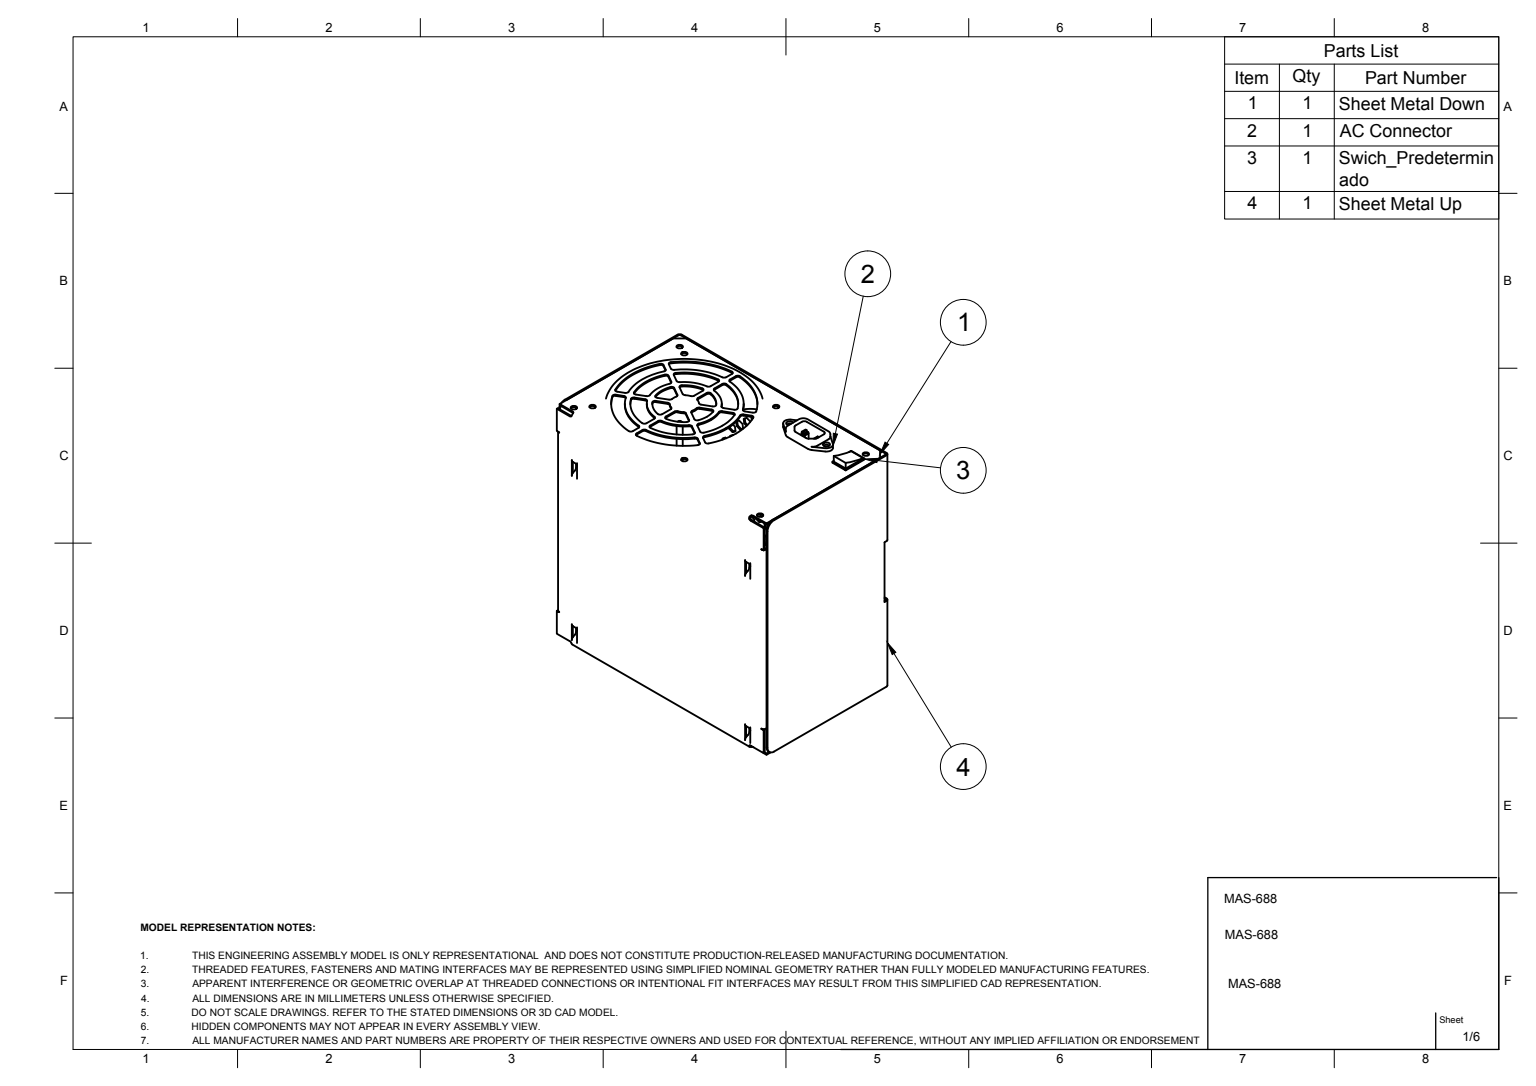
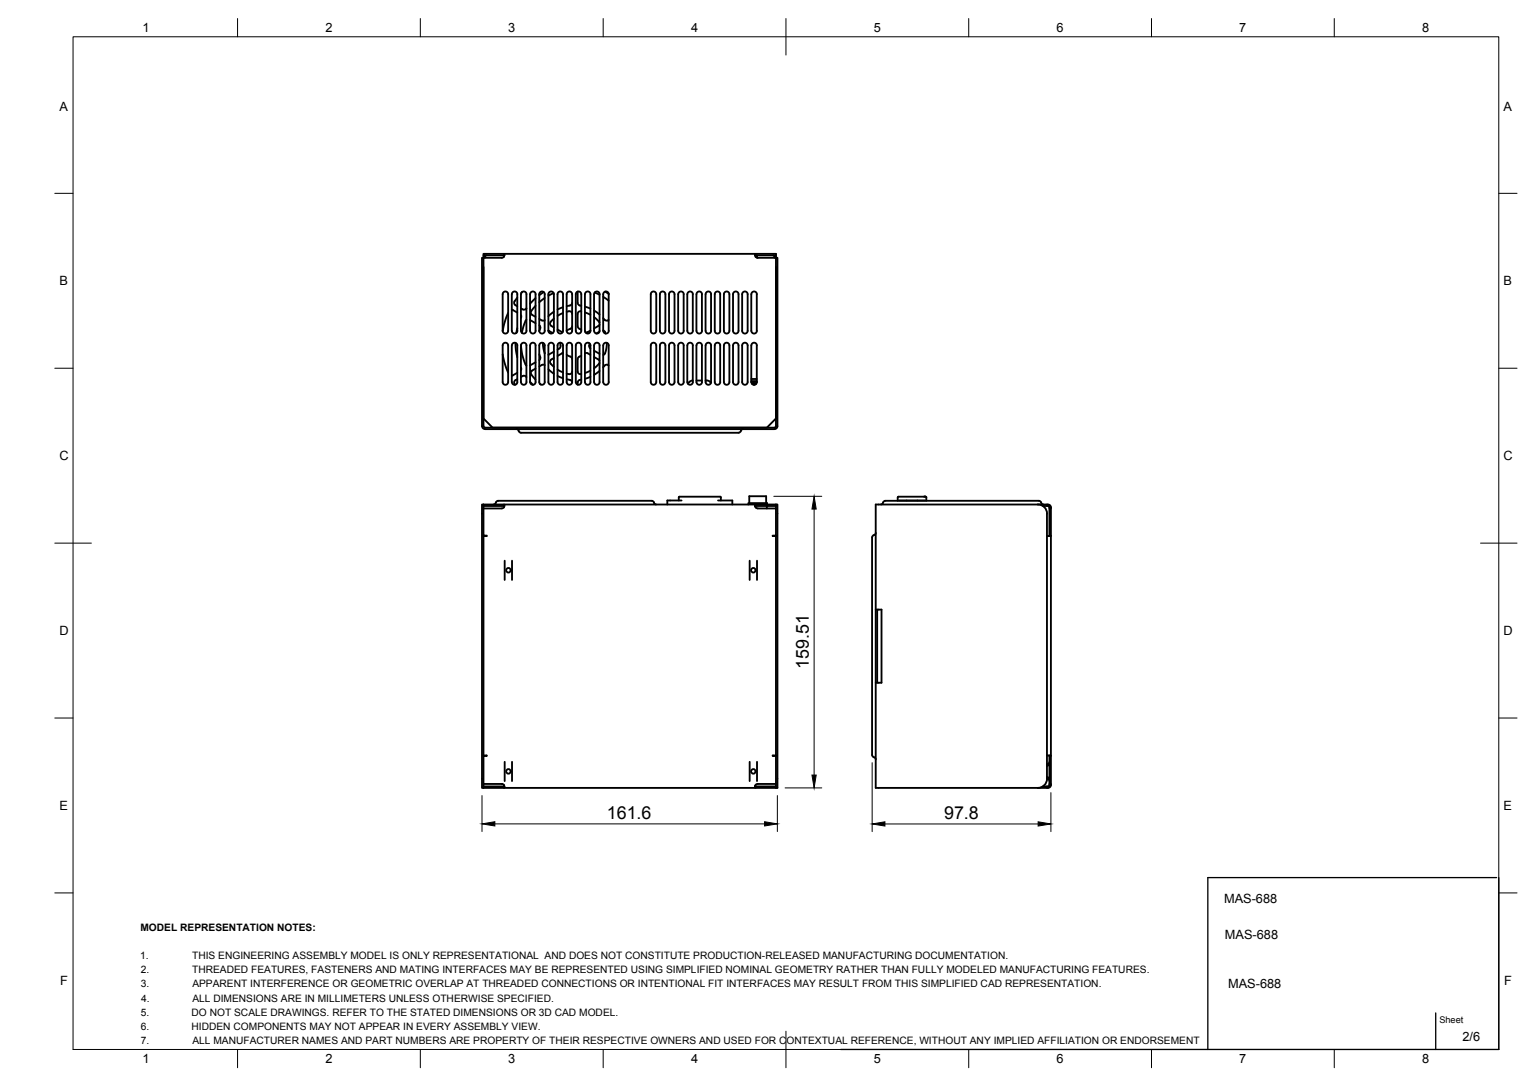
ISO-10303-21;
HEADER;
/* Generated by software containing ST-Developer
 * from STEP Tools, Inc. (www.steptools.com) 
 */

FILE_DESCRIPTION(
/* description */ ('STEP AP214'),
/* implementation_level */ '2;1');

FILE_NAME(
/* name */ 'MAS-688.step',
/* time_stamp */ '2026-11-14T03:58:36-08:00',
/* author */ (''),
/* organization */ (''),
/* preprocessor_version */ 'ST-DEVELOPER v20.2',
/* originating_system */ 'Autodesk Translation Framework v15.17.0.0',
/* authorisation */ '');

FILE_SCHEMA (('AUTOMOTIVE_DESIGN { 1 0 10303 214 3 1 1 }'));
ENDSEC;

DATA;
#10=MECHANICAL_DESIGN_GEOMETRIC_PRESENTATION_REPRESENTATION('',(#41,#42,
#43,#44),#65304);
#11=ITEM_DEFINED_TRANSFORMATION($,$,#39984,#42510);
#12=ITEM_DEFINED_TRANSFORMATION($,$,#41041,#42511);
#13=ITEM_DEFINED_TRANSFORMATION($,$,#41224,#42512);
#14=ITEM_DEFINED_TRANSFORMATION($,$,#41307,#42513);
#15=(
REPRESENTATION_RELATIONSHIP($,$,#65324,#65323)
REPRESENTATION_RELATIONSHIP_WITH_TRANSFORMATION(#11)
SHAPE_REPRESENTATION_RELATIONSHIP()
);
#16=(
REPRESENTATION_RELATIONSHIP($,$,#65325,#65323)
REPRESENTATION_RELATIONSHIP_WITH_TRANSFORMATION(#12)
SHAPE_REPRESENTATION_RELATIONSHIP()
);
#17=(
REPRESENTATION_RELATIONSHIP($,$,#65326,#65323)
REPRESENTATION_RELATIONSHIP_WITH_TRANSFORMATION(#13)
SHAPE_REPRESENTATION_RELATIONSHIP()
);
#18=(
REPRESENTATION_RELATIONSHIP($,$,#65327,#65323)
REPRESENTATION_RELATIONSHIP_WITH_TRANSFORMATION(#14)
SHAPE_REPRESENTATION_RELATIONSHIP()
);
#19=CONTEXT_DEPENDENT_SHAPE_REPRESENTATION(#15,#65319);
#20=CONTEXT_DEPENDENT_SHAPE_REPRESENTATION(#16,#65320);
#21=CONTEXT_DEPENDENT_SHAPE_REPRESENTATION(#17,#65321);
#22=CONTEXT_DEPENDENT_SHAPE_REPRESENTATION(#18,#65322);
#23=NEXT_ASSEMBLY_USAGE_OCCURRENCE('Sheet Metal Down:1',
'Sheet Metal Down:1','Sheet Metal Down:1',#65329,#65330,
'Sheet Metal Down:1');
#24=NEXT_ASSEMBLY_USAGE_OCCURRENCE('AC Connector:1','AC Connector:1',
'AC Connector:1',#65329,#65331,'AC Connector:1');
#25=NEXT_ASSEMBLY_USAGE_OCCURRENCE('Swich_Predeterminado:1',
'Swich_Predeterminado:1','Swich_Predeterminado:1',#65329,#65332,
'Swich_Predeterminado:1');
#26=NEXT_ASSEMBLY_USAGE_OCCURRENCE('Sheet Metal Up:1',
'Sheet Metal Up:1','Sheet Metal Up:1',#65329,#65333,'Sheet Metal Up:1');
#27=SPHERICAL_SURFACE('',#41303,0.5);
#28=SPHERICAL_SURFACE('',#41305,0.5);
#29=ORIENTED_CLOSED_SHELL('',*,#39935,.F.);
#30=BREP_WITH_VOIDS('Body1',#39936,(#29));
#31=CONICAL_SURFACE('',#41051,1.97294590991864,0.71558499331768);
#32=CONICAL_SURFACE('',#41055,1.97294590991864,0.71558499331768);
#33=SHAPE_REPRESENTATION_RELATIONSHIP('SRR','None',#65324,#37);
#34=SHAPE_REPRESENTATION_RELATIONSHIP('SRR','None',#65325,#38);
#35=SHAPE_REPRESENTATION_RELATIONSHIP('SRR','None',#65326,#39);
#36=SHAPE_REPRESENTATION_RELATIONSHIP('SRR','None',#65327,#40);
#37=ADVANCED_BREP_SHAPE_REPRESENTATION('',(#45),#65300);
#38=ADVANCED_BREP_SHAPE_REPRESENTATION('',(#46),#65301);
#39=ADVANCED_BREP_SHAPE_REPRESENTATION('',(#30),#65302);
#40=ADVANCED_BREP_SHAPE_REPRESENTATION('',(#47),#65303);
#41=STYLED_ITEM('',(#65353),#45);
#42=STYLED_ITEM('',(#65354),#46);
#43=STYLED_ITEM('',(#65355),#30);
#44=STYLED_ITEM('',(#65356),#47);
#45=MANIFOLD_SOLID_BREP('Body1',#39933);
#46=MANIFOLD_SOLID_BREP('Body1',#39934);
#47=MANIFOLD_SOLID_BREP('Body1',#39937);
#48=FACE_BOUND('',#4336,.T.);
#49=FACE_BOUND('',#4337,.T.);
#50=FACE_BOUND('',#4338,.T.);
#51=FACE_BOUND('',#4339,.T.);
#52=FACE_BOUND('',#4341,.T.);
#53=FACE_BOUND('',#4342,.T.);
#54=FACE_BOUND('',#4343,.T.);
#55=FACE_BOUND('',#4344,.T.);
#56=FACE_BOUND('',#4348,.T.);
#57=FACE_BOUND('',#4349,.T.);
#58=FACE_BOUND('',#4351,.T.);
#59=FACE_BOUND('',#4352,.T.);
#60=FACE_BOUND('',#4356,.T.);
#61=FACE_BOUND('',#4357,.T.);
#62=FACE_BOUND('',#4358,.T.);
#63=FACE_BOUND('',#4359,.T.);
#64=FACE_BOUND('',#4360,.T.);
#65=FACE_BOUND('',#4361,.T.);
#66=FACE_BOUND('',#4362,.T.);
#67=FACE_BOUND('',#4363,.T.);
#68=FACE_BOUND('',#4364,.T.);
#69=FACE_BOUND('',#4365,.T.);
#70=FACE_BOUND('',#4366,.T.);
#71=FACE_BOUND('',#4367,.T.);
#72=FACE_BOUND('',#4368,.T.);
#73=FACE_BOUND('',#4369,.T.);
#74=FACE_BOUND('',#4370,.T.);
#75=FACE_BOUND('',#4371,.T.);
#76=FACE_BOUND('',#4372,.T.);
#77=FACE_BOUND('',#4373,.T.);
#78=FACE_BOUND('',#4374,.T.);
#79=FACE_BOUND('',#4375,.T.);
#80=FACE_BOUND('',#4376,.T.);
#81=FACE_BOUND('',#4377,.T.);
#82=FACE_BOUND('',#4378,.T.);
#83=FACE_BOUND('',#4379,.T.);
#84=FACE_BOUND('',#4380,.T.);
#85=FACE_BOUND('',#4381,.T.);
#86=FACE_BOUND('',#4382,.T.);
#87=FACE_BOUND('',#4383,.T.);
#88=FACE_BOUND('',#4384,.T.);
#89=FACE_BOUND('',#4385,.T.);
#90=FACE_BOUND('',#4386,.T.);
#91=FACE_BOUND('',#4387,.T.);
#92=FACE_BOUND('',#4388,.T.);
#93=FACE_BOUND('',#4389,.T.);
#94=FACE_BOUND('',#4390,.T.);
#95=FACE_BOUND('',#4391,.T.);
#96=FACE_BOUND('',#4392,.T.);
#97=FACE_BOUND('',#4393,.T.);
#98=FACE_BOUND('',#4394,.T.);
#99=FACE_BOUND('',#4395,.T.);
#100=FACE_BOUND('',#4396,.T.);
#101=FACE_BOUND('',#4397,.T.);
#102=FACE_BOUND('',#4398,.T.);
#103=FACE_BOUND('',#4399,.T.);
#104=FACE_BOUND('',#4400,.T.);
#105=FACE_BOUND('',#4401,.T.);
#106=FACE_BOUND('',#4402,.T.);
#107=FACE_BOUND('',#4403,.T.);
#108=FACE_BOUND('',#4405,.T.);
#109=FACE_BOUND('',#4406,.T.);
#110=FACE_BOUND('',#4407,.T.);
#111=FACE_BOUND('',#4408,.T.);
#112=FACE_BOUND('',#4409,.T.);
#113=FACE_BOUND('',#4410,.T.);
#114=FACE_BOUND('',#4411,.T.);
#115=FACE_BOUND('',#4412,.T.);
#116=FACE_BOUND('',#4413,.T.);
#117=FACE_BOUND('',#4414,.T.);
#118=FACE_BOUND('',#4415,.T.);
#119=FACE_BOUND('',#4416,.T.);
#120=FACE_BOUND('',#4417,.T.);
#121=FACE_BOUND('',#4418,.T.);
#122=FACE_BOUND('',#4419,.T.);
#123=FACE_BOUND('',#4420,.T.);
#124=FACE_BOUND('',#4421,.T.);
#125=FACE_BOUND('',#4422,.T.);
#126=FACE_BOUND('',#4423,.T.);
#127=FACE_BOUND('',#4424,.T.);
#128=FACE_BOUND('',#4425,.T.);
#129=FACE_BOUND('',#4426,.T.);
#130=FACE_BOUND('',#4427,.T.);
#131=FACE_BOUND('',#4428,.T.);
#132=FACE_BOUND('',#4429,.T.);
#133=FACE_BOUND('',#4430,.T.);
#134=FACE_BOUND('',#4431,.T.);
#135=FACE_BOUND('',#4432,.T.);
#136=FACE_BOUND('',#4433,.T.);
#137=FACE_BOUND('',#4434,.T.);
#138=FACE_BOUND('',#4435,.T.);
#139=FACE_BOUND('',#4436,.T.);
#140=FACE_BOUND('',#4437,.T.);
#141=FACE_BOUND('',#4438,.T.);
#142=FACE_BOUND('',#4439,.T.);
#143=FACE_BOUND('',#4440,.T.);
#144=FACE_BOUND('',#4441,.T.);
#145=FACE_BOUND('',#4442,.T.);
#146=FACE_BOUND('',#4443,.T.);
#147=FACE_BOUND('',#4444,.T.);
#148=FACE_BOUND('',#4445,.T.);
#149=FACE_BOUND('',#4446,.T.);
#150=FACE_BOUND('',#4447,.T.);
#151=FACE_BOUND('',#4448,.T.);
#152=FACE_BOUND('',#4449,.T.);
#153=FACE_BOUND('',#4450,.T.);
#154=FACE_BOUND('',#4451,.T.);
#155=FACE_BOUND('',#4452,.T.);
#156=FACE_BOUND('',#4479,.T.);
#157=FACE_BOUND('',#4480,.T.);
#158=FACE_BOUND('',#4481,.T.);
#159=FACE_BOUND('',#4482,.T.);
#160=FACE_BOUND('',#4483,.T.);
#161=FACE_BOUND('',#4484,.T.);
#162=FACE_BOUND('',#4485,.T.);
#163=FACE_BOUND('',#4486,.T.);
#164=FACE_BOUND('',#4487,.T.);
#165=FACE_BOUND('',#4488,.T.);
#166=FACE_BOUND('',#4489,.T.);
#167=FACE_BOUND('',#4490,.T.);
#168=FACE_BOUND('',#4491,.T.);
#169=FACE_BOUND('',#4492,.T.);
#170=FACE_BOUND('',#4493,.T.);
#171=FACE_BOUND('',#4494,.T.);
#172=FACE_BOUND('',#4495,.T.);
#173=FACE_BOUND('',#4496,.T.);
#174=FACE_BOUND('',#4503,.T.);
#175=FACE_BOUND('',#4504,.T.);
#176=FACE_BOUND('',#4505,.T.);
#177=FACE_BOUND('',#4506,.T.);
#178=FACE_BOUND('',#4507,.T.);
#179=FACE_BOUND('',#4508,.T.);
#180=FACE_BOUND('',#4509,.T.);
#181=FACE_BOUND('',#4510,.T.);
#182=FACE_BOUND('',#4511,.T.);
#183=FACE_BOUND('',#4512,.T.);
#184=FACE_BOUND('',#4513,.T.);
#185=FACE_BOUND('',#4515,.T.);
#186=FACE_BOUND('',#4516,.T.);
#187=FACE_BOUND('',#4517,.T.);
#188=FACE_BOUND('',#4518,.T.);
#189=FACE_BOUND('',#4519,.T.);
#190=FACE_BOUND('',#4520,.T.);
#191=FACE_BOUND('',#4521,.T.);
#192=FACE_BOUND('',#4522,.T.);
#193=FACE_BOUND('',#4523,.T.);
#194=FACE_BOUND('',#4524,.T.);
#195=FACE_BOUND('',#4525,.T.);
#196=FACE_BOUND('',#4567,.T.);
#197=FACE_BOUND('',#4575,.T.);
#198=FACE_BOUND('',#4587,.T.);
#199=FACE_BOUND('',#4595,.T.);
#200=FACE_BOUND('',#4607,.T.);
#201=FACE_BOUND('',#4615,.T.);
#202=FACE_BOUND('',#4627,.T.);
#203=FACE_BOUND('',#4635,.T.);
#204=FACE_BOUND('',#4637,.T.);
#205=FACE_BOUND('',#4638,.T.);
#206=FACE_BOUND('',#4639,.T.);
#207=FACE_BOUND('',#4640,.T.);
#208=FACE_BOUND('',#4641,.T.);
#209=FACE_BOUND('',#4642,.T.);
#210=FACE_BOUND('',#4643,.T.);
#211=FACE_BOUND('',#4644,.T.);
#212=FACE_BOUND('',#4645,.T.);
#213=FACE_BOUND('',#4646,.T.);
#214=FACE_BOUND('',#4647,.T.);
#215=FACE_BOUND('',#4648,.T.);
#216=FACE_BOUND('',#4649,.T.);
#217=FACE_BOUND('',#4650,.T.);
#218=FACE_BOUND('',#4651,.T.);
#219=FACE_BOUND('',#4652,.T.);
#220=FACE_BOUND('',#4653,.T.);
#221=FACE_BOUND('',#4654,.T.);
#222=FACE_BOUND('',#4941,.T.);
#223=FACE_BOUND('',#4949,.T.);
#224=FACE_BOUND('',#4961,.T.);
#225=FACE_BOUND('',#4969,.T.);
#226=FACE_BOUND('',#4996,.T.);
#227=FACE_BOUND('',#4997,.T.);
#228=FACE_BOUND('',#4998,.T.);
#229=FACE_BOUND('',#5012,.T.);
#230=FACE_BOUND('',#5013,.T.);
#231=FACE_BOUND('',#5014,.T.);
#232=FACE_BOUND('',#5016,.T.);
#233=FACE_BOUND('',#5018,.T.);
#234=FACE_BOUND('',#5019,.T.);
#235=FACE_BOUND('',#5020,.T.);
#236=FACE_BOUND('',#5033,.T.);
#237=FACE_BOUND('',#5037,.T.);
#238=FACE_BOUND('',#5080,.T.);
#239=FACE_BOUND('',#5090,.T.);
#240=FACE_BOUND('',#5093,.T.);
#241=FACE_BOUND('',#5099,.T.);
#242=FACE_BOUND('',#5106,.T.);
#243=FACE_BOUND('',#5108,.T.);
#244=FACE_BOUND('',#5110,.T.);
#245=FACE_BOUND('',#5121,.T.);
#246=FACE_BOUND('',#5123,.T.);
#247=FACE_BOUND('',#5142,.T.);
#248=FACE_BOUND('',#5143,.T.);
#249=FACE_BOUND('',#5145,.T.);
#250=FACE_BOUND('',#5151,.T.);
#251=FACE_BOUND('',#5167,.T.);
#252=FACE_BOUND('',#5169,.T.);
#253=FACE_BOUND('',#5172,.T.);
#254=FACE_BOUND('',#5174,.T.);
#255=FACE_BOUND('',#5203,.T.);
#256=FACE_BOUND('',#5205,.T.);
#257=FACE_BOUND('',#5251,.T.);
#258=FACE_BOUND('',#5252,.T.);
#259=FACE_BOUND('',#5253,.T.);
#260=FACE_BOUND('',#5254,.T.);
#261=FACE_BOUND('',#5255,.T.);
#262=FACE_BOUND('',#5256,.T.);
#263=FACE_BOUND('',#5257,.T.);
#264=FACE_BOUND('',#5258,.T.);
#265=FACE_BOUND('',#5259,.T.);
#266=FACE_BOUND('',#5260,.T.);
#267=FACE_BOUND('',#5261,.T.);
#268=FACE_BOUND('',#5262,.T.);
#269=FACE_BOUND('',#5263,.T.);
#270=FACE_BOUND('',#5264,.T.);
#271=FACE_BOUND('',#5265,.T.);
#272=FACE_BOUND('',#5266,.T.);
#273=FACE_BOUND('',#5267,.T.);
#274=FACE_BOUND('',#5268,.T.);
#275=FACE_BOUND('',#5269,.T.);
#276=FACE_BOUND('',#5270,.T.);
#277=FACE_BOUND('',#5271,.T.);
#278=FACE_BOUND('',#5272,.T.);
#279=FACE_BOUND('',#5273,.T.);
#280=FACE_BOUND('',#5274,.T.);
#281=FACE_BOUND('',#5275,.T.);
#282=FACE_BOUND('',#5276,.T.);
#283=FACE_BOUND('',#5277,.T.);
#284=FACE_BOUND('',#5278,.T.);
#285=FACE_BOUND('',#5279,.T.);
#286=FACE_BOUND('',#5280,.T.);
#287=FACE_BOUND('',#5281,.T.);
#288=FACE_BOUND('',#5282,.T.);
#289=FACE_BOUND('',#5283,.T.);
#290=FACE_BOUND('',#5284,.T.);
#291=FACE_BOUND('',#5285,.T.);
#292=FACE_BOUND('',#5286,.T.);
#293=FACE_BOUND('',#5287,.T.);
#294=FACE_BOUND('',#5288,.T.);
#295=FACE_BOUND('',#5289,.T.);
#296=FACE_BOUND('',#5290,.T.);
#297=FACE_BOUND('',#5291,.T.);
#298=FACE_BOUND('',#5292,.T.);
#299=FACE_BOUND('',#5293,.T.);
#300=FACE_BOUND('',#5294,.T.);
#301=FACE_BOUND('',#5295,.T.);
#302=FACE_BOUND('',#5296,.T.);
#303=FACE_BOUND('',#5297,.T.);
#304=FACE_BOUND('',#5298,.T.);
#305=FACE_BOUND('',#5299,.T.);
#306=FACE_BOUND('',#5300,.T.);
#307=FACE_BOUND('',#5301,.T.);
#308=FACE_BOUND('',#5302,.T.);
#309=FACE_BOUND('',#5303,.T.);
#310=FACE_BOUND('',#5304,.T.);
#311=FACE_BOUND('',#5305,.T.);
#312=FACE_BOUND('',#5306,.T.);
#313=FACE_BOUND('',#5307,.T.);
#314=FACE_BOUND('',#5308,.T.);
#315=FACE_BOUND('',#5309,.T.);
#316=FACE_BOUND('',#5310,.T.);
#317=FACE_BOUND('',#5311,.T.);
#318=FACE_BOUND('',#5312,.T.);
#319=FACE_BOUND('',#5313,.T.);
#320=FACE_BOUND('',#5314,.T.);
#321=FACE_BOUND('',#5315,.T.);
#322=FACE_BOUND('',#5316,.T.);
#323=FACE_BOUND('',#5317,.T.);
#324=FACE_BOUND('',#5318,.T.);
#325=FACE_BOUND('',#5319,.T.);
#326=FACE_BOUND('',#5320,.T.);
#327=FACE_BOUND('',#5321,.T.);
#328=FACE_BOUND('',#5322,.T.);
#329=FACE_BOUND('',#5323,.T.);
#330=FACE_BOUND('',#5324,.T.);
#331=FACE_BOUND('',#5325,.T.);
#332=FACE_BOUND('',#5326,.T.);
#333=FACE_BOUND('',#5327,.T.);
#334=FACE_BOUND('',#5328,.T.);
#335=FACE_BOUND('',#5329,.T.);
#336=FACE_BOUND('',#5330,.T.);
#337=FACE_BOUND('',#5331,.T.);
#338=FACE_BOUND('',#5332,.T.);
#339=FACE_BOUND('',#5333,.T.);
#340=FACE_BOUND('',#5334,.T.);
#341=FACE_BOUND('',#5335,.T.);
#342=FACE_BOUND('',#5336,.T.);
#343=FACE_BOUND('',#5337,.T.);
#344=FACE_BOUND('',#5338,.T.);
#345=FACE_BOUND('',#5339,.T.);
#346=FACE_BOUND('',#5340,.T.);
#347=FACE_BOUND('',#5341,.T.);
#348=FACE_BOUND('',#5342,.T.);
#349=FACE_BOUND('',#5343,.T.);
#350=FACE_BOUND('',#5344,.T.);
#351=FACE_BOUND('',#5345,.T.);
#352=FACE_BOUND('',#5346,.T.);
#353=FACE_BOUND('',#5347,.T.);
#354=FACE_BOUND('',#5348,.T.);
#355=FACE_BOUND('',#5349,.T.);
#356=FACE_BOUND('',#5350,.T.);
#357=FACE_BOUND('',#5351,.T.);
#358=FACE_BOUND('',#5352,.T.);
#359=FACE_BOUND('',#5353,.T.);
#360=FACE_BOUND('',#5354,.T.);
#361=FACE_BOUND('',#5355,.T.);
#362=FACE_BOUND('',#5356,.T.);
#363=FACE_BOUND('',#5357,.T.);
#364=FACE_BOUND('',#5358,.T.);
#365=FACE_BOUND('',#5359,.T.);
#366=FACE_BOUND('',#5360,.T.);
#367=FACE_BOUND('',#5361,.T.);
#368=FACE_BOUND('',#5362,.T.);
#369=FACE_BOUND('',#5363,.T.);
#370=FACE_BOUND('',#5364,.T.);
#371=FACE_BOUND('',#5365,.T.);
#372=FACE_BOUND('',#5366,.T.);
#373=FACE_BOUND('',#5367,.T.);
#374=FACE_BOUND('',#5368,.T.);
#375=FACE_BOUND('',#5369,.T.);
#376=FACE_BOUND('',#5370,.T.);
#377=FACE_BOUND('',#5371,.T.);
#378=FACE_BOUND('',#5372,.T.);
#379=FACE_BOUND('',#5373,.T.);
#380=FACE_BOUND('',#5374,.T.);
#381=FACE_BOUND('',#5375,.T.);
#382=FACE_BOUND('',#5376,.T.);
#383=FACE_BOUND('',#5377,.T.);
#384=FACE_BOUND('',#5378,.T.);
#385=FACE_BOUND('',#5379,.T.);
#386=FACE_BOUND('',#5380,.T.);
#387=FACE_BOUND('',#5381,.T.);
#388=FACE_BOUND('',#5382,.T.);
#389=FACE_BOUND('',#5383,.T.);
#390=FACE_BOUND('',#5384,.T.);
#391=FACE_BOUND('',#5385,.T.);
#392=FACE_BOUND('',#5386,.T.);
#393=FACE_BOUND('',#5387,.T.);
#394=FACE_BOUND('',#5388,.T.);
#395=FACE_BOUND('',#5389,.T.);
#396=FACE_BOUND('',#5390,.T.);
#397=FACE_BOUND('',#5391,.T.);
#398=FACE_BOUND('',#5392,.T.);
#399=FACE_BOUND('',#5393,.T.);
#400=FACE_BOUND('',#5394,.T.);
#401=FACE_BOUND('',#5395,.T.);
#402=FACE_BOUND('',#5396,.T.);
#403=FACE_BOUND('',#5397,.T.);
#404=FACE_BOUND('',#5398,.T.);
#405=FACE_BOUND('',#5399,.T.);
#406=FACE_BOUND('',#5400,.T.);
#407=FACE_BOUND('',#5401,.T.);
#408=FACE_BOUND('',#5402,.T.);
#409=FACE_BOUND('',#5403,.T.);
#410=FACE_BOUND('',#5404,.T.);
#411=FACE_BOUND('',#5405,.T.);
#412=FACE_BOUND('',#5406,.T.);
#413=FACE_BOUND('',#5407,.T.);
#414=FACE_BOUND('',#5408,.T.);
#415=FACE_BOUND('',#5409,.T.);
#416=FACE_BOUND('',#5410,.T.);
#417=FACE_BOUND('',#5411,.T.);
#418=FACE_BOUND('',#5412,.T.);
#419=FACE_BOUND('',#5413,.T.);
#420=FACE_BOUND('',#5414,.T.);
#421=FACE_BOUND('',#5415,.T.);
#422=FACE_BOUND('',#5416,.T.);
#423=FACE_BOUND('',#5417,.T.);
#424=FACE_BOUND('',#5418,.T.);
#425=FACE_BOUND('',#5419,.T.);
#426=FACE_BOUND('',#5420,.T.);
#427=FACE_BOUND('',#5421,.T.);
#428=FACE_BOUND('',#5422,.T.);
#429=FACE_BOUND('',#5423,.T.);
#430=FACE_BOUND('',#5424,.T.);
#431=FACE_BOUND('',#5425,.T.);
#432=FACE_BOUND('',#5426,.T.);
#433=FACE_BOUND('',#5427,.T.);
#434=FACE_BOUND('',#5428,.T.);
#435=FACE_BOUND('',#5429,.T.);
#436=FACE_BOUND('',#5430,.T.);
#437=FACE_BOUND('',#5431,.T.);
#438=FACE_BOUND('',#5432,.T.);
#439=FACE_BOUND('',#5433,.T.);
#440=FACE_BOUND('',#5434,.T.);
#441=FACE_BOUND('',#5435,.T.);
#442=FACE_BOUND('',#5436,.T.);
#443=FACE_BOUND('',#5438,.T.);
#444=FACE_BOUND('',#5439,.T.);
#445=FACE_BOUND('',#5440,.T.);
#446=FACE_BOUND('',#5441,.T.);
#447=FACE_BOUND('',#5442,.T.);
#448=FACE_BOUND('',#5443,.T.);
#449=FACE_BOUND('',#5444,.T.);
#450=FACE_BOUND('',#5445,.T.);
#451=FACE_BOUND('',#5446,.T.);
#452=FACE_BOUND('',#5447,.T.);
#453=FACE_BOUND('',#5448,.T.);
#454=FACE_BOUND('',#5449,.T.);
#455=FACE_BOUND('',#5450,.T.);
#456=FACE_BOUND('',#5451,.T.);
#457=FACE_BOUND('',#5452,.T.);
#458=FACE_BOUND('',#5453,.T.);
#459=FACE_BOUND('',#5454,.T.);
#460=FACE_BOUND('',#5455,.T.);
#461=FACE_BOUND('',#5456,.T.);
#462=FACE_BOUND('',#5457,.T.);
#463=FACE_BOUND('',#5458,.T.);
#464=FACE_BOUND('',#5459,.T.);
#465=FACE_BOUND('',#5460,.T.);
#466=FACE_BOUND('',#5461,.T.);
#467=FACE_BOUND('',#5462,.T.);
#468=FACE_BOUND('',#5463,.T.);
#469=FACE_BOUND('',#5464,.T.);
#470=FACE_BOUND('',#5465,.T.);
#471=FACE_BOUND('',#5466,.T.);
#472=FACE_BOUND('',#5467,.T.);
#473=FACE_BOUND('',#5468,.T.);
#474=FACE_BOUND('',#5469,.T.);
#475=FACE_BOUND('',#5470,.T.);
#476=FACE_BOUND('',#5471,.T.);
#477=FACE_BOUND('',#5472,.T.);
#478=FACE_BOUND('',#5473,.T.);
#479=FACE_BOUND('',#5474,.T.);
#480=FACE_BOUND('',#5475,.T.);
#481=FACE_BOUND('',#5476,.T.);
#482=FACE_BOUND('',#5477,.T.);
#483=FACE_BOUND('',#5478,.T.);
#484=FACE_BOUND('',#5479,.T.);
#485=FACE_BOUND('',#5480,.T.);
#486=FACE_BOUND('',#5481,.T.);
#487=FACE_BOUND('',#5482,.T.);
#488=FACE_BOUND('',#5483,.T.);
#489=FACE_BOUND('',#5484,.T.);
#490=FACE_BOUND('',#5485,.T.);
#491=FACE_BOUND('',#5486,.T.);
#492=FACE_BOUND('',#5487,.T.);
#493=FACE_BOUND('',#5488,.T.);
#494=FACE_BOUND('',#5489,.T.);
#495=FACE_BOUND('',#5490,.T.);
#496=FACE_BOUND('',#5491,.T.);
#497=FACE_BOUND('',#5492,.T.);
#498=FACE_BOUND('',#5493,.T.);
#499=FACE_BOUND('',#5494,.T.);
#500=FACE_BOUND('',#5495,.T.);
#501=FACE_BOUND('',#5496,.T.);
#502=FACE_BOUND('',#5497,.T.);
#503=FACE_BOUND('',#5498,.T.);
#504=FACE_BOUND('',#5499,.T.);
#505=FACE_BOUND('',#5500,.T.);
#506=FACE_BOUND('',#5501,.T.);
#507=FACE_BOUND('',#5502,.T.);
#508=FACE_BOUND('',#5503,.T.);
#509=FACE_BOUND('',#5504,.T.);
#510=FACE_BOUND('',#5505,.T.);
#511=FACE_BOUND('',#5506,.T.);
#512=FACE_BOUND('',#5507,.T.);
#513=FACE_BOUND('',#5508,.T.);
#514=FACE_BOUND('',#5509,.T.);
#515=FACE_BOUND('',#5510,.T.);
#516=FACE_BOUND('',#5511,.T.);
#517=FACE_BOUND('',#5512,.T.);
#518=FACE_BOUND('',#5513,.T.);
#519=FACE_BOUND('',#5514,.T.);
#520=FACE_BOUND('',#5515,.T.);
#521=FACE_BOUND('',#5516,.T.);
#522=FACE_BOUND('',#5517,.T.);
#523=FACE_BOUND('',#5518,.T.);
#524=FACE_BOUND('',#5519,.T.);
#525=FACE_BOUND('',#5520,.T.);
#526=FACE_BOUND('',#5521,.T.);
#527=FACE_BOUND('',#5522,.T.);
#528=FACE_BOUND('',#5523,.T.);
#529=FACE_BOUND('',#5524,.T.);
#530=FACE_BOUND('',#5525,.T.);
#531=FACE_BOUND('',#5526,.T.);
#532=FACE_BOUND('',#5527,.T.);
#533=FACE_BOUND('',#5528,.T.);
#534=FACE_BOUND('',#5529,.T.);
#535=FACE_BOUND('',#5530,.T.);
#536=FACE_BOUND('',#5531,.T.);
#537=FACE_BOUND('',#5532,.T.);
#538=FACE_BOUND('',#5533,.T.);
#539=FACE_BOUND('',#5534,.T.);
#540=FACE_BOUND('',#5535,.T.);
#541=FACE_BOUND('',#5536,.T.);
#542=FACE_BOUND('',#5537,.T.);
#543=FACE_BOUND('',#5538,.T.);
#544=FACE_BOUND('',#5539,.T.);
#545=FACE_BOUND('',#5540,.T.);
#546=FACE_BOUND('',#5541,.T.);
#547=FACE_BOUND('',#5542,.T.);
#548=FACE_BOUND('',#5543,.T.);
#549=FACE_BOUND('',#5544,.T.);
#550=FACE_BOUND('',#5545,.T.);
#551=FACE_BOUND('',#5546,.T.);
#552=FACE_BOUND('',#5547,.T.);
#553=FACE_BOUND('',#5548,.T.);
#554=FACE_BOUND('',#5549,.T.);
#555=FACE_BOUND('',#5550,.T.);
#556=FACE_BOUND('',#5551,.T.);
#557=FACE_BOUND('',#5552,.T.);
#558=FACE_BOUND('',#5553,.T.);
#559=FACE_BOUND('',#5554,.T.);
#560=FACE_BOUND('',#5555,.T.);
#561=FACE_BOUND('',#5556,.T.);
#562=FACE_BOUND('',#5557,.T.);
#563=FACE_BOUND('',#5558,.T.);
#564=FACE_BOUND('',#5559,.T.);
#565=FACE_BOUND('',#5560,.T.);
#566=FACE_BOUND('',#5561,.T.);
#567=FACE_BOUND('',#5562,.T.);
#568=FACE_BOUND('',#5563,.T.);
#569=FACE_BOUND('',#5564,.T.);
#570=FACE_BOUND('',#5565,.T.);
#571=FACE_BOUND('',#5566,.T.);
#572=FACE_BOUND('',#5567,.T.);
#573=FACE_BOUND('',#5568,.T.);
#574=FACE_BOUND('',#5569,.T.);
#575=FACE_BOUND('',#5570,.T.);
#576=FACE_BOUND('',#5571,.T.);
#577=FACE_BOUND('',#5572,.T.);
#578=FACE_BOUND('',#5573,.T.);
#579=FACE_BOUND('',#5574,.T.);
#580=FACE_BOUND('',#5575,.T.);
#581=FACE_BOUND('',#5576,.T.);
#582=FACE_BOUND('',#5577,.T.);
#583=FACE_BOUND('',#5578,.T.);
#584=FACE_BOUND('',#5579,.T.);
#585=FACE_BOUND('',#5580,.T.);
#586=FACE_BOUND('',#5581,.T.);
#587=FACE_BOUND('',#5582,.T.);
#588=FACE_BOUND('',#5583,.T.);
#589=FACE_BOUND('',#5584,.T.);
#590=FACE_BOUND('',#5585,.T.);
#591=FACE_BOUND('',#5586,.T.);
#592=FACE_BOUND('',#5587,.T.);
#593=FACE_BOUND('',#5588,.T.);
#594=FACE_BOUND('',#5589,.T.);
#595=FACE_BOUND('',#5590,.T.);
#596=FACE_BOUND('',#5591,.T.);
#597=FACE_BOUND('',#5592,.T.);
#598=FACE_BOUND('',#5593,.T.);
#599=FACE_BOUND('',#5594,.T.);
#600=FACE_BOUND('',#5595,.T.);
#601=FACE_BOUND('',#5596,.T.);
#602=FACE_BOUND('',#5597,.T.);
#603=FACE_BOUND('',#5598,.T.);
#604=FACE_BOUND('',#5599,.T.);
#605=FACE_BOUND('',#5600,.T.);
#606=FACE_BOUND('',#5601,.T.);
#607=FACE_BOUND('',#5602,.T.);
#608=FACE_BOUND('',#5603,.T.);
#609=FACE_BOUND('',#5604,.T.);
#610=FACE_BOUND('',#5605,.T.);
#611=FACE_BOUND('',#5606,.T.);
#612=FACE_BOUND('',#5607,.T.);
#613=FACE_BOUND('',#5608,.T.);
#614=FACE_BOUND('',#5609,.T.);
#615=FACE_BOUND('',#5610,.T.);
#616=FACE_BOUND('',#5611,.T.);
#617=FACE_BOUND('',#5612,.T.);
#618=FACE_BOUND('',#5613,.T.);
#619=FACE_BOUND('',#5614,.T.);
#620=FACE_BOUND('',#5615,.T.);
#621=FACE_BOUND('',#5616,.T.);
#622=FACE_BOUND('',#5617,.T.);
#623=FACE_BOUND('',#5618,.T.);
#624=FACE_BOUND('',#5619,.T.);
#625=FACE_BOUND('',#5620,.T.);
#626=FACE_BOUND('',#5621,.T.);
#627=FACE_BOUND('',#5622,.T.);
#628=FACE_BOUND('',#5623,.T.);
#629=PLANE('',#40239);
#630=PLANE('',#40244);
#631=PLANE('',#40249);
#632=PLANE('',#40250);
#633=PLANE('',#40251);
#634=PLANE('',#40254);
#635=PLANE('',#40257);
#636=PLANE('',#40258);
#637=PLANE('',#40259);
#638=PLANE('',#40310);
#639=PLANE('',#40361);
#640=PLANE('',#40362);
#641=PLANE('',#40363);
#642=PLANE('',#40364);
#643=PLANE('',#40365);
#644=PLANE('',#40366);
#645=PLANE('',#40367);
#646=PLANE('',#40368);
#647=PLANE('',#40369);
#648=PLANE('',#40370);
#649=PLANE('',#40371);
#650=PLANE('',#40372);
#651=PLANE('',#40373);
#652=PLANE('',#40374);
#653=PLANE('',#40375);
#654=PLANE('',#40376);
#655=PLANE('',#40377);
#656=PLANE('',#40378);
#657=PLANE('',#40379);
#658=PLANE('',#40380);
#659=PLANE('',#40381);
#660=PLANE('',#40382);
#661=PLANE('',#40383);
#662=PLANE('',#40384);
#663=PLANE('',#40385);
#664=PLANE('',#40440);
#665=PLANE('',#40441);
#666=PLANE('',#40450);
#667=PLANE('',#40460);
#668=PLANE('',#40462);
#669=PLANE('',#40464);
#670=PLANE('',#40466);
#671=PLANE('',#40469);
#672=PLANE('',#40470);
#673=PLANE('',#40471);
#674=PLANE('',#40472);
#675=PLANE('',#40473);
#676=PLANE('',#40478);
#677=PLANE('',#40479);
#678=PLANE('',#40480);
#679=PLANE('',#40481);
#680=PLANE('',#40482);
#681=PLANE('',#40485);
#682=PLANE('',#40488);
#683=PLANE('',#40497);
#684=PLANE('',#40504);
#685=PLANE('',#40513);
#686=PLANE('',#40514);
#687=PLANE('',#40515);
#688=PLANE('',#40520);
#689=PLANE('',#40521);
#690=PLANE('',#40522);
#691=PLANE('',#40523);
#692=PLANE('',#40526);
#693=PLANE('',#40535);
#694=PLANE('',#40542);
#695=PLANE('',#40551);
#696=PLANE('',#40552);
#697=PLANE('',#40553);
#698=PLANE('',#40558);
#699=PLANE('',#40559);
#700=PLANE('',#40560);
#701=PLANE('',#40561);
#702=PLANE('',#40564);
#703=PLANE('',#40573);
#704=PLANE('',#40580);
#705=PLANE('',#40589);
#706=PLANE('',#40590);
#707=PLANE('',#40591);
#708=PLANE('',#40596);
#709=PLANE('',#40597);
#710=PLANE('',#40598);
#711=PLANE('',#40599);
#712=PLANE('',#40602);
#713=PLANE('',#40611);
#714=PLANE('',#40618);
#715=PLANE('',#40627);
#716=PLANE('',#40628);
#717=PLANE('',#40629);
#718=PLANE('',#40634);
#719=PLANE('',#40635);
#720=PLANE('',#40636);
#721=PLANE('',#40637);
#722=PLANE('',#40692);
#723=PLANE('',#40693);
#724=PLANE('',#40694);
#725=PLANE('',#40695);
#726=PLANE('',#40696);
#727=PLANE('',#40697);
#728=PLANE('',#40698);
#729=PLANE('',#40699);
#730=PLANE('',#40700);
#731=PLANE('',#40701);
#732=PLANE('',#40702);
#733=PLANE('',#40758);
#734=PLANE('',#40760);
#735=PLANE('',#40762);
#736=PLANE('',#40764);
#737=PLANE('',#40766);
#738=PLANE('',#40768);
#739=PLANE('',#40769);
#740=PLANE('',#40770);
#741=PLANE('',#40771);
#742=PLANE('',#40772);
#743=PLANE('',#40773);
#744=PLANE('',#40774);
#745=PLANE('',#40775);
#746=PLANE('',#40776);
#747=PLANE('',#40777);
#748=PLANE('',#40779);
#749=PLANE('',#40780);
#750=PLANE('',#40781);
#751=PLANE('',#40783);
#752=PLANE('',#40784);
#753=PLANE('',#40786);
#754=PLANE('',#40788);
#755=PLANE('',#40789);
#756=PLANE('',#40790);
#757=PLANE('',#40792);
#758=PLANE('',#40794);
#759=PLANE('',#40795);
#760=PLANE('',#40797);
#761=PLANE('',#40798);
#762=PLANE('',#40799);
#763=PLANE('',#40801);
#764=PLANE('',#40802);
#765=PLANE('',#40804);
#766=PLANE('',#40805);
#767=PLANE('',#40807);
#768=PLANE('',#40808);
#769=PLANE('',#40810);
#770=PLANE('',#40812);
#771=PLANE('',#40813);
#772=PLANE('',#40815);
#773=PLANE('',#40816);
#774=PLANE('',#40818);
#775=PLANE('',#40819);
#776=PLANE('',#40821);
#777=PLANE('',#40822);
#778=PLANE('',#40824);
#779=PLANE('',#40825);
#780=PLANE('',#40827);
#781=PLANE('',#40828);
#782=PLANE('',#40830);
#783=PLANE('',#40831);
#784=PLANE('',#40832);
#785=PLANE('',#40834);
#786=PLANE('',#40835);
#787=PLANE('',#40837);
#788=PLANE('',#40838);
#789=PLANE('',#40840);
#790=PLANE('',#40841);
#791=PLANE('',#40843);
#792=PLANE('',#40844);
#793=PLANE('',#40846);
#794=PLANE('',#40848);
#795=PLANE('',#40849);
#796=PLANE('',#40851);
#797=PLANE('',#40852);
#798=PLANE('',#40854);
#799=PLANE('',#40855);
#800=PLANE('',#40857);
#801=PLANE('',#40858);
#802=PLANE('',#40860);
#803=PLANE('',#40861);
#804=PLANE('',#40863);
#805=PLANE('',#40864);
#806=PLANE('',#40866);
#807=PLANE('',#40867);
#808=PLANE('',#40869);
#809=PLANE('',#40870);
#810=PLANE('',#40872);
#811=PLANE('',#40873);
#812=PLANE('',#40875);
#813=PLANE('',#40876);
#814=PLANE('',#40878);
#815=PLANE('',#40879);
#816=PLANE('',#40881);
#817=PLANE('',#40882);
#818=PLANE('',#40884);
#819=PLANE('',#40885);
#820=PLANE('',#40887);
#821=PLANE('',#40888);
#822=PLANE('',#40890);
#823=PLANE('',#40891);
#824=PLANE('',#40893);
#825=PLANE('',#40894);
#826=PLANE('',#40896);
#827=PLANE('',#40897);
#828=PLANE('',#40899);
#829=PLANE('',#40900);
#830=PLANE('',#40902);
#831=PLANE('',#40903);
#832=PLANE('',#40905);
#833=PLANE('',#40906);
#834=PLANE('',#40908);
#835=PLANE('',#40909);
#836=PLANE('',#40911);
#837=PLANE('',#40912);
#838=PLANE('',#40914);
#839=PLANE('',#40915);
#840=PLANE('',#40917);
#841=PLANE('',#40918);
#842=PLANE('',#40920);
#843=PLANE('',#40921);
#844=PLANE('',#40922);
#845=PLANE('',#40923);
#846=PLANE('',#40924);
#847=PLANE('',#40925);
#848=PLANE('',#40926);
#849=PLANE('',#40927);
#850=PLANE('',#40930);
#851=PLANE('',#40935);
#852=PLANE('',#40936);
#853=PLANE('',#40938);
#854=PLANE('',#40940);
#855=PLANE('',#40943);
#856=PLANE('',#40952);
#857=PLANE('',#40959);
#858=PLANE('',#40968);
#859=PLANE('',#40969);
#860=PLANE('',#40970);
#861=PLANE('',#40975);
#862=PLANE('',#40976);
#863=PLANE('',#40977);
#864=PLANE('',#40978);
#865=PLANE('',#40981);
#866=PLANE('',#40990);
#867=PLANE('',#40997);
#868=PLANE('',#41006);
#869=PLANE('',#41007);
#870=PLANE('',#41008);
#871=PLANE('',#41013);
#872=PLANE('',#41014);
#873=PLANE('',#41015);
#874=PLANE('',#41016);
#875=PLANE('',#41017);
#876=PLANE('',#41018);
#877=PLANE('',#41019);
#878=PLANE('',#41020);
#879=PLANE('',#41021);
#880=PLANE('',#41022);
#881=PLANE('',#41025);
#882=PLANE('',#41030);
#883=PLANE('',#41031);
#884=PLANE('',#41032);
#885=PLANE('',#41035);
#886=PLANE('',#41039);
#887=PLANE('',#41066);
#888=PLANE('',#41073);
#889=PLANE('',#41074);
#890=PLANE('',#41075);
#891=PLANE('',#41076);
#892=PLANE('',#41077);
#893=PLANE('',#41078);
#894=PLANE('',#41079);
#895=PLANE('',#41080);
#896=PLANE('',#41081);
#897=PLANE('',#41082);
#898=PLANE('',#41083);
#899=PLANE('',#41084);
#900=PLANE('',#41085);
#901=PLANE('',#41092);
#902=PLANE('',#41103);
#903=PLANE('',#41118);
#904=PLANE('',#41122);
#905=PLANE('',#41126);
#906=PLANE('',#41130);
#907=PLANE('',#41131);
#908=PLANE('',#41134);
#909=PLANE('',#41135);
#910=PLANE('',#41136);
#911=PLANE('',#41137);
#912=PLANE('',#41138);
#913=PLANE('',#41156);
#914=PLANE('',#41158);
#915=PLANE('',#41160);
#916=PLANE('',#41162);
#917=PLANE('',#41164);
#918=PLANE('',#41166);
#919=PLANE('',#41168);
#920=PLANE('',#41170);
#921=PLANE('',#41172);
#922=PLANE('',#41174);
#923=PLANE('',#41176);
#924=PLANE('',#41178);
#925=PLANE('',#41179);
#926=PLANE('',#41180);
#927=PLANE('',#41181);
#928=PLANE('',#41182);
#929=PLANE('',#41183);
#930=PLANE('',#41184);
#931=PLANE('',#41185);
#932=PLANE('',#41186);
#933=PLANE('',#41187);
#934=PLANE('',#41188);
#935=PLANE('',#41189);
#936=PLANE('',#41190);
#937=PLANE('',#41191);
#938=PLANE('',#41192);
#939=PLANE('',#41193);
#940=PLANE('',#41194);
#941=PLANE('',#41195);
#942=PLANE('',#41196);
#943=PLANE('',#41197);
#944=PLANE('',#41198);
#945=PLANE('',#41199);
#946=PLANE('',#41200);
#947=PLANE('',#41201);
#948=PLANE('',#41202);
#949=PLANE('',#41203);
#950=PLANE('',#41204);
#951=PLANE('',#41205);
#952=PLANE('',#41206);
#953=PLANE('',#41207);
#954=PLANE('',#41208);
#955=PLANE('',#41209);
#956=PLANE('',#41210);
#957=PLANE('',#41211);
#958=PLANE('',#41212);
#959=PLANE('',#41213);
#960=PLANE('',#41214);
#961=PLANE('',#41215);
#962=PLANE('',#41216);
#963=PLANE('',#41217);
#964=PLANE('',#41218);
#965=PLANE('',#41219);
#966=PLANE('',#41220);
#967=PLANE('',#41221);
#968=PLANE('',#41222);
#969=PLANE('',#41223);
#970=PLANE('',#41225);
#971=PLANE('',#41226);
#972=PLANE('',#41227);
#973=PLANE('',#41228);
#974=PLANE('',#41229);
#975=PLANE('',#41230);
#976=PLANE('',#41240);
#977=PLANE('',#41241);
#978=PLANE('',#41242);
#979=PLANE('',#41243);
#980=PLANE('',#41244);
#981=PLANE('',#41245);
#982=PLANE('',#41246);
#983=PLANE('',#41247);
#984=PLANE('',#41248);
#985=PLANE('',#41249);
#986=PLANE('',#41250);
#987=PLANE('',#41251);
#988=PLANE('',#41252);
#989=PLANE('',#41253);
#990=PLANE('',#41254);
#991=PLANE('',#41255);
#992=PLANE('',#41258);
#993=PLANE('',#41259);
#994=PLANE('',#41262);
#995=PLANE('',#41263);
#996=PLANE('',#41264);
#997=PLANE('',#41265);
#998=PLANE('',#41266);
#999=PLANE('',#41267);
#1000=PLANE('',#41268);
#1001=PLANE('',#41269);
#1002=PLANE('',#41270);
#1003=PLANE('',#41271);
#1004=PLANE('',#41272);
#1005=PLANE('',#41273);
#1006=PLANE('',#41275);
#1007=PLANE('',#41277);
#1008=PLANE('',#41278);
#1009=PLANE('',#41280);
#1010=PLANE('',#41282);
#1011=PLANE('',#41283);
#1012=PLANE('',#41284);
#1013=PLANE('',#41285);
#1014=PLANE('',#41286);
#1015=PLANE('',#41289);
#1016=PLANE('',#41290);
#1017=PLANE('',#41291);
#1018=PLANE('',#41292);
#1019=PLANE('',#41293);
#1020=PLANE('',#41294);
#1021=PLANE('',#41295);
#1022=PLANE('',#41296);
#1023=PLANE('',#41297);
#1024=PLANE('',#41298);
#1025=PLANE('',#41299);
#1026=PLANE('',#41300);
#1027=PLANE('',#41301);
#1028=PLANE('',#41302);
#1029=PLANE('',#41322);
#1030=PLANE('',#41323);
#1031=PLANE('',#41324);
#1032=PLANE('',#41325);
#1033=PLANE('',#41326);
#1034=PLANE('',#41327);
#1035=PLANE('',#41328);
#1036=PLANE('',#41329);
#1037=PLANE('',#41330);
#1038=PLANE('',#41331);
#1039=PLANE('',#41332);
#1040=PLANE('',#41335);
#1041=PLANE('',#41340);
#1042=PLANE('',#41343);
#1043=PLANE('',#41351);
#1044=PLANE('',#41355);
#1045=PLANE('',#41356);
#1046=PLANE('',#41357);
#1047=PLANE('',#41358);
#1048=PLANE('',#41359);
#1049=PLANE('',#41360);
#1050=PLANE('',#41361);
#1051=PLANE('',#41362);
#1052=PLANE('',#41365);
#1053=PLANE('',#41370);
#1054=PLANE('',#41373);
#1055=PLANE('',#41381);
#1056=PLANE('',#41385);
#1057=PLANE('',#41386);
#1058=PLANE('',#41387);
#1059=PLANE('',#41388);
#1060=PLANE('',#41389);
#1061=PLANE('',#41390);
#1062=PLANE('',#41391);
#1063=PLANE('',#41392);
#1064=PLANE('',#41393);
#1065=PLANE('',#41394);
#1066=PLANE('',#41395);
#1067=PLANE('',#41396);
#1068=PLANE('',#41397);
#1069=PLANE('',#41398);
#1070=PLANE('',#41399);
#1071=PLANE('',#41400);
#1072=PLANE('',#41401);
#1073=PLANE('',#41402);
#1074=PLANE('',#41403);
#1075=PLANE('',#41404);
#1076=PLANE('',#41405);
#1077=PLANE('',#41406);
#1078=PLANE('',#41407);
#1079=PLANE('',#41408);
#1080=PLANE('',#41409);
#1081=PLANE('',#41410);
#1082=PLANE('',#41411);
#1083=PLANE('',#41412);
#1084=PLANE('',#41413);
#1085=PLANE('',#41414);
#1086=PLANE('',#41415);
#1087=PLANE('',#41416);
#1088=PLANE('',#41417);
#1089=PLANE('',#41418);
#1090=PLANE('',#41419);
#1091=PLANE('',#41420);
#1092=PLANE('',#41421);
#1093=PLANE('',#41422);
#1094=PLANE('',#41423);
#1095=PLANE('',#41424);
#1096=PLANE('',#41425);
#1097=PLANE('',#41426);
#1098=PLANE('',#41427);
#1099=PLANE('',#41428);
#1100=PLANE('',#41429);
#1101=PLANE('',#41430);
#1102=PLANE('',#41431);
#1103=PLANE('',#41432);
#1104=PLANE('',#41433);
#1105=PLANE('',#41434);
#1106=PLANE('',#41435);
#1107=PLANE('',#41436);
#1108=PLANE('',#41437);
#1109=PLANE('',#41438);
#1110=PLANE('',#41439);
#1111=PLANE('',#41440);
#1112=PLANE('',#41441);
#1113=PLANE('',#41442);
#1114=PLANE('',#41443);
#1115=PLANE('',#41444);
#1116=PLANE('',#41445);
#1117=PLANE('',#41446);
#1118=PLANE('',#41447);
#1119=PLANE('',#41448);
#1120=PLANE('',#41449);
#1121=PLANE('',#41450);
#1122=PLANE('',#41451);
#1123=PLANE('',#41452);
#1124=PLANE('',#41453);
#1125=PLANE('',#41454);
#1126=PLANE('',#41455);
#1127=PLANE('',#41456);
#1128=PLANE('',#41457);
#1129=PLANE('',#41458);
#1130=PLANE('',#41459);
#1131=PLANE('',#41460);
#1132=PLANE('',#41461);
#1133=PLANE('',#41462);
#1134=PLANE('',#41463);
#1135=PLANE('',#41464);
#1136=PLANE('',#41465);
#1137=PLANE('',#41466);
#1138=PLANE('',#41467);
#1139=PLANE('',#41468);
#1140=PLANE('',#41469);
#1141=PLANE('',#41470);
#1142=PLANE('',#41471);
#1143=PLANE('',#41472);
#1144=PLANE('',#41473);
#1145=PLANE('',#41474);
#1146=PLANE('',#41475);
#1147=PLANE('',#41476);
#1148=PLANE('',#41477);
#1149=PLANE('',#41478);
#1150=PLANE('',#41479);
#1151=PLANE('',#41480);
#1152=PLANE('',#41481);
#1153=PLANE('',#41482);
#1154=PLANE('',#41483);
#1155=PLANE('',#41484);
#1156=PLANE('',#41485);
#1157=PLANE('',#41486);
#1158=PLANE('',#41487);
#1159=PLANE('',#41488);
#1160=PLANE('',#41489);
#1161=PLANE('',#41490);
#1162=PLANE('',#41491);
#1163=PLANE('',#41492);
#1164=PLANE('',#41493);
#1165=PLANE('',#41494);
#1166=PLANE('',#41495);
#1167=PLANE('',#41496);
#1168=PLANE('',#41497);
#1169=PLANE('',#41498);
#1170=PLANE('',#41499);
#1171=PLANE('',#41500);
#1172=PLANE('',#41501);
#1173=PLANE('',#41502);
#1174=PLANE('',#41503);
#1175=PLANE('',#41504);
#1176=PLANE('',#41505);
#1177=PLANE('',#41506);
#1178=PLANE('',#41507);
#1179=PLANE('',#41508);
#1180=PLANE('',#41509);
#1181=PLANE('',#41510);
#1182=PLANE('',#41511);
#1183=PLANE('',#41512);
#1184=PLANE('',#41513);
#1185=PLANE('',#41514);
#1186=PLANE('',#41515);
#1187=PLANE('',#41516);
#1188=PLANE('',#41517);
#1189=PLANE('',#41518);
#1190=PLANE('',#41519);
#1191=PLANE('',#41520);
#1192=PLANE('',#41521);
#1193=PLANE('',#41522);
#1194=PLANE('',#41523);
#1195=PLANE('',#41524);
#1196=PLANE('',#41525);
#1197=PLANE('',#41526);
#1198=PLANE('',#41527);
#1199=PLANE('',#41528);
#1200=PLANE('',#41529);
#1201=PLANE('',#41530);
#1202=PLANE('',#41531);
#1203=PLANE('',#41532);
#1204=PLANE('',#41533);
#1205=PLANE('',#41534);
#1206=PLANE('',#41535);
#1207=PLANE('',#41536);
#1208=PLANE('',#41537);
#1209=PLANE('',#41538);
#1210=PLANE('',#41539);
#1211=PLANE('',#41540);
#1212=PLANE('',#41541);
#1213=PLANE('',#41542);
#1214=PLANE('',#41543);
#1215=PLANE('',#41544);
#1216=PLANE('',#41545);
#1217=PLANE('',#41546);
#1218=PLANE('',#41547);
#1219=PLANE('',#41548);
#1220=PLANE('',#41549);
#1221=PLANE('',#41550);
#1222=PLANE('',#41551);
#1223=PLANE('',#41552);
#1224=PLANE('',#41553);
#1225=PLANE('',#41554);
#1226=PLANE('',#41555);
#1227=PLANE('',#41556);
#1228=PLANE('',#41557);
#1229=PLANE('',#41558);
#1230=PLANE('',#41559);
#1231=PLANE('',#41560);
#1232=PLANE('',#41561);
#1233=PLANE('',#41562);
#1234=PLANE('',#41563);
#1235=PLANE('',#41564);
#1236=PLANE('',#41565);
#1237=PLANE('',#41566);
#1238=PLANE('',#41567);
#1239=PLANE('',#41568);
#1240=PLANE('',#41569);
#1241=PLANE('',#41570);
#1242=PLANE('',#41571);
#1243=PLANE('',#41572);
#1244=PLANE('',#41573);
#1245=PLANE('',#41574);
#1246=PLANE('',#41575);
#1247=PLANE('',#41576);
#1248=PLANE('',#41577);
#1249=PLANE('',#41578);
#1250=PLANE('',#41579);
#1251=PLANE('',#41580);
#1252=PLANE('',#41581);
#1253=PLANE('',#41582);
#1254=PLANE('',#41583);
#1255=PLANE('',#41584);
#1256=PLANE('',#41585);
#1257=PLANE('',#41586);
#1258=PLANE('',#41587);
#1259=PLANE('',#41588);
#1260=PLANE('',#41589);
#1261=PLANE('',#41590);
#1262=PLANE('',#41591);
#1263=PLANE('',#41592);
#1264=PLANE('',#41593);
#1265=PLANE('',#41594);
#1266=PLANE('',#41595);
#1267=PLANE('',#41596);
#1268=PLANE('',#41597);
#1269=PLANE('',#41598);
#1270=PLANE('',#41599);
#1271=PLANE('',#41600);
#1272=PLANE('',#41601);
#1273=PLANE('',#41602);
#1274=PLANE('',#41603);
#1275=PLANE('',#41604);
#1276=PLANE('',#41605);
#1277=PLANE('',#41606);
#1278=PLANE('',#41607);
#1279=PLANE('',#41608);
#1280=PLANE('',#41609);
#1281=PLANE('',#41610);
#1282=PLANE('',#41611);
#1283=PLANE('',#41612);
#1284=PLANE('',#41613);
#1285=PLANE('',#41614);
#1286=PLANE('',#41615);
#1287=PLANE('',#41616);
#1288=PLANE('',#41617);
#1289=PLANE('',#41618);
#1290=PLANE('',#41619);
#1291=PLANE('',#41620);
#1292=PLANE('',#41621);
#1293=PLANE('',#41622);
#1294=PLANE('',#41623);
#1295=PLANE('',#41624);
#1296=PLANE('',#41625);
#1297=PLANE('',#41626);
#1298=PLANE('',#41627);
#1299=PLANE('',#41628);
#1300=PLANE('',#41629);
#1301=PLANE('',#41630);
#1302=PLANE('',#41631);
#1303=PLANE('',#41632);
#1304=PLANE('',#41633);
#1305=PLANE('',#41634);
#1306=PLANE('',#41635);
#1307=PLANE('',#41636);
#1308=PLANE('',#41637);
#1309=PLANE('',#41638);
#1310=PLANE('',#41639);
#1311=PLANE('',#41640);
#1312=PLANE('',#41641);
#1313=PLANE('',#41642);
#1314=PLANE('',#41643);
#1315=PLANE('',#41644);
#1316=PLANE('',#41645);
#1317=PLANE('',#41646);
#1318=PLANE('',#41647);
#1319=PLANE('',#41648);
#1320=PLANE('',#41649);
#1321=PLANE('',#41650);
#1322=PLANE('',#41651);
#1323=PLANE('',#41652);
#1324=PLANE('',#41653);
#1325=PLANE('',#41654);
#1326=PLANE('',#41655);
#1327=PLANE('',#41656);
#1328=PLANE('',#41657);
#1329=PLANE('',#41658);
#1330=PLANE('',#41659);
#1331=PLANE('',#41660);
#1332=PLANE('',#41661);
#1333=PLANE('',#41662);
#1334=PLANE('',#41663);
#1335=PLANE('',#41664);
#1336=PLANE('',#41665);
#1337=PLANE('',#41666);
#1338=PLANE('',#41667);
#1339=PLANE('',#41668);
#1340=PLANE('',#41669);
#1341=PLANE('',#41670);
#1342=PLANE('',#41671);
#1343=PLANE('',#41672);
#1344=PLANE('',#41673);
#1345=PLANE('',#41674);
#1346=PLANE('',#41675);
#1347=PLANE('',#41676);
#1348=PLANE('',#41677);
#1349=PLANE('',#41678);
#1350=PLANE('',#41679);
#1351=PLANE('',#41680);
#1352=PLANE('',#41681);
#1353=PLANE('',#41682);
#1354=PLANE('',#41683);
#1355=PLANE('',#41684);
#1356=PLANE('',#41685);
#1357=PLANE('',#41686);
#1358=PLANE('',#41687);
#1359=PLANE('',#41688);
#1360=PLANE('',#41689);
#1361=PLANE('',#41690);
#1362=PLANE('',#41691);
#1363=PLANE('',#41692);
#1364=PLANE('',#41693);
#1365=PLANE('',#41694);
#1366=PLANE('',#41695);
#1367=PLANE('',#41696);
#1368=PLANE('',#41697);
#1369=PLANE('',#41698);
#1370=PLANE('',#41699);
#1371=PLANE('',#41700);
#1372=PLANE('',#41701);
#1373=PLANE('',#41702);
#1374=PLANE('',#41703);
#1375=PLANE('',#41704);
#1376=PLANE('',#41705);
#1377=PLANE('',#41706);
#1378=PLANE('',#41707);
#1379=PLANE('',#41708);
#1380=PLANE('',#41709);
#1381=PLANE('',#41710);
#1382=PLANE('',#41711);
#1383=PLANE('',#41712);
#1384=PLANE('',#41713);
#1385=PLANE('',#41714);
#1386=PLANE('',#41715);
#1387=PLANE('',#41716);
#1388=PLANE('',#41717);
#1389=PLANE('',#41718);
#1390=PLANE('',#41719);
#1391=PLANE('',#41720);
#1392=PLANE('',#41721);
#1393=PLANE('',#41722);
#1394=PLANE('',#41723);
#1395=PLANE('',#41724);
#1396=PLANE('',#41725);
#1397=PLANE('',#41726);
#1398=PLANE('',#41727);
#1399=PLANE('',#41728);
#1400=PLANE('',#41729);
#1401=PLANE('',#41730);
#1402=PLANE('',#41731);
#1403=PLANE('',#41732);
#1404=PLANE('',#41733);
#1405=PLANE('',#41734);
#1406=PLANE('',#41735);
#1407=PLANE('',#41736);
#1408=PLANE('',#41737);
#1409=PLANE('',#41738);
#1410=PLANE('',#41739);
#1411=PLANE('',#41740);
#1412=PLANE('',#41741);
#1413=PLANE('',#41742);
#1414=PLANE('',#41743);
#1415=PLANE('',#41744);
#1416=PLANE('',#41745);
#1417=PLANE('',#41746);
#1418=PLANE('',#41747);
#1419=PLANE('',#41748);
#1420=PLANE('',#41749);
#1421=PLANE('',#41750);
#1422=PLANE('',#41751);
#1423=PLANE('',#41752);
#1424=PLANE('',#41753);
#1425=PLANE('',#41754);
#1426=PLANE('',#41755);
#1427=PLANE('',#41756);
#1428=PLANE('',#41757);
#1429=PLANE('',#41758);
#1430=PLANE('',#41759);
#1431=PLANE('',#41760);
#1432=PLANE('',#41761);
#1433=PLANE('',#41762);
#1434=PLANE('',#41763);
#1435=PLANE('',#41764);
#1436=PLANE('',#41765);
#1437=PLANE('',#41766);
#1438=PLANE('',#41767);
#1439=PLANE('',#41768);
#1440=PLANE('',#41769);
#1441=PLANE('',#41770);
#1442=PLANE('',#41771);
#1443=PLANE('',#41772);
#1444=PLANE('',#41773);
#1445=PLANE('',#41774);
#1446=PLANE('',#41775);
#1447=PLANE('',#41776);
#1448=PLANE('',#41777);
#1449=PLANE('',#41778);
#1450=PLANE('',#41779);
#1451=PLANE('',#41780);
#1452=PLANE('',#41781);
#1453=PLANE('',#41782);
#1454=PLANE('',#41783);
#1455=PLANE('',#41784);
#1456=PLANE('',#41785);
#1457=PLANE('',#41786);
#1458=PLANE('',#41787);
#1459=PLANE('',#41788);
#1460=PLANE('',#41789);
#1461=PLANE('',#41790);
#1462=PLANE('',#41791);
#1463=PLANE('',#41792);
#1464=PLANE('',#41793);
#1465=PLANE('',#41794);
#1466=PLANE('',#41795);
#1467=PLANE('',#41796);
#1468=PLANE('',#41797);
#1469=PLANE('',#41798);
#1470=PLANE('',#41799);
#1471=PLANE('',#41800);
#1472=PLANE('',#41801);
#1473=PLANE('',#41802);
#1474=PLANE('',#41803);
#1475=PLANE('',#41804);
#1476=PLANE('',#41805);
#1477=PLANE('',#41806);
#1478=PLANE('',#41807);
#1479=PLANE('',#41808);
#1480=PLANE('',#41809);
#1481=PLANE('',#41810);
#1482=PLANE('',#41811);
#1483=PLANE('',#41812);
#1484=PLANE('',#41813);
#1485=PLANE('',#41814);
#1486=PLANE('',#41815);
#1487=PLANE('',#41816);
#1488=PLANE('',#41817);
#1489=PLANE('',#41818);
#1490=PLANE('',#41819);
#1491=PLANE('',#41820);
#1492=PLANE('',#41821);
#1493=PLANE('',#41822);
#1494=PLANE('',#41823);
#1495=PLANE('',#41824);
#1496=PLANE('',#41825);
#1497=PLANE('',#41826);
#1498=PLANE('',#41827);
#1499=PLANE('',#41828);
#1500=PLANE('',#41829);
#1501=PLANE('',#41830);
#1502=PLANE('',#41831);
#1503=PLANE('',#41832);
#1504=PLANE('',#41833);
#1505=PLANE('',#41834);
#1506=PLANE('',#41835);
#1507=PLANE('',#41836);
#1508=PLANE('',#41837);
#1509=PLANE('',#41838);
#1510=PLANE('',#41839);
#1511=PLANE('',#41840);
#1512=PLANE('',#41841);
#1513=PLANE('',#41842);
#1514=PLANE('',#41843);
#1515=PLANE('',#41844);
#1516=PLANE('',#41845);
#1517=PLANE('',#41846);
#1518=PLANE('',#41847);
#1519=PLANE('',#41848);
#1520=PLANE('',#41849);
#1521=PLANE('',#41850);
#1522=PLANE('',#41851);
#1523=PLANE('',#41852);
#1524=PLANE('',#41853);
#1525=PLANE('',#41854);
#1526=PLANE('',#41855);
#1527=PLANE('',#41856);
#1528=PLANE('',#41857);
#1529=PLANE('',#41858);
#1530=PLANE('',#41859);
#1531=PLANE('',#41860);
#1532=PLANE('',#41861);
#1533=PLANE('',#41862);
#1534=PLANE('',#41863);
#1535=PLANE('',#41864);
#1536=PLANE('',#41865);
#1537=PLANE('',#41866);
#1538=PLANE('',#41867);
#1539=PLANE('',#41868);
#1540=PLANE('',#41869);
#1541=PLANE('',#41870);
#1542=PLANE('',#41871);
#1543=PLANE('',#41872);
#1544=PLANE('',#41873);
#1545=PLANE('',#41874);
#1546=PLANE('',#41875);
#1547=PLANE('',#41876);
#1548=PLANE('',#41877);
#1549=PLANE('',#41878);
#1550=PLANE('',#41879);
#1551=PLANE('',#41880);
#1552=PLANE('',#41881);
#1553=PLANE('',#41882);
#1554=PLANE('',#41883);
#1555=PLANE('',#41884);
#1556=PLANE('',#41885);
#1557=PLANE('',#41886);
#1558=PLANE('',#41887);
#1559=PLANE('',#41888);
#1560=PLANE('',#41889);
#1561=PLANE('',#41890);
#1562=PLANE('',#41891);
#1563=PLANE('',#41892);
#1564=PLANE('',#41893);
#1565=PLANE('',#41894);
#1566=PLANE('',#41895);
#1567=PLANE('',#41896);
#1568=PLANE('',#41897);
#1569=PLANE('',#41898);
#1570=PLANE('',#41899);
#1571=PLANE('',#41900);
#1572=PLANE('',#41901);
#1573=PLANE('',#41902);
#1574=PLANE('',#41903);
#1575=PLANE('',#41904);
#1576=PLANE('',#41905);
#1577=PLANE('',#41906);
#1578=PLANE('',#41907);
#1579=PLANE('',#41908);
#1580=PLANE('',#41909);
#1581=PLANE('',#41910);
#1582=PLANE('',#41911);
#1583=PLANE('',#41912);
#1584=PLANE('',#41913);
#1585=PLANE('',#41914);
#1586=PLANE('',#41915);
#1587=PLANE('',#41916);
#1588=PLANE('',#41917);
#1589=PLANE('',#41918);
#1590=PLANE('',#41919);
#1591=PLANE('',#41920);
#1592=PLANE('',#41921);
#1593=PLANE('',#41922);
#1594=PLANE('',#41923);
#1595=PLANE('',#41924);
#1596=PLANE('',#41925);
#1597=PLANE('',#41926);
#1598=PLANE('',#41927);
#1599=PLANE('',#41928);
#1600=PLANE('',#41929);
#1601=PLANE('',#41930);
#1602=PLANE('',#41931);
#1603=PLANE('',#41932);
#1604=PLANE('',#41933);
#1605=PLANE('',#41934);
#1606=PLANE('',#41935);
#1607=PLANE('',#41936);
#1608=PLANE('',#41937);
#1609=PLANE('',#41938);
#1610=PLANE('',#41939);
#1611=PLANE('',#41940);
#1612=PLANE('',#41941);
#1613=PLANE('',#41942);
#1614=PLANE('',#41943);
#1615=PLANE('',#41944);
#1616=PLANE('',#41945);
#1617=PLANE('',#41946);
#1618=PLANE('',#41947);
#1619=PLANE('',#41948);
#1620=PLANE('',#41949);
#1621=PLANE('',#41950);
#1622=PLANE('',#41951);
#1623=PLANE('',#41952);
#1624=PLANE('',#41953);
#1625=PLANE('',#41954);
#1626=PLANE('',#41955);
#1627=PLANE('',#41956);
#1628=PLANE('',#41957);
#1629=PLANE('',#41958);
#1630=PLANE('',#41959);
#1631=PLANE('',#41960);
#1632=PLANE('',#41961);
#1633=PLANE('',#41962);
#1634=PLANE('',#41963);
#1635=PLANE('',#41964);
#1636=PLANE('',#41965);
#1637=PLANE('',#41966);
#1638=PLANE('',#41967);
#1639=PLANE('',#41968);
#1640=PLANE('',#41969);
#1641=PLANE('',#41970);
#1642=PLANE('',#41971);
#1643=PLANE('',#41972);
#1644=PLANE('',#41973);
#1645=PLANE('',#41974);
#1646=PLANE('',#41975);
#1647=PLANE('',#41976);
#1648=PLANE('',#41977);
#1649=PLANE('',#41978);
#1650=PLANE('',#41979);
#1651=PLANE('',#41980);
#1652=PLANE('',#41981);
#1653=PLANE('',#41982);
#1654=PLANE('',#41983);
#1655=PLANE('',#41984);
#1656=PLANE('',#41985);
#1657=PLANE('',#41986);
#1658=PLANE('',#41987);
#1659=PLANE('',#41988);
#1660=PLANE('',#41989);
#1661=PLANE('',#41990);
#1662=PLANE('',#41991);
#1663=PLANE('',#41992);
#1664=PLANE('',#41993);
#1665=PLANE('',#41994);
#1666=PLANE('',#41995);
#1667=PLANE('',#41996);
#1668=PLANE('',#41997);
#1669=PLANE('',#41998);
#1670=PLANE('',#41999);
#1671=PLANE('',#42000);
#1672=PLANE('',#42001);
#1673=PLANE('',#42002);
#1674=PLANE('',#42003);
#1675=PLANE('',#42004);
#1676=PLANE('',#42005);
#1677=PLANE('',#42006);
#1678=PLANE('',#42007);
#1679=PLANE('',#42008);
#1680=PLANE('',#42009);
#1681=PLANE('',#42010);
#1682=PLANE('',#42011);
#1683=PLANE('',#42012);
#1684=PLANE('',#42013);
#1685=PLANE('',#42014);
#1686=PLANE('',#42015);
#1687=PLANE('',#42016);
#1688=PLANE('',#42017);
#1689=PLANE('',#42018);
#1690=PLANE('',#42019);
#1691=PLANE('',#42020);
#1692=PLANE('',#42021);
#1693=PLANE('',#42022);
#1694=PLANE('',#42023);
#1695=PLANE('',#42024);
#1696=PLANE('',#42025);
#1697=PLANE('',#42026);
#1698=PLANE('',#42027);
#1699=PLANE('',#42028);
#1700=PLANE('',#42029);
#1701=PLANE('',#42030);
#1702=PLANE('',#42031);
#1703=PLANE('',#42032);
#1704=PLANE('',#42033);
#1705=PLANE('',#42034);
#1706=PLANE('',#42035);
#1707=PLANE('',#42036);
#1708=PLANE('',#42037);
#1709=PLANE('',#42038);
#1710=PLANE('',#42039);
#1711=PLANE('',#42040);
#1712=PLANE('',#42041);
#1713=PLANE('',#42042);
#1714=PLANE('',#42043);
#1715=PLANE('',#42044);
#1716=PLANE('',#42045);
#1717=PLANE('',#42046);
#1718=PLANE('',#42047);
#1719=PLANE('',#42048);
#1720=PLANE('',#42049);
#1721=PLANE('',#42050);
#1722=PLANE('',#42051);
#1723=PLANE('',#42052);
#1724=PLANE('',#42053);
#1725=PLANE('',#42054);
#1726=PLANE('',#42055);
#1727=PLANE('',#42056);
#1728=PLANE('',#42057);
#1729=PLANE('',#42058);
#1730=PLANE('',#42059);
#1731=PLANE('',#42060);
#1732=PLANE('',#42061);
#1733=PLANE('',#42062);
#1734=PLANE('',#42063);
#1735=PLANE('',#42064);
#1736=PLANE('',#42065);
#1737=PLANE('',#42066);
#1738=PLANE('',#42067);
#1739=PLANE('',#42068);
#1740=PLANE('',#42069);
#1741=PLANE('',#42070);
#1742=PLANE('',#42071);
#1743=PLANE('',#42072);
#1744=PLANE('',#42073);
#1745=PLANE('',#42074);
#1746=PLANE('',#42075);
#1747=PLANE('',#42076);
#1748=PLANE('',#42077);
#1749=PLANE('',#42078);
#1750=PLANE('',#42079);
#1751=PLANE('',#42080);
#1752=PLANE('',#42081);
#1753=PLANE('',#42082);
#1754=PLANE('',#42083);
#1755=PLANE('',#42084);
#1756=PLANE('',#42085);
#1757=PLANE('',#42086);
#1758=PLANE('',#42087);
#1759=PLANE('',#42088);
#1760=PLANE('',#42089);
#1761=PLANE('',#42090);
#1762=PLANE('',#42091);
#1763=PLANE('',#42092);
#1764=PLANE('',#42093);
#1765=PLANE('',#42094);
#1766=PLANE('',#42095);
#1767=PLANE('',#42096);
#1768=PLANE('',#42097);
#1769=PLANE('',#42098);
#1770=PLANE('',#42099);
#1771=PLANE('',#42100);
#1772=PLANE('',#42101);
#1773=PLANE('',#42102);
#1774=PLANE('',#42103);
#1775=PLANE('',#42104);
#1776=PLANE('',#42105);
#1777=PLANE('',#42106);
#1778=PLANE('',#42107);
#1779=PLANE('',#42108);
#1780=PLANE('',#42109);
#1781=PLANE('',#42110);
#1782=PLANE('',#42111);
#1783=PLANE('',#42112);
#1784=PLANE('',#42113);
#1785=PLANE('',#42114);
#1786=PLANE('',#42115);
#1787=PLANE('',#42116);
#1788=PLANE('',#42117);
#1789=PLANE('',#42118);
#1790=PLANE('',#42119);
#1791=PLANE('',#42120);
#1792=PLANE('',#42121);
#1793=PLANE('',#42122);
#1794=PLANE('',#42123);
#1795=PLANE('',#42124);
#1796=PLANE('',#42125);
#1797=PLANE('',#42126);
#1798=PLANE('',#42127);
#1799=PLANE('',#42128);
#1800=PLANE('',#42129);
#1801=PLANE('',#42130);
#1802=PLANE('',#42131);
#1803=PLANE('',#42132);
#1804=PLANE('',#42133);
#1805=PLANE('',#42134);
#1806=PLANE('',#42135);
#1807=PLANE('',#42136);
#1808=PLANE('',#42137);
#1809=PLANE('',#42138);
#1810=PLANE('',#42139);
#1811=PLANE('',#42140);
#1812=PLANE('',#42141);
#1813=PLANE('',#42142);
#1814=PLANE('',#42143);
#1815=PLANE('',#42144);
#1816=PLANE('',#42145);
#1817=PLANE('',#42146);
#1818=PLANE('',#42147);
#1819=PLANE('',#42148);
#1820=PLANE('',#42149);
#1821=PLANE('',#42150);
#1822=PLANE('',#42151);
#1823=PLANE('',#42152);
#1824=PLANE('',#42153);
#1825=PLANE('',#42154);
#1826=PLANE('',#42155);
#1827=PLANE('',#42156);
#1828=PLANE('',#42157);
#1829=PLANE('',#42158);
#1830=PLANE('',#42159);
#1831=PLANE('',#42160);
#1832=PLANE('',#42161);
#1833=PLANE('',#42162);
#1834=PLANE('',#42163);
#1835=PLANE('',#42164);
#1836=PLANE('',#42165);
#1837=PLANE('',#42166);
#1838=PLANE('',#42167);
#1839=PLANE('',#42168);
#1840=PLANE('',#42169);
#1841=PLANE('',#42170);
#1842=PLANE('',#42171);
#1843=PLANE('',#42172);
#1844=PLANE('',#42173);
#1845=PLANE('',#42174);
#1846=PLANE('',#42175);
#1847=PLANE('',#42176);
#1848=PLANE('',#42177);
#1849=PLANE('',#42178);
#1850=PLANE('',#42179);
#1851=PLANE('',#42180);
#1852=PLANE('',#42181);
#1853=PLANE('',#42182);
#1854=PLANE('',#42183);
#1855=PLANE('',#42184);
#1856=PLANE('',#42185);
#1857=PLANE('',#42186);
#1858=PLANE('',#42187);
#1859=PLANE('',#42188);
#1860=PLANE('',#42189);
#1861=PLANE('',#42190);
#1862=PLANE('',#42191);
#1863=PLANE('',#42192);
#1864=PLANE('',#42193);
#1865=PLANE('',#42194);
#1866=PLANE('',#42195);
#1867=PLANE('',#42196);
#1868=PLANE('',#42197);
#1869=PLANE('',#42198);
#1870=PLANE('',#42199);
#1871=PLANE('',#42200);
#1872=PLANE('',#42201);
#1873=PLANE('',#42202);
#1874=PLANE('',#42203);
#1875=PLANE('',#42204);
#1876=PLANE('',#42205);
#1877=PLANE('',#42206);
#1878=PLANE('',#42207);
#1879=PLANE('',#42208);
#1880=PLANE('',#42209);
#1881=PLANE('',#42210);
#1882=PLANE('',#42211);
#1883=PLANE('',#42212);
#1884=PLANE('',#42213);
#1885=PLANE('',#42214);
#1886=PLANE('',#42215);
#1887=PLANE('',#42216);
#1888=PLANE('',#42217);
#1889=PLANE('',#42218);
#1890=PLANE('',#42219);
#1891=PLANE('',#42220);
#1892=PLANE('',#42221);
#1893=PLANE('',#42222);
#1894=PLANE('',#42223);
#1895=PLANE('',#42224);
#1896=PLANE('',#42225);
#1897=PLANE('',#42226);
#1898=PLANE('',#42227);
#1899=PLANE('',#42228);
#1900=PLANE('',#42229);
#1901=PLANE('',#42230);
#1902=PLANE('',#42231);
#1903=PLANE('',#42232);
#1904=PLANE('',#42233);
#1905=PLANE('',#42234);
#1906=PLANE('',#42235);
#1907=PLANE('',#42236);
#1908=PLANE('',#42237);
#1909=PLANE('',#42238);
#1910=PLANE('',#42239);
#1911=PLANE('',#42240);
#1912=PLANE('',#42241);
#1913=PLANE('',#42242);
#1914=PLANE('',#42243);
#1915=PLANE('',#42244);
#1916=PLANE('',#42245);
#1917=PLANE('',#42246);
#1918=PLANE('',#42247);
#1919=PLANE('',#42248);
#1920=PLANE('',#42249);
#1921=PLANE('',#42250);
#1922=PLANE('',#42251);
#1923=PLANE('',#42252);
#1924=PLANE('',#42253);
#1925=PLANE('',#42254);
#1926=PLANE('',#42255);
#1927=PLANE('',#42256);
#1928=PLANE('',#42257);
#1929=PLANE('',#42258);
#1930=PLANE('',#42259);
#1931=PLANE('',#42260);
#1932=PLANE('',#42261);
#1933=PLANE('',#42262);
#1934=PLANE('',#42263);
#1935=PLANE('',#42264);
#1936=PLANE('',#42265);
#1937=PLANE('',#42266);
#1938=PLANE('',#42267);
#1939=PLANE('',#42268);
#1940=PLANE('',#42269);
#1941=PLANE('',#42270);
#1942=PLANE('',#42271);
#1943=PLANE('',#42272);
#1944=PLANE('',#42273);
#1945=PLANE('',#42274);
#1946=PLANE('',#42275);
#1947=PLANE('',#42276);
#1948=PLANE('',#42277);
#1949=PLANE('',#42278);
#1950=PLANE('',#42279);
#1951=PLANE('',#42280);
#1952=PLANE('',#42281);
#1953=PLANE('',#42282);
#1954=PLANE('',#42283);
#1955=PLANE('',#42284);
#1956=PLANE('',#42285);
#1957=PLANE('',#42286);
#1958=PLANE('',#42287);
#1959=PLANE('',#42288);
#1960=PLANE('',#42289);
#1961=PLANE('',#42290);
#1962=PLANE('',#42291);
#1963=PLANE('',#42292);
#1964=PLANE('',#42293);
#1965=PLANE('',#42294);
#1966=PLANE('',#42295);
#1967=PLANE('',#42296);
#1968=PLANE('',#42297);
#1969=PLANE('',#42298);
#1970=PLANE('',#42299);
#1971=PLANE('',#42300);
#1972=PLANE('',#42301);
#1973=PLANE('',#42302);
#1974=PLANE('',#42303);
#1975=PLANE('',#42304);
#1976=PLANE('',#42305);
#1977=PLANE('',#42306);
#1978=PLANE('',#42307);
#1979=PLANE('',#42308);
#1980=PLANE('',#42309);
#1981=PLANE('',#42310);
#1982=PLANE('',#42311);
#1983=PLANE('',#42312);
#1984=PLANE('',#42313);
#1985=PLANE('',#42314);
#1986=PLANE('',#42315);
#1987=PLANE('',#42316);
#1988=PLANE('',#42317);
#1989=PLANE('',#42318);
#1990=PLANE('',#42319);
#1991=PLANE('',#42320);
#1992=PLANE('',#42321);
#1993=PLANE('',#42322);
#1994=PLANE('',#42323);
#1995=PLANE('',#42324);
#1996=PLANE('',#42325);
#1997=PLANE('',#42326);
#1998=PLANE('',#42327);
#1999=PLANE('',#42328);
#2000=PLANE('',#42329);
#2001=PLANE('',#42330);
#2002=PLANE('',#42331);
#2003=PLANE('',#42332);
#2004=PLANE('',#42333);
#2005=PLANE('',#42334);
#2006=PLANE('',#42335);
#2007=PLANE('',#42336);
#2008=PLANE('',#42337);
#2009=PLANE('',#42338);
#2010=PLANE('',#42339);
#2011=PLANE('',#42340);
#2012=PLANE('',#42341);
#2013=PLANE('',#42342);
#2014=PLANE('',#42343);
#2015=PLANE('',#42344);
#2016=PLANE('',#42345);
#2017=PLANE('',#42346);
#2018=PLANE('',#42347);
#2019=PLANE('',#42348);
#2020=PLANE('',#42349);
#2021=PLANE('',#42350);
#2022=PLANE('',#42351);
#2023=PLANE('',#42352);
#2024=PLANE('',#42353);
#2025=PLANE('',#42354);
#2026=PLANE('',#42355);
#2027=PLANE('',#42356);
#2028=PLANE('',#42357);
#2029=PLANE('',#42358);
#2030=PLANE('',#42359);
#2031=PLANE('',#42360);
#2032=PLANE('',#42361);
#2033=PLANE('',#42362);
#2034=PLANE('',#42363);
#2035=PLANE('',#42364);
#2036=PLANE('',#42365);
#2037=PLANE('',#42366);
#2038=PLANE('',#42367);
#2039=PLANE('',#42368);
#2040=PLANE('',#42369);
#2041=PLANE('',#42370);
#2042=PLANE('',#42371);
#2043=PLANE('',#42372);
#2044=PLANE('',#42373);
#2045=PLANE('',#42374);
#2046=PLANE('',#42375);
#2047=PLANE('',#42376);
#2048=PLANE('',#42377);
#2049=PLANE('',#42378);
#2050=PLANE('',#42379);
#2051=PLANE('',#42380);
#2052=PLANE('',#42381);
#2053=PLANE('',#42382);
#2054=PLANE('',#42383);
#2055=PLANE('',#42384);
#2056=PLANE('',#42385);
#2057=PLANE('',#42386);
#2058=PLANE('',#42387);
#2059=PLANE('',#42388);
#2060=PLANE('',#42389);
#2061=PLANE('',#42390);
#2062=PLANE('',#42391);
#2063=PLANE('',#42392);
#2064=PLANE('',#42393);
#2065=PLANE('',#42394);
#2066=PLANE('',#42395);
#2067=PLANE('',#42396);
#2068=PLANE('',#42397);
#2069=PLANE('',#42398);
#2070=PLANE('',#42399);
#2071=PLANE('',#42400);
#2072=PLANE('',#42401);
#2073=PLANE('',#42402);
#2074=PLANE('',#42403);
#2075=PLANE('',#42404);
#2076=PLANE('',#42405);
#2077=PLANE('',#42406);
#2078=PLANE('',#42407);
#2079=PLANE('',#42408);
#2080=PLANE('',#42409);
#2081=PLANE('',#42410);
#2082=PLANE('',#42411);
#2083=PLANE('',#42412);
#2084=PLANE('',#42413);
#2085=PLANE('',#42414);
#2086=PLANE('',#42415);
#2087=PLANE('',#42416);
#2088=PLANE('',#42417);
#2089=PLANE('',#42418);
#2090=PLANE('',#42419);
#2091=PLANE('',#42420);
#2092=PLANE('',#42421);
#2093=PLANE('',#42422);
#2094=PLANE('',#42423);
#2095=PLANE('',#42424);
#2096=PLANE('',#42425);
#2097=PLANE('',#42426);
#2098=PLANE('',#42427);
#2099=PLANE('',#42428);
#2100=PLANE('',#42429);
#2101=PLANE('',#42430);
#2102=PLANE('',#42431);
#2103=PLANE('',#42432);
#2104=PLANE('',#42433);
#2105=PLANE('',#42434);
#2106=PLANE('',#42435);
#2107=PLANE('',#42436);
#2108=PLANE('',#42437);
#2109=PLANE('',#42438);
#2110=PLANE('',#42439);
#2111=PLANE('',#42440);
#2112=PLANE('',#42441);
#2113=PLANE('',#42442);
#2114=PLANE('',#42443);
#2115=PLANE('',#42444);
#2116=PLANE('',#42445);
#2117=PLANE('',#42446);
#2118=PLANE('',#42447);
#2119=PLANE('',#42448);
#2120=PLANE('',#42449);
#2121=PLANE('',#42450);
#2122=PLANE('',#42451);
#2123=PLANE('',#42452);
#2124=PLANE('',#42453);
#2125=PLANE('',#42454);
#2126=PLANE('',#42455);
#2127=PLANE('',#42456);
#2128=PLANE('',#42457);
#2129=PLANE('',#42458);
#2130=PLANE('',#42459);
#2131=PLANE('',#42460);
#2132=PLANE('',#42461);
#2133=PLANE('',#42462);
#2134=PLANE('',#42463);
#2135=PLANE('',#42464);
#2136=PLANE('',#42465);
#2137=PLANE('',#42466);
#2138=PLANE('',#42467);
#2139=PLANE('',#42468);
#2140=PLANE('',#42469);
#2141=PLANE('',#42470);
#2142=PLANE('',#42471);
#2143=PLANE('',#42472);
#2144=PLANE('',#42473);
#2145=PLANE('',#42474);
#2146=PLANE('',#42475);
#2147=PLANE('',#42476);
#2148=PLANE('',#42477);
#2149=PLANE('',#42478);
#2150=PLANE('',#42479);
#2151=PLANE('',#42480);
#2152=PLANE('',#42481);
#2153=PLANE('',#42482);
#2154=PLANE('',#42483);
#2155=PLANE('',#42484);
#2156=PLANE('',#42485);
#2157=PLANE('',#42486);
#2158=PLANE('',#42487);
#2159=PLANE('',#42488);
#2160=PLANE('',#42489);
#2161=PLANE('',#42490);
#2162=PLANE('',#42491);
#2163=PLANE('',#42492);
#2164=PLANE('',#42493);
#2165=PLANE('',#42494);
#2166=PLANE('',#42495);
#2167=PLANE('',#42496);
#2168=PLANE('',#42497);
#2169=PLANE('',#42498);
#2170=PLANE('',#42499);
#2171=PLANE('',#42500);
#2172=PLANE('',#42501);
#2173=PLANE('',#42502);
#2174=PLANE('',#42503);
#2175=PLANE('',#42504);
#2176=PLANE('',#42505);
#2177=PLANE('',#42506);
#2178=PLANE('',#42507);
#2179=PLANE('',#42508);
#2180=PLANE('',#42509);
#2181=TOROIDAL_SURFACE('',#40213,42.,0.5);
#2182=TOROIDAL_SURFACE('',#40217,44.4494897427832,1.2);
#2183=TOROIDAL_SURFACE('',#40221,42.,1.3);
#2184=TOROIDAL_SURFACE('',#40224,44.4494897427832,2.);
#2185=TOROIDAL_SURFACE('',#41139,3.2004,0.3556);
#2186=TOROIDAL_SURFACE('',#41146,3.2004,0.3556);
#2187=TOROIDAL_SURFACE('',#41148,3.2004,0.3556);
#2188=TOROIDAL_SURFACE('',#41154,3.2004,0.3556);
#2189=TOROIDAL_SURFACE('',#41308,59.5,0.5);
#2190=TOROIDAL_SURFACE('',#41312,61.9494897427832,1.2);
#2191=TOROIDAL_SURFACE('',#41316,59.5,1.3);
#2192=TOROIDAL_SURFACE('',#41319,61.9494897427832,2.);
#2193=B_SPLINE_CURVE_WITH_KNOTS('',3,(#53095,#53096,#53097,#53098,#53099,
#53100,#53101),.UNSPECIFIED.,.F.,.F.,(4,3,4),(0.,0.157051988846949,0.161817475839807),
 .UNSPECIFIED.);
#2194=B_SPLINE_CURVE_WITH_KNOTS('',3,(#53105,#53106,#53107,#53108,#53109,
#53110,#53111),.UNSPECIFIED.,.F.,.F.,(4,3,4),(-0.161817475844561,-0.157051988849942,
0.),.UNSPECIFIED.);
#2195=B_SPLINE_CURVE_WITH_KNOTS('',3,(#53125,#53126,#53127,#53128,#53129),
 .UNSPECIFIED.,.F.,.F.,(4,1,4),(0.,0.0312500000000001,0.0615627359467318),
 .UNSPECIFIED.);
#2196=B_SPLINE_CURVE_WITH_KNOTS('',3,(#53133,#53134,#53135,#53136,#53137),
 .UNSPECIFIED.,.F.,.F.,(4,1,4),(0.938437264048131,0.96875,1.),
 .UNSPECIFIED.);
#2197=B_SPLINE_CURVE_WITH_KNOTS('',3,(#53151,#53152,#53153,#53154,#53155),
 .UNSPECIFIED.,.F.,.F.,(4,1,4),(0.946686835703626,0.96875,1.),
 .UNSPECIFIED.);
#2198=B_SPLINE_CURVE_WITH_KNOTS('',3,(#53159,#53160,#53161,#53162,#53163),
 .UNSPECIFIED.,.F.,.F.,(4,1,4),(3.5013190022134E-10,0.0220631646607223,
0.0533131646607223),.UNSPECIFIED.);
#2199=B_SPLINE_CURVE_WITH_KNOTS('',3,(#53179,#53180,#53181,#53182,#53183,
#53184),.UNSPECIFIED.,.F.,.F.,(4,1,1,4),(0.,0.0312500000000001,0.0625000000000001,
0.0692715472300784),.UNSPECIFIED.);
#2200=B_SPLINE_CURVE_WITH_KNOTS('',3,(#53188,#53189,#53190,#53191,#53192,
#53193),.UNSPECIFIED.,.F.,.F.,(4,1,1,4),(0.930728452769685,0.9375,0.96875,
1.),.UNSPECIFIED.);
#2201=B_SPLINE_CURVE_WITH_KNOTS('',3,(#53209,#53210,#53211,#53212,#53213,
#53214),.UNSPECIFIED.,.F.,.F.,(4,1,1,4),(0.933751327236427,0.9375,0.96875,
1.),.UNSPECIFIED.);
#2202=B_SPLINE_CURVE_WITH_KNOTS('',3,(#53218,#53219,#53220,#53221,#53222,
#53223),.UNSPECIFIED.,.F.,.F.,(4,1,1,4),(0.,0.00374867276368319,0.0349986727636832,
0.0662486727636832),.UNSPECIFIED.);
#2203=B_SPLINE_CURVE_WITH_KNOTS('',3,(#53311,#53312,#53313,#53314,#53315,
#53316,#53317,#53318),.UNSPECIFIED.,.F.,.F.,(4,1,1,1,1,4),(-0.0709179217772133,
-0.0624999946725598,-0.0468738960837615,-0.0312499946726309,-0.0156244480037392,
3.22111226580546E-11),.UNSPECIFIED.);
#2204=B_SPLINE_CURVE_WITH_KNOTS('',3,(#53322,#53323,#53324,#53325,#53326,
#53327,#53328,#53329),.UNSPECIFIED.,.F.,.F.,(4,1,1,1,1,4),(-0.0709179217772133,
-0.0624999946725598,-0.0468738960837615,-0.0312499946726309,-0.0156244480037392,
3.22111226580546E-11),.UNSPECIFIED.);
#2205=B_SPLINE_CURVE_WITH_KNOTS('',3,(#54357,#54358,#54359,#54360,#54361,
#54362,#54363,#54364,#54365,#54366,#54367,#54368,#54369),.UNSPECIFIED.,
 .F.,.F.,(4,1,1,1,1,1,1,1,1,1,4),(0.762413302244216,0.765626103915763,0.781250005327804,
0.796876103916497,0.812500005327733,0.828126103916075,0.843750005327655,
0.859376103915845,0.875000005327586,0.890626103916147,0.904252904949607),
 .UNSPECIFIED.);
#2206=B_SPLINE_CURVE_WITH_KNOTS('',3,(#54373,#54374,#54375,#54376,#54377,
#54378,#54379,#54380,#54381,#54382,#54383,#54384,#54385),.UNSPECIFIED.,
 .F.,.F.,(4,1,1,1,1,1,1,1,1,1,4),(0.762413302244216,0.765626103915763,0.781250005327804,
0.796876103916497,0.812500005327733,0.828126103916075,0.843750005327655,
0.859376103915845,0.875000005327586,0.890626103916147,0.904252904949607),
 .UNSPECIFIED.);
#2207=B_SPLINE_CURVE_WITH_KNOTS('',3,(#54391,#54392,#54393,#54394,#54395),
 .UNSPECIFIED.,.F.,.F.,(4,1,4),(0.938437264053268,0.96875,1.),
 .UNSPECIFIED.);
#2208=B_SPLINE_CURVE_WITH_KNOTS('',3,(#54397,#54398,#54399,#54400,#54401,
#54402),.UNSPECIFIED.,.F.,.F.,(4,1,1,4),(0.,0.03125,0.0625,0.0662486727635731),
 .UNSPECIFIED.);
#2209=B_SPLINE_CURVE_WITH_KNOTS('',3,(#54409,#54410,#54411,#54412,#54413,
#54414,#54415),.UNSPECIFIED.,.F.,.F.,(4,3,4),(0.,0.00476894941081738,0.161935046139474),
 .UNSPECIFIED.);
#2210=B_SPLINE_CURVE_WITH_KNOTS('',3,(#54419,#54420,#54421,#54422,#54423),
 .UNSPECIFIED.,.F.,.F.,(4,1,4),(0.,0.0312500000000001,0.053313164296374),
 .UNSPECIFIED.);
#2211=B_SPLINE_CURVE_WITH_KNOTS('',3,(#54429,#54430,#54431,#54432,#54433,
#54434),.UNSPECIFIED.,.F.,.F.,(4,1,1,4),(0.801135800019621,0.8125,0.84375,
0.865533173173361),.UNSPECIFIED.);
#2212=B_SPLINE_CURVE_WITH_KNOTS('',3,(#54440,#54441,#54442,#54443,#54444,
#54445,#54446,#54447),.UNSPECIFIED.,.F.,.F.,(4,1,1,1,1,4),(0.780018892621858,
0.78125,0.8125,0.84375,0.875,0.886647915447513),.UNSPECIFIED.);
#2213=B_SPLINE_CURVE_WITH_KNOTS('',3,(#54452,#54453,#54454,#54455,#54456,
#54457),.UNSPECIFIED.,.F.,.F.,(4,1,1,4),(0.634466826826639,0.65625,0.6875,
0.698864199980379),.UNSPECIFIED.);
#2214=B_SPLINE_CURVE_WITH_KNOTS('',3,(#54465,#54466,#54467,#54468,#54469,
#54470,#54471,#54472),.UNSPECIFIED.,.F.,.F.,(4,1,1,1,1,4),(0.613352084552486,
0.625,0.65625,0.6875,0.71875,0.719981107378142),.UNSPECIFIED.);
#2215=B_SPLINE_CURVE_WITH_KNOTS('',3,(#54479,#54480,#54481,#54482,#54483,
#54484,#54485),.UNSPECIFIED.,.F.,.F.,(4,1,1,1,4),(0.467801769610686,0.46875,
0.5,0.53125,0.532198230389313),.UNSPECIFIED.);
#2216=B_SPLINE_CURVE_WITH_KNOTS('',3,(#54492,#54493,#54494,#54495,#54496,
#54497,#54498),.UNSPECIFIED.,.F.,.F.,(4,1,1,1,4),(0.446686835703626,0.46875,
0.5,0.53125,0.553313164296374),.UNSPECIFIED.);
#2217=B_SPLINE_CURVE_WITH_KNOTS('',3,(#54504,#54505,#54506,#54507,#54508,
#54509),.UNSPECIFIED.,.F.,.F.,(4,1,1,4),(0.301135800019622,0.3125,0.34375,
0.36553317317336),.UNSPECIFIED.);
#2218=B_SPLINE_CURVE_WITH_KNOTS('',3,(#54516,#54517,#54518,#54519,#54520,
#54521,#54522,#54523),.UNSPECIFIED.,.F.,.F.,(4,1,1,1,1,4),(0.280018892621858,
0.28125,0.3125,0.34375,0.375,0.386647915447513),.UNSPECIFIED.);
#2219=B_SPLINE_CURVE_WITH_KNOTS('',3,(#54530,#54531,#54532,#54533,#54534,
#54535),.UNSPECIFIED.,.F.,.F.,(4,1,1,4),(0.13446682682664,0.15625,0.1875,
0.198864199980378),.UNSPECIFIED.);
#2220=B_SPLINE_CURVE_WITH_KNOTS('',3,(#54540,#54541,#54542,#54543,#54544,
#54545,#54546,#54547),.UNSPECIFIED.,.F.,.F.,(4,1,1,1,1,4),(0.113352084552487,
0.125,0.15625,0.1875,0.21875,0.219981107378142),.UNSPECIFIED.);
#2221=B_SPLINE_CURVE_WITH_KNOTS('',3,(#54551,#54552,#54553,#54554,#54555,
#54556,#54557,#54558),.UNSPECIFIED.,.F.,.F.,(4,1,1,1,1,4),(0.771771373885868,
0.78125,0.8125,0.84375,0.875,0.894896231061431),.UNSPECIFIED.);
#2222=B_SPLINE_CURVE_WITH_KNOTS('',3,(#54562,#54563,#54564,#54565,#54566,
#54567,#54568,#54569),.UNSPECIFIED.,.F.,.F.,(4,1,1,1,1,4),(0.767085043602908,
0.78125,0.8125,0.84375,0.875,0.899580964190556),.UNSPECIFIED.);
#2223=B_SPLINE_CURVE_WITH_KNOTS('',3,(#54572,#54573,#54574,#54575,#54576,
#54577,#54578,#54579),.UNSPECIFIED.,.F.,.F.,(4,1,1,1,1,4),(0.605103768938569,
0.625,0.65625,0.6875,0.71875,0.728228626114132),.UNSPECIFIED.);
#2224=B_SPLINE_CURVE_WITH_KNOTS('',3,(#54584,#54585,#54586,#54587,#54588,
#54589,#54590,#54591),.UNSPECIFIED.,.F.,.F.,(4,1,1,1,1,4),(0.600419035809444,
0.625,0.65625,0.6875,0.71875,0.732914956397092),.UNSPECIFIED.);
#2225=B_SPLINE_CURVE_WITH_KNOTS('',3,(#54596,#54597,#54598,#54599,#54600,
#54601,#54602),.UNSPECIFIED.,.F.,.F.,(4,1,1,1,4),(0.438437264053268,0.46875,
0.5,0.53125,0.561562735946732),.UNSPECIFIED.);
#2226=B_SPLINE_CURVE_WITH_KNOTS('',3,(#54606,#54607,#54608,#54609,#54610,
#54611,#54612,#54613,#54614),.UNSPECIFIED.,.F.,.F.,(4,1,1,1,1,1,4),(0.433751327236426,
0.4375,0.46875,0.5,0.53125,0.5625,0.566248672763573),.UNSPECIFIED.);
#2227=B_SPLINE_CURVE_WITH_KNOTS('',3,(#54618,#54619,#54620,#54621,#54622,
#54623,#54624,#54625),.UNSPECIFIED.,.F.,.F.,(4,1,1,1,1,4),(0.271771373885868,
0.28125,0.3125,0.34375,0.375,0.394896231061431),.UNSPECIFIED.);
#2228=B_SPLINE_CURVE_WITH_KNOTS('',3,(#54629,#54630,#54631,#54632,#54633,
#54634,#54635,#54636),.UNSPECIFIED.,.F.,.F.,(4,1,1,1,1,4),(0.267085043602908,
0.28125,0.3125,0.34375,0.375,0.399580964190556),.UNSPECIFIED.);
#2229=B_SPLINE_CURVE_WITH_KNOTS('',3,(#54640,#54641,#54642,#54643,#54644,
#54645,#54646,#54647),.UNSPECIFIED.,.F.,.F.,(4,1,1,1,1,4),(0.105103768938569,
0.125,0.15625,0.1875,0.21875,0.228228626114132),.UNSPECIFIED.);
#2230=B_SPLINE_CURVE_WITH_KNOTS('',3,(#54650,#54651,#54652,#54653,#54654,
#54655,#54656,#54657),.UNSPECIFIED.,.F.,.F.,(4,1,1,1,1,4),(0.100419035809444,
0.125,0.15625,0.1875,0.21875,0.232914956397092),.UNSPECIFIED.);
#2231=B_SPLINE_CURVE_WITH_KNOTS('',3,(#54661,#54662,#54663,#54664,#54665,
#54666,#54667,#54668),.UNSPECIFIED.,.F.,.F.,(4,1,1,1,1,4),(0.764061321213706,
0.78125,0.8125,0.84375,0.875,0.902605614421776),.UNSPECIFIED.);
#2232=B_SPLINE_CURVE_WITH_KNOTS('',3,(#54672,#54673,#54674,#54675,#54676,
#54677,#54678,#54679),.UNSPECIFIED.,.F.,.F.,(4,1,1,1,1,4),(0.597394385578223,
0.625,0.65625,0.6875,0.71875,0.735938678786293),.UNSPECIFIED.);
#2233=B_SPLINE_CURVE_WITH_KNOTS('',3,(#54684,#54685,#54686,#54687,#54688,
#54689,#54690,#54691,#54692,#54693,#54694,#54695,#54696),.UNSPECIFIED.,
 .F.,.F.,(4,1,1,1,1,1,1,1,1,1,4),(0.595747106058032,0.609376103916341,0.625000005328168,
0.640626103916569,0.656250005328095,0.671876103916693,0.687500005328024,
0.703126103916646,0.718750005327949,0.734376103915816,0.737586706461852),
 .UNSPECIFIED.);
#2234=B_SPLINE_CURVE_WITH_KNOTS('',3,(#54701,#54702,#54703,#54704,#54705,
#54706,#54707,#54708,#54709),.UNSPECIFIED.,.F.,.F.,(4,1,1,1,1,1,4),(0.430728452769921,
0.4375,0.46875,0.5,0.53125,0.5625,0.569271547230078),.UNSPECIFIED.);
#2235=B_SPLINE_CURVE_WITH_KNOTS('',3,(#54713,#54714,#54715,#54716,#54717,
#54718,#54719,#54720,#54721,#54722,#54723,#54724,#54725),.UNSPECIFIED.,
 .F.,.F.,(4,1,1,1,1,1,1,1,1,1,4),(0.429082078647101,0.437500005328602,0.453126103916167,
0.468750005328528,0.484376103916409,0.500000005328459,0.515626103916853,
0.531250005328387,0.546876103916685,0.562500005328313,0.57091793098853),
 .UNSPECIFIED.);
#2236=B_SPLINE_CURVE_WITH_KNOTS('',3,(#54729,#54730,#54731,#54732,#54733,
#54734,#54735,#54736),.UNSPECIFIED.,.F.,.F.,(4,1,1,1,1,4),(0.264061321213707,
0.28125,0.3125,0.34375,0.375,0.402605614421775),.UNSPECIFIED.);
#2237=B_SPLINE_CURVE_WITH_KNOTS('',3,(#54740,#54741,#54742,#54743,#54744,
#54745,#54746,#54747,#54748,#54749,#54750,#54751,#54752),.UNSPECIFIED.,
 .F.,.F.,(4,1,1,1,1,1,1,1,1,1,4),(0.262413302245398,0.265626103917436,0.28125000532897,
0.296876103917406,0.312500005328897,0.328126103917406,0.343750005328825,
0.359376103917345,0.375000005328751,0.390626103917082,0.404252904915522),
 .UNSPECIFIED.);
#2238=B_SPLINE_CURVE_WITH_KNOTS('',3,(#54756,#54757,#54758,#54759,#54760,
#54761,#54762,#54763),.UNSPECIFIED.,.F.,.F.,(4,1,1,1,1,4),(0.097394385578224,
0.125,0.15625,0.1875,0.21875,0.235938678786293),.UNSPECIFIED.);
#2239=B_SPLINE_CURVE_WITH_KNOTS('',3,(#54766,#54767,#54768,#54769,#54770,
#54771,#54772,#54773,#54774,#54775,#54776,#54777,#54778),.UNSPECIFIED.,
 .F.,.F.,(4,1,1,1,1,1,1,1,1,1,4),(0.0957471060944922,0.109376103917698,
0.125000005329334,0.140626103917786,0.156250005329262,0.171876103917926,
0.18750000532919,0.203126103917764,0.218750005329116,0.234376103917514,
0.237586706463033),.UNSPECIFIED.);
#2240=B_SPLINE_CURVE_WITH_KNOTS('',3,(#54783,#54784,#54785,#54786,#54787,
#54788),.UNSPECIFIED.,.F.,.F.,(4,1,1,4),(0.930728452769921,0.9375,0.96875,
1.),.UNSPECIFIED.);
#2241=B_SPLINE_CURVE_WITH_KNOTS('',3,(#54790,#54791,#54792,#54793,#54794,
#54795,#54796,#54797),.UNSPECIFIED.,.F.,.F.,(4,1,1,1,1,4),(0.,0.0156255519209496,
0.0312500053295531,0.0468761039179887,0.0625000053294804,0.0709179305664047),
 .UNSPECIFIED.);
#2242=B_SPLINE_CURVE_WITH_KNOTS('',3,(#54814,#54815,#54816,#54817,#54818,
#54819,#54820,#54821),.UNSPECIFIED.,.F.,.F.,(4,1,1,1,1,4),(0.,0.0156255519209496,
0.0312500053295531,0.0468761039179887,0.0625000053294804,0.0709179305664047),
 .UNSPECIFIED.);
#2243=B_SPLINE_CURVE_WITH_KNOTS('',3,(#54853,#54854,#54855,#54856,#54857,
#54858,#54859,#54860,#54861,#54862,#54863,#54864,#54865),.UNSPECIFIED.,
 .F.,.F.,(4,1,1,1,1,1,1,1,1,1,4),(0.0957471060944922,0.109376103917698,
0.125000005329334,0.140626103917786,0.156250005329262,0.171876103917926,
0.18750000532919,0.203126103917764,0.218750005329116,0.234376103917514,
0.237586706463033),.UNSPECIFIED.);
#2244=B_SPLINE_CURVE_WITH_KNOTS('',3,(#54895,#54896,#54897,#54898,#54899,
#54900,#54901,#54902,#54903,#54904,#54905,#54906,#54907),.UNSPECIFIED.,
 .F.,.F.,(4,1,1,1,1,1,1,1,1,1,4),(0.262413302245398,0.265626103917436,0.28125000532897,
0.296876103917406,0.312500005328897,0.328126103917406,0.343750005328825,
0.359376103917345,0.375000005328751,0.390626103917082,0.404252904915522),
 .UNSPECIFIED.);
#2245=B_SPLINE_CURVE_WITH_KNOTS('',3,(#54936,#54937,#54938,#54939,#54940,
#54941,#54942,#54943,#54944,#54945,#54946,#54947,#54948),.UNSPECIFIED.,
 .F.,.F.,(4,1,1,1,1,1,1,1,1,1,4),(0.429082078647101,0.437500005328602,0.453126103916167,
0.468750005328528,0.484376103916409,0.500000005328459,0.515626103916853,
0.531250005328387,0.546876103916685,0.562500005328313,0.57091793098853),
 .UNSPECIFIED.);
#2246=B_SPLINE_CURVE_WITH_KNOTS('',3,(#55119,#55120,#55121,#55122,#55123,
#55124,#55125,#55126,#55127,#55128,#55129,#55130,#55131,#55132,#55133,#55134,
#55135,#55136,#55137,#55138),.UNSPECIFIED.,.F.,.F.,(4,2,2,2,2,2,2,2,2,4),
(0.,0.25,0.375,0.4375,0.46875,0.484375,0.4921875,0.5,0.75,1.),
 .UNSPECIFIED.);
#2247=B_SPLINE_CURVE_WITH_KNOTS('',3,(#55142,#55143,#55144,#55145,#55146,
#55147,#55148,#55149,#55150,#55151,#55152,#55153,#55154,#55155,#55156,#55157,
#55158,#55159,#55160,#55161,#55162,#55163,#55164,#55165,#55166,#55167,#55168,
#55169,#55170,#55171,#55172,#55173,#55174,#55175,#55176,#55177,#55178,#55179,
#55180,#55181,#55182,#55183,#55184),.UNSPECIFIED.,.F.,.F.,(4,3,3,3,3,3,
3,3,3,3,3,3,3,3,4),(0.,0.0927561114044612,0.190932288541826,0.249999999999901,
0.374999999999842,0.437499999999813,0.468749992147447,0.484374999999801,
0.492187499999797,0.499999999999798,0.749999999999899,0.83185850735952,
0.909993813469674,0.982561474349579,1.),.UNSPECIFIED.);
#2248=B_SPLINE_CURVE_WITH_KNOTS('',3,(#55228,#55229,#55230,#55231,#55232,
#55233,#55234,#55235,#55236,#55237,#55238,#55239,#55240,#55241,#55242,#55243,
#55244,#55245,#55246,#55247),.UNSPECIFIED.,.F.,.F.,(4,2,2,2,2,2,2,2,2,4),
(0.,0.25,0.375,0.4375,0.46875,0.484375,0.4921875,0.5,0.75,1.),
 .UNSPECIFIED.);
#2249=B_SPLINE_CURVE_WITH_KNOTS('',3,(#55248,#55249,#55250,#55251,#55252,
#55253,#55254,#55255,#55256,#55257,#55258,#55259,#55260,#55261,#55262,#55263,
#55264,#55265,#55266,#55267,#55268,#55269,#55270,#55271,#55272,#55273,#55274,
#55275,#55276,#55277,#55278,#55279,#55280,#55281,#55282,#55283,#55284,#55285,
#55286,#55287,#55288,#55289,#55290),.UNSPECIFIED.,.F.,.F.,(4,3,3,3,3,3,
3,3,3,3,3,3,3,3,4),(0.,0.0927561113839666,0.190932288501874,0.2499999999999,
0.374999999999847,0.437499999999822,0.468749992147457,0.48437499999981,
0.492187499999816,0.49999999999981,0.749999999999905,0.83185850736903,0.909993813488733,
0.982561474378202,1.),.UNSPECIFIED.);
#2250=B_SPLINE_CURVE_WITH_KNOTS('',3,(#55351,#55352,#55353,#55354,#55355,
#55356,#55357,#55358,#55359,#55360,#55361,#55362,#55363,#55364,#55365,#55366,
#55367,#55368,#55369,#55370),.UNSPECIFIED.,.F.,.F.,(4,2,2,2,2,2,2,2,2,4),
(0.,0.25,0.375,0.4375,0.46875,0.484375,0.4921875,0.5,0.75,1.),
 .UNSPECIFIED.);
#2251=B_SPLINE_CURVE_WITH_KNOTS('',3,(#55371,#55372,#55373,#55374,#55375,
#55376,#55377,#55378,#55379,#55380,#55381,#55382,#55383,#55384,#55385,#55386,
#55387,#55388,#55389,#55390,#55391,#55392,#55393,#55394,#55395,#55396,#55397,
#55398,#55399,#55400,#55401,#55402,#55403,#55404,#55405,#55406,#55407,#55408,
#55409,#55410,#55411,#55412,#55413),.UNSPECIFIED.,.F.,.F.,(4,3,3,3,3,3,
3,3,3,3,3,3,3,3,4),(0.,0.0927561113855575,0.190932288505144,0.250000000000093,
0.37500000000014,0.437500000000168,0.468749992147812,0.48437500000018,0.492187500000186,
0.500000000000184,0.750000000000092,0.831858507368402,0.909993813487336,
0.982561474376173,1.),.UNSPECIFIED.);
#2252=B_SPLINE_CURVE_WITH_KNOTS('',3,(#55454,#55455,#55456,#55457,#55458,
#55459,#55460,#55461,#55462,#55463,#55464,#55465,#55466,#55467,#55468,#55469,
#55470,#55471,#55472,#55473),.UNSPECIFIED.,.F.,.F.,(4,2,2,2,2,2,2,2,2,4),
(0.,0.25,0.375,0.4375,0.46875,0.484375,0.4921875,0.5,0.75,1.),
 .UNSPECIFIED.);
#2253=B_SPLINE_CURVE_WITH_KNOTS('',3,(#55477,#55478,#55479,#55480,#55481,
#55482,#55483,#55484,#55485,#55486,#55487,#55488,#55489,#55490,#55491,#55492,
#55493,#55494,#55495,#55496,#55497,#55498,#55499,#55500,#55501,#55502,#55503,
#55504,#55505,#55506,#55507,#55508,#55509,#55510,#55511,#55512,#55513,#55514,
#55515,#55516,#55517,#55518,#55519),.UNSPECIFIED.,.F.,.F.,(4,3,3,3,3,3,
3,3,3,3,3,3,3,3,4),(0.,0.092756111383829,0.190932288501491,0.249999999999982,
0.374999999999972,0.437499999999958,0.468749992147606,0.484374999999957,
0.492187499999956,0.499999999999956,0.749999999999978,0.831858507368429,
0.909993813487417,0.982561474376421,1.),.UNSPECIFIED.);
#2254=B_SPLINE_CURVE_WITH_KNOTS('',3,(#55882,#55883,#55884,#55885,#55886),
 .UNSPECIFIED.,.F.,.F.,(4,1,4),(0.,0.0312500000000001,0.0533131643109959),
 .UNSPECIFIED.);
#2255=B_SPLINE_CURVE_WITH_KNOTS('',3,(#55889,#55890,#55891,#55892,#55893,
#55894,#55895),.UNSPECIFIED.,.F.,.F.,(4,3,4),(-0.161935046144155,-0.00476894941103452,
0.),.UNSPECIFIED.);
#2256=B_SPLINE_CURVE_WITH_KNOTS('',3,(#55903,#55904,#55905,#55906,#55907,
#55908,#55909,#55910),.UNSPECIFIED.,.F.,.F.,(4,1,1,1,1,4),(0.,0.00123110737814575,
0.0324811073781457,0.0637311073781457,0.0949811073781457,0.106629022825536),
 .UNSPECIFIED.);
#2257=B_SPLINE_CURVE_WITH_KNOTS('',3,(#55915,#55916,#55917,#55918,#55919,
#55920),.UNSPECIFIED.,.F.,.F.,(4,1,1,4),(0.134466826826819,0.15625,0.1875,
0.198864199679252),.UNSPECIFIED.);
#2258=B_SPLINE_CURVE_WITH_KNOTS('',3,(#55928,#55929,#55930,#55931,#55932,
#55933,#55934,#55935),.UNSPECIFIED.,.F.,.F.,(4,1,1,1,1,4),(0.,0.0116479154473907,
0.0428979154473907,0.0741479154473907,0.105397915447391,0.106629022825536),
 .UNSPECIFIED.);
#2259=B_SPLINE_CURVE_WITH_KNOTS('',3,(#55942,#55943,#55944,#55945,#55946,
#55947),.UNSPECIFIED.,.F.,.F.,(4,1,1,4),(0.301135800390954,0.3125,0.34375,
0.365533173173181),.UNSPECIFIED.);
#2260=B_SPLINE_CURVE_WITH_KNOTS('',3,(#55952,#55953,#55954,#55955,#55956,
#55957,#55958),.UNSPECIFIED.,.F.,.F.,(4,1,1,1,4),(0.,0.0220631642961554,
0.0533131642961553,0.0845631642961553,0.10662632859231),.UNSPECIFIED.);
#2261=B_SPLINE_CURVE_WITH_KNOTS('',3,(#55966,#55967,#55968,#55969,#55970,
#55971,#55972),.UNSPECIFIED.,.F.,.F.,(4,1,1,1,4),(0.467801769610687,0.46875,
0.5,0.53125,0.532198230389314),.UNSPECIFIED.);
#2262=B_SPLINE_CURVE_WITH_KNOTS('',3,(#55977,#55978,#55979,#55980,#55981,
#55982,#55983,#55984),.UNSPECIFIED.,.F.,.F.,(4,1,1,1,1,4),(0.,0.00123110737814613,
0.0324811073781462,0.063731107378146,0.0949811073781461,0.106629022825536),
 .UNSPECIFIED.);
#2263=B_SPLINE_CURVE_WITH_KNOTS('',3,(#55992,#55993,#55994,#55995,#55996,
#55997),.UNSPECIFIED.,.F.,.F.,(4,1,1,4),(0.63446682682682,0.65625,0.6875,
0.698864199679252),.UNSPECIFIED.);
#2264=B_SPLINE_CURVE_WITH_KNOTS('',3,(#56002,#56003,#56004,#56005,#56006,
#56007,#56008,#56009),.UNSPECIFIED.,.F.,.F.,(4,1,1,1,1,4),(0.,0.0116479154473909,
0.0428979154473909,0.0741479154473906,0.105397915447391,0.106629022825536),
 .UNSPECIFIED.);
#2265=B_SPLINE_CURVE_WITH_KNOTS('',3,(#56015,#56016,#56017,#56018,#56019,
#56020),.UNSPECIFIED.,.F.,.F.,(4,1,1,4),(0.801135800390954,0.8125,0.84375,
0.86553317317318),.UNSPECIFIED.);
#2266=B_SPLINE_CURVE_WITH_KNOTS('',3,(#56026,#56027,#56028,#56029,#56030,
#56031),.UNSPECIFIED.,.F.,.F.,(4,1,1,4),(0.,0.03125,0.0625,0.0662486727636835),
 .UNSPECIFIED.);
#2267=B_SPLINE_CURVE_WITH_KNOTS('',3,(#56034,#56035,#56036,#56037,#56038),
 .UNSPECIFIED.,.F.,.F.,(4,1,4),(0.,0.03125,0.0615627359472197),
 .UNSPECIFIED.);
#2268=B_SPLINE_CURVE_WITH_KNOTS('',3,(#56043,#56044,#56045,#56046,#56047,
#56048,#56049,#56050),.UNSPECIFIED.,.F.,.F.,(4,1,1,1,1,4),(0.,0.0141649563968439,
0.0454149563968439,0.0766649563968438,0.107914956396844,0.132495920587091),
 .UNSPECIFIED.);
#2269=B_SPLINE_CURVE_WITH_KNOTS('',3,(#56053,#56054,#56055,#56056,#56057,
#56058,#56059,#56060),.UNSPECIFIED.,.F.,.F.,(4,1,1,1,1,4),(0.105103768938473,
0.125,0.15625,0.1875,0.21875,0.228228626114295),.UNSPECIFIED.);
#2270=B_SPLINE_CURVE_WITH_KNOTS('',3,(#56065,#56066,#56067,#56068,#56069,
#56070,#56071,#56072),.UNSPECIFIED.,.F.,.F.,(4,1,1,1,1,4),(0.,0.0245809641902474,
0.0558309641902474,0.0870809641902473,0.118330964190247,0.132495920587091),
 .UNSPECIFIED.);
#2271=B_SPLINE_CURVE_WITH_KNOTS('',3,(#56076,#56077,#56078,#56079,#56080,
#56081,#56082,#56083),.UNSPECIFIED.,.F.,.F.,(4,1,1,1,1,4),(0.271771373885705,
0.28125,0.3125,0.34375,0.375,0.394896231061528),.UNSPECIFIED.);
#2272=B_SPLINE_CURVE_WITH_KNOTS('',3,(#56086,#56087,#56088,#56089,#56090,
#56091,#56092,#56093,#56094),.UNSPECIFIED.,.F.,.F.,(4,1,1,1,1,1,4),(0.,
0.00374867276368307,0.034998672763683,0.0662486727636831,0.0974986727636831,
0.128748672763683,0.132497345527366),.UNSPECIFIED.);
#2273=B_SPLINE_CURVE_WITH_KNOTS('',3,(#56099,#56100,#56101,#56102,#56103,
#56104,#56105),.UNSPECIFIED.,.F.,.F.,(4,1,1,1,4),(0.43843726405327,0.46875,
0.5,0.53125,0.561562735946731),.UNSPECIFIED.);
#2274=B_SPLINE_CURVE_WITH_KNOTS('',3,(#56108,#56109,#56110,#56111,#56112,
#56113,#56114,#56115),.UNSPECIFIED.,.F.,.F.,(4,1,1,1,1,4),(0.,0.0141649563968442,
0.0454149563968442,0.0766649563968441,0.107914956396844,0.132495920587091),
 .UNSPECIFIED.);
#2275=B_SPLINE_CURVE_WITH_KNOTS('',3,(#56120,#56121,#56122,#56123,#56124,
#56125,#56126,#56127),.UNSPECIFIED.,.F.,.F.,(4,1,1,1,1,4),(0.605103768938473,
0.625,0.65625,0.6875,0.71875,0.728228626114296),.UNSPECIFIED.);
#2276=B_SPLINE_CURVE_WITH_KNOTS('',3,(#56130,#56131,#56132,#56133,#56134,
#56135,#56136,#56137),.UNSPECIFIED.,.F.,.F.,(4,1,1,1,1,4),(0.,0.0245809641902476,
0.0558309641902476,0.0870809641902475,0.118330964190247,0.132495920587092),
 .UNSPECIFIED.);
#2277=B_SPLINE_CURVE_WITH_KNOTS('',3,(#56141,#56142,#56143,#56144,#56145,
#56146,#56147,#56148),.UNSPECIFIED.,.F.,.F.,(4,1,1,1,1,4),(0.771771373885705,
0.78125,0.8125,0.84375,0.875,0.894896231061527),.UNSPECIFIED.);
#2278=B_SPLINE_CURVE_WITH_KNOTS('',3,(#56153,#56154,#56155,#56156,#56157,
#56158),.UNSPECIFIED.,.F.,.F.,(4,1,1,4),(0.,0.03125,0.0625,0.0692715472303151),
 .UNSPECIFIED.);
#2279=B_SPLINE_CURVE_WITH_KNOTS('',3,(#56163,#56164,#56165,#56166,#56167,
#56168,#56169,#56170),.UNSPECIFIED.,.F.,.F.,(4,1,1,1,1,4),(0.0973943855783285,
0.125,0.15625,0.1875,0.21875,0.235938678786541),.UNSPECIFIED.);
#2280=B_SPLINE_CURVE_WITH_KNOTS('',3,(#56175,#56176,#56177,#56178,#56179,
#56180,#56181,#56182,#56183,#56184,#56185,#56186,#56187),.UNSPECIFIED.,
 .F.,.F.,(4,1,1,1,1,1,1,1,1,1,4),(0.595747106058032,0.609376103916341,0.625000005328168,
0.640626103916569,0.656250005328095,0.671876103916693,0.687500005328024,
0.703126103916646,0.718750005327949,0.734376103915816,0.737586706461852),
 .UNSPECIFIED.);
#2281=B_SPLINE_CURVE_WITH_KNOTS('',3,(#56191,#56192,#56193,#56194,#56195,
#56196,#56197,#56198),.UNSPECIFIED.,.F.,.F.,(4,1,1,1,1,4),(0.26406132121346,
0.28125,0.3125,0.34375,0.375,0.402605614421673),.UNSPECIFIED.);
#2282=B_SPLINE_CURVE_WITH_KNOTS('',3,(#56204,#56205,#56206,#56207,#56208,
#56209,#56210,#56211,#56212),.UNSPECIFIED.,.F.,.F.,(4,1,1,1,1,1,4),(0.430728452769685,
0.4375,0.46875,0.5,0.53125,0.5625,0.569271547230316),.UNSPECIFIED.);
#2283=B_SPLINE_CURVE_WITH_KNOTS('',3,(#56218,#56219,#56220,#56221,#56222,
#56223,#56224,#56225),.UNSPECIFIED.,.F.,.F.,(4,1,1,1,1,4),(0.597394385578329,
0.625,0.65625,0.6875,0.71875,0.735938678786541),.UNSPECIFIED.);
#2284=B_SPLINE_CURVE_WITH_KNOTS('',3,(#56230,#56231,#56232,#56233,#56234,
#56235,#56236,#56237),.UNSPECIFIED.,.F.,.F.,(4,1,1,1,1,4),(0.76406132121346,
0.78125,0.8125,0.84375,0.875,0.902605614421672),.UNSPECIFIED.);
#2285=B_SPLINE_SURFACE_WITH_KNOTS('',3,1,((#53083,#53084),(#53085,#53086),
(#53087,#53088),(#53089,#53090),(#53091,#53092)),.UNSPECIFIED.,.F.,.F.,
 .F.,(4,1,4),(2,2),(0.967801769610354,0.96875,1.),(0.,0.0959999999999937),
 .UNSPECIFIED.);
#2286=B_SPLINE_SURFACE_WITH_KNOTS('',3,1,((#53113,#53114),(#53115,#53116),
(#53117,#53118),(#53119,#53120),(#53121,#53122)),.UNSPECIFIED.,.F.,.F.,
 .F.,(4,1,4),(2,2),(0.938437264048131,0.96875,1.),(0.,0.0959999999999979),
 .UNSPECIFIED.);
#2287=B_SPLINE_SURFACE_WITH_KNOTS('',3,1,((#53139,#53140),(#53141,#53142),
(#53143,#53144),(#53145,#53146),(#53147,#53148)),.UNSPECIFIED.,.F.,.F.,
 .F.,(4,1,4),(2,2),(0.,0.0220631646607223,0.0533131646607223),(0.,0.0960000000000576),
 .UNSPECIFIED.);
#2288=B_SPLINE_SURFACE_WITH_KNOTS('',3,1,((#53165,#53166),(#53167,#53168),
(#53169,#53170),(#53171,#53172),(#53173,#53174),(#53175,#53176)),
 .UNSPECIFIED.,.F.,.F.,.F.,(4,1,1,4),(2,2),(0.930728452769685,0.9375,0.96875,
1.),(0.,0.0960000000000171),.UNSPECIFIED.);
#2289=B_SPLINE_SURFACE_WITH_KNOTS('',3,1,((#53195,#53196),(#53197,#53198),
(#53199,#53200),(#53201,#53202),(#53203,#53204),(#53205,#53206)),
 .UNSPECIFIED.,.F.,.F.,.F.,(4,1,1,4),(2,2),(0.,0.00374867276368319,0.0349986727636832,
0.0662486727636832),(0.,0.0960000000000512),.UNSPECIFIED.);
#2290=B_SPLINE_SURFACE_WITH_KNOTS('',3,1,((#53293,#53294),(#53295,#53296),
(#53297,#53298),(#53299,#53300),(#53301,#53302),(#53303,#53304),(#53305,
#53306),(#53307,#53308)),.UNSPECIFIED.,.F.,.F.,.F.,(4,1,1,1,1,4),(2,2),
(-3.22111226580546E-11,0.0156244480037392,0.0312499946726309,0.0468738960837615,
0.0624999946725598,0.0709179217772133),(0.,0.0960000000000491),
 .UNSPECIFIED.);
#2291=B_SPLINE_SURFACE_WITH_KNOTS('',3,1,((#54329,#54330),(#54331,#54332),
(#54333,#54334),(#54335,#54336),(#54337,#54338),(#54339,#54340),(#54341,
#54342),(#54343,#54344),(#54345,#54346),(#54347,#54348),(#54349,#54350),
(#54351,#54352),(#54353,#54354)),.UNSPECIFIED.,.F.,.F.,.F.,(4,1,1,1,1,1,
1,1,1,1,4),(2,2),(0.0957470950504153,0.109373896083853,0.124999994672414,
0.140623896084155,0.156249994672345,0.171873896083925,0.187499994672267,
0.203123896083503,0.218749994672196,0.234373896084237,0.237586697755757),
(0.,0.0960000000000299),.UNSPECIFIED.);
#2292=B_SPLINE_SURFACE_WITH_KNOTS('',3,1,((#54798,#54799),(#54800,#54801),
(#54802,#54803),(#54804,#54805),(#54806,#54807),(#54808,#54809),(#54810,
#54811),(#54812,#54813)),.UNSPECIFIED.,.F.,.F.,.F.,(4,1,1,1,1,4),(2,2),
(0.929082069433556,0.93749999467052,0.953123896082011,0.968749994670447,
0.98437444807905,1.),(0.,0.0960000000000576),.UNSPECIFIED.);
#2293=B_SPLINE_SURFACE_WITH_KNOTS('',3,1,((#54826,#54827),(#54828,#54829),
(#54830,#54831),(#54832,#54833),(#54834,#54835),(#54836,#54837),(#54838,
#54839),(#54840,#54841),(#54842,#54843),(#54844,#54845),(#54846,#54847),
(#54848,#54849),(#54850,#54851)),.UNSPECIFIED.,.F.,.F.,.F.,(4,1,1,1,1,1,
1,1,1,1,4),(2,2),(0.762413293536994,0.765623896082486,0.781249994670884,
0.796873896082236,0.81249999467081,0.828123896082074,0.843749994670738,
0.859373896082214,0.874999994670666,0.890623896082302,0.904252893905486),
(0.,0.0960000000000257),.UNSPECIFIED.);
#2294=B_SPLINE_SURFACE_WITH_KNOTS('',3,1,((#54867,#54868),(#54869,#54870),
(#54871,#54872),(#54873,#54874),(#54875,#54876),(#54877,#54878),(#54879,
#54880),(#54881,#54882),(#54883,#54884),(#54885,#54886),(#54887,#54888),
(#54889,#54890),(#54891,#54892)),.UNSPECIFIED.,.F.,.F.,.F.,(4,1,1,1,1,1,
1,1,1,1,4),(2,2),(0.595747095084501,0.609373896082918,0.624999994671249,
0.640623896082655,0.656249994671175,0.671873896082594,0.687499994671103,
0.703123896082594,0.71874999467103,0.734373896082564,0.737586697754574),
(0.,0.0960000000000214),.UNSPECIFIED.);
#2295=B_SPLINE_SURFACE_WITH_KNOTS('',3,1,((#54908,#54909),(#54910,#54911),
(#54912,#54913),(#54914,#54915),(#54916,#54917),(#54918,#54919),(#54920,
#54921),(#54922,#54923),(#54924,#54925),(#54926,#54927),(#54928,#54929),
(#54930,#54931),(#54932,#54933)),.UNSPECIFIED.,.F.,.F.,.F.,(4,1,1,1,1,1,
1,1,1,1,4),(2,2),(0.429082069011431,0.437499994671687,0.453123896083315,
0.468749994671613,0.484373896083147,0.499999994671541,0.515623896083591,
0.531249994671472,0.546873896083833,0.562499994671398,0.570917921352938),
(0.,0.0960000000000299),.UNSPECIFIED.);
#2296=B_SPLINE_SURFACE_WITH_KNOTS('',1,3,((#55079,#55080,#55081,#55082,
#55083,#55084,#55085,#55086,#55087,#55088,#55089,#55090,#55091,#55092,#55093,
#55094,#55095,#55096,#55097,#55098),(#55099,#55100,#55101,#55102,#55103,
#55104,#55105,#55106,#55107,#55108,#55109,#55110,#55111,#55112,#55113,#55114,
#55115,#55116,#55117,#55118)),.UNSPECIFIED.,.F.,.F.,.F.,(2,2),(4,2,2,2,
2,2,2,2,2,4),(0.,1.),(0.,0.25,0.375,0.4375,0.46875,0.484375,0.4921875,0.5,
0.75,1.),.UNSPECIFIED.);
#2297=B_SPLINE_SURFACE_WITH_KNOTS('',1,3,((#55185,#55186,#55187,#55188,
#55189,#55190,#55191,#55192,#55193,#55194,#55195,#55196,#55197,#55198,#55199,
#55200,#55201,#55202,#55203,#55204),(#55205,#55206,#55207,#55208,#55209,
#55210,#55211,#55212,#55213,#55214,#55215,#55216,#55217,#55218,#55219,#55220,
#55221,#55222,#55223,#55224)),.UNSPECIFIED.,.F.,.F.,.F.,(2,2),(4,2,2,2,
2,2,2,2,2,4),(0.,1.),(0.,0.25,0.375,0.4375,0.46875,0.484375,0.4921875,0.5,
0.75,1.),.UNSPECIFIED.);
#2298=B_SPLINE_SURFACE_WITH_KNOTS('',1,3,((#55308,#55309,#55310,#55311,
#55312,#55313,#55314,#55315,#55316,#55317,#55318,#55319,#55320,#55321,#55322,
#55323,#55324,#55325,#55326,#55327),(#55328,#55329,#55330,#55331,#55332,
#55333,#55334,#55335,#55336,#55337,#55338,#55339,#55340,#55341,#55342,#55343,
#55344,#55345,#55346,#55347)),.UNSPECIFIED.,.F.,.F.,.F.,(2,2),(4,2,2,2,
2,2,2,2,2,4),(0.,1.),(0.,0.25,0.375,0.4375,0.46875,0.484375,0.4921875,0.5,
0.75,1.),.UNSPECIFIED.);
#2299=B_SPLINE_SURFACE_WITH_KNOTS('',1,3,((#55414,#55415,#55416,#55417,
#55418,#55419,#55420,#55421,#55422,#55423,#55424,#55425,#55426,#55427,#55428,
#55429,#55430,#55431,#55432,#55433),(#55434,#55435,#55436,#55437,#55438,
#55439,#55440,#55441,#55442,#55443,#55444,#55445,#55446,#55447,#55448,#55449,
#55450,#55451,#55452,#55453)),.UNSPECIFIED.,.F.,.F.,.F.,(2,2),(4,2,2,2,
2,2,2,2,2,4),(0.,1.),(0.,0.25,0.375,0.4375,0.46875,0.484375,0.4921875,0.5,
0.75,1.),.UNSPECIFIED.);
#2300=B_SPLINE_SURFACE_WITH_KNOTS('',3,1,((#56240,#56241),(#56242,#56243),
(#56244,#56245),(#56246,#56247),(#56248,#56249),(#56250,#56251),(#56252,
#56253),(#56254,#56255),(#56256,#56257),(#56258,#56259),(#56260,#56261),
(#56262,#56263),(#56264,#56265)),.UNSPECIFIED.,.F.,.F.,.F.,(4,1,1,1,1,1,
1,1,1,1,4),(2,2),(0.262413293538176,0.265623896084184,0.281249994672051,
0.296873896083354,0.312499994671976,0.328123896083308,0.343749994671905,
0.359373896083431,0.374999994671832,0.390623896083659,0.404252893941946),
(0.,0.0960000000000214),.UNSPECIFIED.);
#2301=B_SPLINE_SURFACE_WITH_KNOTS('',3,1,((#56296,#56297),(#56298,#56299),
(#56300,#56301),(#56302,#56303),(#56304,#56305),(#56306,#56307),(#56308,
#56309),(#56310,#56311)),.UNSPECIFIED.,.F.,.F.,.F.,(4,1,1,1,1,4),(2,2),
(0.,0.0245809641902474,0.0558309641902474,0.0870809641902473,0.118330964190247,
0.132495920587091),(0.,0.096000000000015),.UNSPECIFIED.);
#2302=B_SPLINE_SURFACE_WITH_KNOTS('',3,1,((#56314,#56315),(#56316,#56317),
(#56318,#56319),(#56320,#56321),(#56322,#56323),(#56324,#56325),(#56326,
#56327),(#56328,#56329)),.UNSPECIFIED.,.F.,.F.,.F.,(4,1,1,1,1,4),(2,2),
(0.26406132121346,0.28125,0.3125,0.34375,0.375,0.402605614421673),(0.,0.0960000000000342),
 .UNSPECIFIED.);
#2303=B_SPLINE_SURFACE_WITH_KNOTS('',3,1,((#56331,#56332),(#56333,#56334),
(#56335,#56336),(#56337,#56338),(#56339,#56340),(#56341,#56342),(#56343,
#56344),(#56345,#56346)),.UNSPECIFIED.,.F.,.F.,.F.,(4,1,1,1,1,4),(2,2),
(0.,0.0141649563968439,0.0454149563968439,0.0766649563968438,0.107914956396844,
0.132495920587091),(0.,0.0959999999999916),.UNSPECIFIED.);
#2304=B_SPLINE_SURFACE_WITH_KNOTS('',3,1,((#56349,#56350),(#56351,#56352),
(#56353,#56354),(#56355,#56356),(#56357,#56358),(#56359,#56360),(#56361,
#56362),(#56363,#56364)),.UNSPECIFIED.,.F.,.F.,.F.,(4,1,1,1,1,4),(2,2),
(0.0973943855783285,0.125,0.15625,0.1875,0.21875,0.235938678786541),(0.,
0.0960000000000321),.UNSPECIFIED.);
#2305=B_SPLINE_SURFACE_WITH_KNOTS('',3,1,((#56366,#56367),(#56368,#56369),
(#56370,#56371),(#56372,#56373),(#56374,#56375),(#56376,#56377)),
 .UNSPECIFIED.,.F.,.F.,.F.,(4,1,1,4),(2,2),(0.,0.03125,0.0625,0.0662486727636835),
(0.,0.0960000000000193),.UNSPECIFIED.);
#2306=B_SPLINE_SURFACE_WITH_KNOTS('',3,1,((#56378,#56379),(#56380,#56381),
(#56382,#56383),(#56384,#56385),(#56386,#56387),(#56388,#56389)),
 .UNSPECIFIED.,.F.,.F.,.F.,(4,1,1,4),(2,2),(0.,0.03125,0.0625,0.0692715472303151),
(0.,0.0960000000000278),.UNSPECIFIED.);
#2307=B_SPLINE_SURFACE_WITH_KNOTS('',3,1,((#56391,#56392),(#56393,#56394),
(#56395,#56396),(#56397,#56398),(#56399,#56400),(#56401,#56402),(#56403,
#56404),(#56405,#56406)),.UNSPECIFIED.,.F.,.F.,.F.,(4,1,1,1,1,4),(2,2),
(0.,0.0245809641902476,0.0558309641902476,0.0870809641902475,0.118330964190247,
0.132495920587092),(0.,0.0959999999999617),.UNSPECIFIED.);
#2308=B_SPLINE_SURFACE_WITH_KNOTS('',3,1,((#56408,#56409),(#56410,#56411),
(#56412,#56413),(#56414,#56415),(#56416,#56417),(#56418,#56419),(#56420,
#56421),(#56422,#56423)),.UNSPECIFIED.,.F.,.F.,.F.,(4,1,1,1,1,4),(2,2),
(0.76406132121346,0.78125,0.8125,0.84375,0.875,0.902605614421672),(0.,0.0960000000000022),
 .UNSPECIFIED.);
#2309=B_SPLINE_SURFACE_WITH_KNOTS('',3,1,((#56426,#56427),(#56428,#56429),
(#56430,#56431),(#56432,#56433),(#56434,#56435),(#56436,#56437),(#56438,
#56439),(#56440,#56441)),.UNSPECIFIED.,.F.,.F.,.F.,(4,1,1,1,1,4),(2,2),
(0.,0.0141649563968442,0.0454149563968442,0.0766649563968441,0.107914956396844,
0.132495920587091),(0.,0.0959999999999745),.UNSPECIFIED.);
#2310=B_SPLINE_SURFACE_WITH_KNOTS('',3,1,((#56443,#56444),(#56445,#56446),
(#56447,#56448),(#56449,#56450),(#56451,#56452),(#56453,#56454),(#56455,
#56456),(#56457,#56458)),.UNSPECIFIED.,.F.,.F.,.F.,(4,1,1,1,1,4),(2,2),
(0.597394385578329,0.625,0.65625,0.6875,0.71875,0.735938678786541),(0.,
0.0960000000000129),.UNSPECIFIED.);
#2311=B_SPLINE_SURFACE_WITH_KNOTS('',3,1,((#56461,#56462),(#56463,#56464),
(#56465,#56466),(#56467,#56468),(#56469,#56470),(#56471,#56472),(#56473,
#56474),(#56475,#56476),(#56477,#56478)),.UNSPECIFIED.,.F.,.F.,.F.,(4,1,
1,1,1,1,4),(2,2),(0.430728452769685,0.4375,0.46875,0.5,0.53125,0.5625,0.569271547230316),
(0.,0.0959999999999958),.UNSPECIFIED.);
#2312=B_SPLINE_SURFACE_WITH_KNOTS('',3,1,((#56481,#56482),(#56483,#56484),
(#56485,#56486),(#56487,#56488),(#56489,#56490),(#56491,#56492),(#56493,
#56494),(#56495,#56496),(#56497,#56498)),.UNSPECIFIED.,.F.,.F.,.F.,(4,1,
1,1,1,1,4),(2,2),(0.,0.00374867276368307,0.034998672763683,0.0662486727636831,
0.0974986727636831,0.128748672763683,0.132497345527366),(0.,0.0959999999999873),
 .UNSPECIFIED.);
#2313=B_SPLINE_SURFACE_WITH_KNOTS('',3,1,((#56500,#56501),(#56502,#56503),
(#56504,#56505),(#56506,#56507),(#56508,#56509),(#56510,#56511),(#56512,
#56513),(#56514,#56515)),.UNSPECIFIED.,.F.,.F.,.F.,(4,1,1,1,1,4),(2,2),
(0.,0.0116479154473907,0.0428979154473907,0.0741479154473907,0.105397915447391,
0.106629022825536),(0.,0.0960000000000235),.UNSPECIFIED.);
#2314=B_SPLINE_SURFACE_WITH_KNOTS('',3,1,((#56518,#56519),(#56520,#56521),
(#56522,#56523),(#56524,#56525),(#56526,#56527),(#56528,#56529),(#56530,
#56531),(#56532,#56533)),.UNSPECIFIED.,.F.,.F.,.F.,(4,1,1,1,1,4),(2,2),
(0.271771373885705,0.28125,0.3125,0.34375,0.375,0.394896231061528),(0.,
0.0959999999999894),.UNSPECIFIED.);
#2315=B_SPLINE_SURFACE_WITH_KNOTS('',3,1,((#56535,#56536),(#56537,#56538),
(#56539,#56540),(#56541,#56542),(#56543,#56544),(#56545,#56546),(#56547,
#56548),(#56549,#56550)),.UNSPECIFIED.,.F.,.F.,.F.,(4,1,1,1,1,4),(2,2),
(0.,0.00123110737814575,0.0324811073781457,0.0637311073781457,0.0949811073781457,
0.106629022825536),(0.,0.0960000000000043),.UNSPECIFIED.);
#2316=B_SPLINE_SURFACE_WITH_KNOTS('',3,1,((#56553,#56554),(#56555,#56556),
(#56557,#56558),(#56559,#56560),(#56561,#56562),(#56563,#56564),(#56565,
#56566),(#56567,#56568)),.UNSPECIFIED.,.F.,.F.,.F.,(4,1,1,1,1,4),(2,2),
(0.105103768938473,0.125,0.15625,0.1875,0.21875,0.228228626114295),(0.,
0.0959999999999894),.UNSPECIFIED.);
#2317=B_SPLINE_SURFACE_WITH_KNOTS('',3,1,((#56570,#56571),(#56572,#56573),
(#56574,#56575),(#56576,#56577),(#56578,#56579)),.UNSPECIFIED.,.F.,.F.,
 .F.,(4,1,4),(2,2),(0.,0.0312500000000001,0.0533131646711191),(0.,0.0960000000000768),
 .UNSPECIFIED.);
#2318=B_SPLINE_SURFACE_WITH_KNOTS('',3,1,((#56580,#56581),(#56582,#56583),
(#56584,#56585),(#56586,#56587),(#56588,#56589)),.UNSPECIFIED.,.F.,.F.,
 .F.,(4,1,4),(2,2),(0.,0.03125,0.0615627359472197),(0.,0.0960000000000001),
 .UNSPECIFIED.);
#2319=B_SPLINE_SURFACE_WITH_KNOTS('',3,1,((#56591,#56592),(#56593,#56594),
(#56595,#56596),(#56597,#56598),(#56599,#56600),(#56601,#56602),(#56603,
#56604),(#56605,#56606)),.UNSPECIFIED.,.F.,.F.,.F.,(4,1,1,1,1,4),(2,2),
(0.,0.0116479154473909,0.0428979154473909,0.0741479154473906,0.105397915447391,
0.106629022825536),(0.,0.0960000000000491),.UNSPECIFIED.);
#2320=B_SPLINE_SURFACE_WITH_KNOTS('',3,1,((#56608,#56609),(#56610,#56611),
(#56612,#56613),(#56614,#56615),(#56616,#56617),(#56618,#56619),(#56620,
#56621),(#56622,#56623)),.UNSPECIFIED.,.F.,.F.,.F.,(4,1,1,1,1,4),(2,2),
(0.771771373885705,0.78125,0.8125,0.84375,0.875,0.894896231061527),(0.,
0.0960000000000001),.UNSPECIFIED.);
#2321=B_SPLINE_SURFACE_WITH_KNOTS('',3,1,((#56626,#56627),(#56628,#56629),
(#56630,#56631),(#56632,#56633),(#56634,#56635),(#56636,#56637),(#56638,
#56639),(#56640,#56641)),.UNSPECIFIED.,.F.,.F.,.F.,(4,1,1,1,1,4),(2,2),
(0.,0.00123110737814613,0.0324811073781462,0.063731107378146,0.0949811073781461,
0.106629022825536),(0.,0.0960000000000043),.UNSPECIFIED.);
#2322=B_SPLINE_SURFACE_WITH_KNOTS('',3,1,((#56643,#56644),(#56645,#56646),
(#56647,#56648),(#56649,#56650),(#56651,#56652),(#56653,#56654),(#56655,
#56656),(#56657,#56658)),.UNSPECIFIED.,.F.,.F.,.F.,(4,1,1,1,1,4),(2,2),
(0.605103768938473,0.625,0.65625,0.6875,0.71875,0.728228626114296),(0.,
0.0959999999999873),.UNSPECIFIED.);
#2323=B_SPLINE_SURFACE_WITH_KNOTS('',3,1,((#56661,#56662),(#56663,#56664),
(#56665,#56666),(#56667,#56668),(#56669,#56670),(#56671,#56672),(#56673,
#56674)),.UNSPECIFIED.,.F.,.F.,.F.,(4,1,1,1,4),(2,2),(0.43843726405327,
0.46875,0.5,0.53125,0.561562735946731),(0.,0.0960000000000065),
 .UNSPECIFIED.);
#2324=B_SPLINE_SURFACE_WITH_KNOTS('',3,1,((#56677,#56678),(#56679,#56680),
(#56681,#56682),(#56683,#56684),(#56685,#56686),(#56687,#56688),(#56689,
#56690)),.UNSPECIFIED.,.F.,.F.,.F.,(4,1,1,1,4),(2,2),(0.,0.0220631642961554,
0.0533131642961553,0.0845631642961553,0.10662632859231),(0.,0.0960000000000299),
 .UNSPECIFIED.);
#2325=B_SPLINE_SURFACE_WITH_KNOTS('',3,1,((#56692,#56693),(#56694,#56695),
(#56696,#56697),(#56698,#56699),(#56700,#56701),(#56702,#56703)),
 .UNSPECIFIED.,.F.,.F.,.F.,(4,1,1,4),(2,2),(0.301135800019707,0.3125,0.34375,
0.365533173173181),(0.,0.0959999999999553),.UNSPECIFIED.);
#2326=B_SPLINE_SURFACE_WITH_KNOTS('',3,1,((#56705,#56706),(#56707,#56708),
(#56709,#56710),(#56711,#56712),(#56713,#56714),(#56715,#56716)),
 .UNSPECIFIED.,.F.,.F.,.F.,(4,1,1,4),(2,2),(0.134466826826819,0.15625,0.1875,
0.198864199980294),(0.,0.0959999999999489),.UNSPECIFIED.);
#2327=B_SPLINE_SURFACE_WITH_KNOTS('',3,1,((#56718,#56719),(#56720,#56721),
(#56722,#56723),(#56724,#56725),(#56726,#56727)),.UNSPECIFIED.,.F.,.F.,
 .F.,(4,1,4),(2,2),(0.,0.03125,0.0321982303893307),(0.,0.0959999999999532),
 .UNSPECIFIED.);
#2328=B_SPLINE_SURFACE_WITH_KNOTS('',3,1,((#56729,#56730),(#56731,#56732),
(#56733,#56734),(#56735,#56736),(#56737,#56738),(#56739,#56740)),
 .UNSPECIFIED.,.F.,.F.,.F.,(4,1,1,4),(2,2),(0.801135800019707,0.8125,0.84375,
0.86553317317318),(0.,0.0959999999999511),.UNSPECIFIED.);
#2329=B_SPLINE_SURFACE_WITH_KNOTS('',3,1,((#56743,#56744),(#56745,#56746),
(#56747,#56748),(#56749,#56750),(#56751,#56752),(#56753,#56754)),
 .UNSPECIFIED.,.F.,.F.,.F.,(4,1,1,4),(2,2),(0.63446682682682,0.65625,0.6875,
0.698864199980293),(0.,0.0959999999999106),.UNSPECIFIED.);
#2330=B_SPLINE_SURFACE_WITH_KNOTS('',3,1,((#56757,#56758),(#56759,#56760),
(#56761,#56762),(#56763,#56764),(#56765,#56766),(#56767,#56768),(#56769,
#56770)),.UNSPECIFIED.,.F.,.F.,.F.,(4,1,1,1,4),(2,2),(0.467801769610687,
0.46875,0.5,0.53125,0.532198230389314),(0.,0.0959999999999468),
 .UNSPECIFIED.);
#2331=FACE_OUTER_BOUND('',#4245,.T.);
#2332=FACE_OUTER_BOUND('',#4246,.T.);
#2333=FACE_OUTER_BOUND('',#4247,.T.);
#2334=FACE_OUTER_BOUND('',#4248,.T.);
#2335=FACE_OUTER_BOUND('',#4249,.T.);
#2336=FACE_OUTER_BOUND('',#4250,.T.);
#2337=FACE_OUTER_BOUND('',#4251,.T.);
#2338=FACE_OUTER_BOUND('',#4252,.T.);
#2339=FACE_OUTER_BOUND('',#4253,.T.);
#2340=FACE_OUTER_BOUND('',#4254,.T.);
#2341=FACE_OUTER_BOUND('',#4255,.T.);
#2342=FACE_OUTER_BOUND('',#4256,.T.);
#2343=FACE_OUTER_BOUND('',#4257,.T.);
#2344=FACE_OUTER_BOUND('',#4258,.T.);
#2345=FACE_OUTER_BOUND('',#4259,.T.);
#2346=FACE_OUTER_BOUND('',#4260,.T.);
#2347=FACE_OUTER_BOUND('',#4261,.T.);
#2348=FACE_OUTER_BOUND('',#4262,.T.);
#2349=FACE_OUTER_BOUND('',#4263,.T.);
#2350=FACE_OUTER_BOUND('',#4264,.T.);
#2351=FACE_OUTER_BOUND('',#4265,.T.);
#2352=FACE_OUTER_BOUND('',#4266,.T.);
#2353=FACE_OUTER_BOUND('',#4267,.T.);
#2354=FACE_OUTER_BOUND('',#4268,.T.);
#2355=FACE_OUTER_BOUND('',#4269,.T.);
#2356=FACE_OUTER_BOUND('',#4270,.T.);
#2357=FACE_OUTER_BOUND('',#4271,.T.);
#2358=FACE_OUTER_BOUND('',#4272,.T.);
#2359=FACE_OUTER_BOUND('',#4273,.T.);
#2360=FACE_OUTER_BOUND('',#4274,.T.);
#2361=FACE_OUTER_BOUND('',#4275,.T.);
#2362=FACE_OUTER_BOUND('',#4276,.T.);
#2363=FACE_OUTER_BOUND('',#4277,.T.);
#2364=FACE_OUTER_BOUND('',#4278,.T.);
#2365=FACE_OUTER_BOUND('',#4279,.T.);
#2366=FACE_OUTER_BOUND('',#4280,.T.);
#2367=FACE_OUTER_BOUND('',#4281,.T.);
#2368=FACE_OUTER_BOUND('',#4282,.T.);
#2369=FACE_OUTER_BOUND('',#4283,.T.);
#2370=FACE_OUTER_BOUND('',#4284,.T.);
#2371=FACE_OUTER_BOUND('',#4285,.T.);
#2372=FACE_OUTER_BOUND('',#4286,.T.);
#2373=FACE_OUTER_BOUND('',#4287,.T.);
#2374=FACE_OUTER_BOUND('',#4288,.T.);
#2375=FACE_OUTER_BOUND('',#4289,.T.);
#2376=FACE_OUTER_BOUND('',#4290,.T.);
#2377=FACE_OUTER_BOUND('',#4291,.T.);
#2378=FACE_OUTER_BOUND('',#4292,.T.);
#2379=FACE_OUTER_BOUND('',#4293,.T.);
#2380=FACE_OUTER_BOUND('',#4294,.T.);
#2381=FACE_OUTER_BOUND('',#4295,.T.);
#2382=FACE_OUTER_BOUND('',#4296,.T.);
#2383=FACE_OUTER_BOUND('',#4297,.T.);
#2384=FACE_OUTER_BOUND('',#4298,.T.);
#2385=FACE_OUTER_BOUND('',#4299,.T.);
#2386=FACE_OUTER_BOUND('',#4300,.T.);
#2387=FACE_OUTER_BOUND('',#4301,.T.);
#2388=FACE_OUTER_BOUND('',#4302,.T.);
#2389=FACE_OUTER_BOUND('',#4303,.T.);
#2390=FACE_OUTER_BOUND('',#4304,.T.);
#2391=FACE_OUTER_BOUND('',#4305,.T.);
#2392=FACE_OUTER_BOUND('',#4306,.T.);
#2393=FACE_OUTER_BOUND('',#4307,.T.);
#2394=FACE_OUTER_BOUND('',#4308,.T.);
#2395=FACE_OUTER_BOUND('',#4309,.T.);
#2396=FACE_OUTER_BOUND('',#4310,.T.);
#2397=FACE_OUTER_BOUND('',#4311,.T.);
#2398=FACE_OUTER_BOUND('',#4312,.T.);
#2399=FACE_OUTER_BOUND('',#4313,.T.);
#2400=FACE_OUTER_BOUND('',#4314,.T.);
#2401=FACE_OUTER_BOUND('',#4315,.T.);
#2402=FACE_OUTER_BOUND('',#4316,.T.);
#2403=FACE_OUTER_BOUND('',#4317,.T.);
#2404=FACE_OUTER_BOUND('',#4318,.T.);
#2405=FACE_OUTER_BOUND('',#4319,.T.);
#2406=FACE_OUTER_BOUND('',#4320,.T.);
#2407=FACE_OUTER_BOUND('',#4321,.T.);
#2408=FACE_OUTER_BOUND('',#4322,.T.);
#2409=FACE_OUTER_BOUND('',#4323,.T.);
#2410=FACE_OUTER_BOUND('',#4324,.T.);
#2411=FACE_OUTER_BOUND('',#4325,.T.);
#2412=FACE_OUTER_BOUND('',#4326,.T.);
#2413=FACE_OUTER_BOUND('',#4327,.T.);
#2414=FACE_OUTER_BOUND('',#4328,.T.);
#2415=FACE_OUTER_BOUND('',#4329,.T.);
#2416=FACE_OUTER_BOUND('',#4330,.T.);
#2417=FACE_OUTER_BOUND('',#4331,.T.);
#2418=FACE_OUTER_BOUND('',#4332,.T.);
#2419=FACE_OUTER_BOUND('',#4333,.T.);
#2420=FACE_OUTER_BOUND('',#4334,.T.);
#2421=FACE_OUTER_BOUND('',#4335,.T.);
#2422=FACE_OUTER_BOUND('',#4340,.T.);
#2423=FACE_OUTER_BOUND('',#4345,.T.);
#2424=FACE_OUTER_BOUND('',#4346,.T.);
#2425=FACE_OUTER_BOUND('',#4347,.T.);
#2426=FACE_OUTER_BOUND('',#4350,.T.);
#2427=FACE_OUTER_BOUND('',#4353,.T.);
#2428=FACE_OUTER_BOUND('',#4354,.T.);
#2429=FACE_OUTER_BOUND('',#4355,.T.);
#2430=FACE_OUTER_BOUND('',#4404,.T.);
#2431=FACE_OUTER_BOUND('',#4453,.T.);
#2432=FACE_OUTER_BOUND('',#4454,.T.);
#2433=FACE_OUTER_BOUND('',#4455,.T.);
#2434=FACE_OUTER_BOUND('',#4456,.T.);
#2435=FACE_OUTER_BOUND('',#4457,.T.);
#2436=FACE_OUTER_BOUND('',#4458,.T.);
#2437=FACE_OUTER_BOUND('',#4459,.T.);
#2438=FACE_OUTER_BOUND('',#4460,.T.);
#2439=FACE_OUTER_BOUND('',#4461,.T.);
#2440=FACE_OUTER_BOUND('',#4462,.T.);
#2441=FACE_OUTER_BOUND('',#4463,.T.);
#2442=FACE_OUTER_BOUND('',#4464,.T.);
#2443=FACE_OUTER_BOUND('',#4465,.T.);
#2444=FACE_OUTER_BOUND('',#4466,.T.);
#2445=FACE_OUTER_BOUND('',#4467,.T.);
#2446=FACE_OUTER_BOUND('',#4468,.T.);
#2447=FACE_OUTER_BOUND('',#4469,.T.);
#2448=FACE_OUTER_BOUND('',#4470,.T.);
#2449=FACE_OUTER_BOUND('',#4471,.T.);
#2450=FACE_OUTER_BOUND('',#4472,.T.);
#2451=FACE_OUTER_BOUND('',#4473,.T.);
#2452=FACE_OUTER_BOUND('',#4474,.T.);
#2453=FACE_OUTER_BOUND('',#4475,.T.);
#2454=FACE_OUTER_BOUND('',#4476,.T.);
#2455=FACE_OUTER_BOUND('',#4477,.T.);
#2456=FACE_OUTER_BOUND('',#4478,.T.);
#2457=FACE_OUTER_BOUND('',#4497,.T.);
#2458=FACE_OUTER_BOUND('',#4498,.T.);
#2459=FACE_OUTER_BOUND('',#4499,.T.);
#2460=FACE_OUTER_BOUND('',#4500,.T.);
#2461=FACE_OUTER_BOUND('',#4501,.T.);
#2462=FACE_OUTER_BOUND('',#4502,.T.);
#2463=FACE_OUTER_BOUND('',#4514,.T.);
#2464=FACE_OUTER_BOUND('',#4526,.T.);
#2465=FACE_OUTER_BOUND('',#4527,.T.);
#2466=FACE_OUTER_BOUND('',#4528,.T.);
#2467=FACE_OUTER_BOUND('',#4529,.T.);
#2468=FACE_OUTER_BOUND('',#4530,.T.);
#2469=FACE_OUTER_BOUND('',#4531,.T.);
#2470=FACE_OUTER_BOUND('',#4532,.T.);
#2471=FACE_OUTER_BOUND('',#4533,.T.);
#2472=FACE_OUTER_BOUND('',#4534,.T.);
#2473=FACE_OUTER_BOUND('',#4535,.T.);
#2474=FACE_OUTER_BOUND('',#4536,.T.);
#2475=FACE_OUTER_BOUND('',#4537,.T.);
#2476=FACE_OUTER_BOUND('',#4538,.T.);
#2477=FACE_OUTER_BOUND('',#4539,.T.);
#2478=FACE_OUTER_BOUND('',#4540,.T.);
#2479=FACE_OUTER_BOUND('',#4541,.T.);
#2480=FACE_OUTER_BOUND('',#4542,.T.);
#2481=FACE_OUTER_BOUND('',#4543,.T.);
#2482=FACE_OUTER_BOUND('',#4544,.T.);
#2483=FACE_OUTER_BOUND('',#4545,.T.);
#2484=FACE_OUTER_BOUND('',#4546,.T.);
#2485=FACE_OUTER_BOUND('',#4547,.T.);
#2486=FACE_OUTER_BOUND('',#4548,.T.);
#2487=FACE_OUTER_BOUND('',#4549,.T.);
#2488=FACE_OUTER_BOUND('',#4550,.T.);
#2489=FACE_OUTER_BOUND('',#4551,.T.);
#2490=FACE_OUTER_BOUND('',#4552,.T.);
#2491=FACE_OUTER_BOUND('',#4553,.T.);
#2492=FACE_OUTER_BOUND('',#4554,.T.);
#2493=FACE_OUTER_BOUND('',#4555,.T.);
#2494=FACE_OUTER_BOUND('',#4556,.T.);
#2495=FACE_OUTER_BOUND('',#4557,.T.);
#2496=FACE_OUTER_BOUND('',#4558,.T.);
#2497=FACE_OUTER_BOUND('',#4559,.T.);
#2498=FACE_OUTER_BOUND('',#4560,.T.);
#2499=FACE_OUTER_BOUND('',#4561,.T.);
#2500=FACE_OUTER_BOUND('',#4562,.T.);
#2501=FACE_OUTER_BOUND('',#4563,.T.);
#2502=FACE_OUTER_BOUND('',#4564,.T.);
#2503=FACE_OUTER_BOUND('',#4565,.T.);
#2504=FACE_OUTER_BOUND('',#4566,.T.);
#2505=FACE_OUTER_BOUND('',#4568,.T.);
#2506=FACE_OUTER_BOUND('',#4569,.T.);
#2507=FACE_OUTER_BOUND('',#4570,.T.);
#2508=FACE_OUTER_BOUND('',#4571,.T.);
#2509=FACE_OUTER_BOUND('',#4572,.T.);
#2510=FACE_OUTER_BOUND('',#4573,.T.);
#2511=FACE_OUTER_BOUND('',#4574,.T.);
#2512=FACE_OUTER_BOUND('',#4576,.T.);
#2513=FACE_OUTER_BOUND('',#4577,.T.);
#2514=FACE_OUTER_BOUND('',#4578,.T.);
#2515=FACE_OUTER_BOUND('',#4579,.T.);
#2516=FACE_OUTER_BOUND('',#4580,.T.);
#2517=FACE_OUTER_BOUND('',#4581,.T.);
#2518=FACE_OUTER_BOUND('',#4582,.T.);
#2519=FACE_OUTER_BOUND('',#4583,.T.);
#2520=FACE_OUTER_BOUND('',#4584,.T.);
#2521=FACE_OUTER_BOUND('',#4585,.T.);
#2522=FACE_OUTER_BOUND('',#4586,.T.);
#2523=FACE_OUTER_BOUND('',#4588,.T.);
#2524=FACE_OUTER_BOUND('',#4589,.T.);
#2525=FACE_OUTER_BOUND('',#4590,.T.);
#2526=FACE_OUTER_BOUND('',#4591,.T.);
#2527=FACE_OUTER_BOUND('',#4592,.T.);
#2528=FACE_OUTER_BOUND('',#4593,.T.);
#2529=FACE_OUTER_BOUND('',#4594,.T.);
#2530=FACE_OUTER_BOUND('',#4596,.T.);
#2531=FACE_OUTER_BOUND('',#4597,.T.);
#2532=FACE_OUTER_BOUND('',#4598,.T.);
#2533=FACE_OUTER_BOUND('',#4599,.T.);
#2534=FACE_OUTER_BOUND('',#4600,.T.);
#2535=FACE_OUTER_BOUND('',#4601,.T.);
#2536=FACE_OUTER_BOUND('',#4602,.T.);
#2537=FACE_OUTER_BOUND('',#4603,.T.);
#2538=FACE_OUTER_BOUND('',#4604,.T.);
#2539=FACE_OUTER_BOUND('',#4605,.T.);
#2540=FACE_OUTER_BOUND('',#4606,.T.);
#2541=FACE_OUTER_BOUND('',#4608,.T.);
#2542=FACE_OUTER_BOUND('',#4609,.T.);
#2543=FACE_OUTER_BOUND('',#4610,.T.);
#2544=FACE_OUTER_BOUND('',#4611,.T.);
#2545=FACE_OUTER_BOUND('',#4612,.T.);
#2546=FACE_OUTER_BOUND('',#4613,.T.);
#2547=FACE_OUTER_BOUND('',#4614,.T.);
#2548=FACE_OUTER_BOUND('',#4616,.T.);
#2549=FACE_OUTER_BOUND('',#4617,.T.);
#2550=FACE_OUTER_BOUND('',#4618,.T.);
#2551=FACE_OUTER_BOUND('',#4619,.T.);
#2552=FACE_OUTER_BOUND('',#4620,.T.);
#2553=FACE_OUTER_BOUND('',#4621,.T.);
#2554=FACE_OUTER_BOUND('',#4622,.T.);
#2555=FACE_OUTER_BOUND('',#4623,.T.);
#2556=FACE_OUTER_BOUND('',#4624,.T.);
#2557=FACE_OUTER_BOUND('',#4625,.T.);
#2558=FACE_OUTER_BOUND('',#4626,.T.);
#2559=FACE_OUTER_BOUND('',#4628,.T.);
#2560=FACE_OUTER_BOUND('',#4629,.T.);
#2561=FACE_OUTER_BOUND('',#4630,.T.);
#2562=FACE_OUTER_BOUND('',#4631,.T.);
#2563=FACE_OUTER_BOUND('',#4632,.T.);
#2564=FACE_OUTER_BOUND('',#4633,.T.);
#2565=FACE_OUTER_BOUND('',#4634,.T.);
#2566=FACE_OUTER_BOUND('',#4636,.T.);
#2567=FACE_OUTER_BOUND('',#4655,.T.);
#2568=FACE_OUTER_BOUND('',#4656,.T.);
#2569=FACE_OUTER_BOUND('',#4657,.T.);
#2570=FACE_OUTER_BOUND('',#4658,.T.);
#2571=FACE_OUTER_BOUND('',#4659,.T.);
#2572=FACE_OUTER_BOUND('',#4660,.T.);
#2573=FACE_OUTER_BOUND('',#4661,.T.);
#2574=FACE_OUTER_BOUND('',#4662,.T.);
#2575=FACE_OUTER_BOUND('',#4663,.T.);
#2576=FACE_OUTER_BOUND('',#4664,.T.);
#2577=FACE_OUTER_BOUND('',#4665,.T.);
#2578=FACE_OUTER_BOUND('',#4666,.T.);
#2579=FACE_OUTER_BOUND('',#4667,.T.);
#2580=FACE_OUTER_BOUND('',#4668,.T.);
#2581=FACE_OUTER_BOUND('',#4669,.T.);
#2582=FACE_OUTER_BOUND('',#4670,.T.);
#2583=FACE_OUTER_BOUND('',#4671,.T.);
#2584=FACE_OUTER_BOUND('',#4672,.T.);
#2585=FACE_OUTER_BOUND('',#4673,.T.);
#2586=FACE_OUTER_BOUND('',#4674,.T.);
#2587=FACE_OUTER_BOUND('',#4675,.T.);
#2588=FACE_OUTER_BOUND('',#4676,.T.);
#2589=FACE_OUTER_BOUND('',#4677,.T.);
#2590=FACE_OUTER_BOUND('',#4678,.T.);
#2591=FACE_OUTER_BOUND('',#4679,.T.);
#2592=FACE_OUTER_BOUND('',#4680,.T.);
#2593=FACE_OUTER_BOUND('',#4681,.T.);
#2594=FACE_OUTER_BOUND('',#4682,.T.);
#2595=FACE_OUTER_BOUND('',#4683,.T.);
#2596=FACE_OUTER_BOUND('',#4684,.T.);
#2597=FACE_OUTER_BOUND('',#4685,.T.);
#2598=FACE_OUTER_BOUND('',#4686,.T.);
#2599=FACE_OUTER_BOUND('',#4687,.T.);
#2600=FACE_OUTER_BOUND('',#4688,.T.);
#2601=FACE_OUTER_BOUND('',#4689,.T.);
#2602=FACE_OUTER_BOUND('',#4690,.T.);
#2603=FACE_OUTER_BOUND('',#4691,.T.);
#2604=FACE_OUTER_BOUND('',#4692,.T.);
#2605=FACE_OUTER_BOUND('',#4693,.T.);
#2606=FACE_OUTER_BOUND('',#4694,.T.);
#2607=FACE_OUTER_BOUND('',#4695,.T.);
#2608=FACE_OUTER_BOUND('',#4696,.T.);
#2609=FACE_OUTER_BOUND('',#4697,.T.);
#2610=FACE_OUTER_BOUND('',#4698,.T.);
#2611=FACE_OUTER_BOUND('',#4699,.T.);
#2612=FACE_OUTER_BOUND('',#4700,.T.);
#2613=FACE_OUTER_BOUND('',#4701,.T.);
#2614=FACE_OUTER_BOUND('',#4702,.T.);
#2615=FACE_OUTER_BOUND('',#4703,.T.);
#2616=FACE_OUTER_BOUND('',#4704,.T.);
#2617=FACE_OUTER_BOUND('',#4705,.T.);
#2618=FACE_OUTER_BOUND('',#4706,.T.);
#2619=FACE_OUTER_BOUND('',#4707,.T.);
#2620=FACE_OUTER_BOUND('',#4708,.T.);
#2621=FACE_OUTER_BOUND('',#4709,.T.);
#2622=FACE_OUTER_BOUND('',#4710,.T.);
#2623=FACE_OUTER_BOUND('',#4711,.T.);
#2624=FACE_OUTER_BOUND('',#4712,.T.);
#2625=FACE_OUTER_BOUND('',#4713,.T.);
#2626=FACE_OUTER_BOUND('',#4714,.T.);
#2627=FACE_OUTER_BOUND('',#4715,.T.);
#2628=FACE_OUTER_BOUND('',#4716,.T.);
#2629=FACE_OUTER_BOUND('',#4717,.T.);
#2630=FACE_OUTER_BOUND('',#4718,.T.);
#2631=FACE_OUTER_BOUND('',#4719,.T.);
#2632=FACE_OUTER_BOUND('',#4720,.T.);
#2633=FACE_OUTER_BOUND('',#4721,.T.);
#2634=FACE_OUTER_BOUND('',#4722,.T.);
#2635=FACE_OUTER_BOUND('',#4723,.T.);
#2636=FACE_OUTER_BOUND('',#4724,.T.);
#2637=FACE_OUTER_BOUND('',#4725,.T.);
#2638=FACE_OUTER_BOUND('',#4726,.T.);
#2639=FACE_OUTER_BOUND('',#4727,.T.);
#2640=FACE_OUTER_BOUND('',#4728,.T.);
#2641=FACE_OUTER_BOUND('',#4729,.T.);
#2642=FACE_OUTER_BOUND('',#4730,.T.);
#2643=FACE_OUTER_BOUND('',#4731,.T.);
#2644=FACE_OUTER_BOUND('',#4732,.T.);
#2645=FACE_OUTER_BOUND('',#4733,.T.);
#2646=FACE_OUTER_BOUND('',#4734,.T.);
#2647=FACE_OUTER_BOUND('',#4735,.T.);
#2648=FACE_OUTER_BOUND('',#4736,.T.);
#2649=FACE_OUTER_BOUND('',#4737,.T.);
#2650=FACE_OUTER_BOUND('',#4738,.T.);
#2651=FACE_OUTER_BOUND('',#4739,.T.);
#2652=FACE_OUTER_BOUND('',#4740,.T.);
#2653=FACE_OUTER_BOUND('',#4741,.T.);
#2654=FACE_OUTER_BOUND('',#4742,.T.);
#2655=FACE_OUTER_BOUND('',#4743,.T.);
#2656=FACE_OUTER_BOUND('',#4744,.T.);
#2657=FACE_OUTER_BOUND('',#4745,.T.);
#2658=FACE_OUTER_BOUND('',#4746,.T.);
#2659=FACE_OUTER_BOUND('',#4747,.T.);
#2660=FACE_OUTER_BOUND('',#4748,.T.);
#2661=FACE_OUTER_BOUND('',#4749,.T.);
#2662=FACE_OUTER_BOUND('',#4750,.T.);
#2663=FACE_OUTER_BOUND('',#4751,.T.);
#2664=FACE_OUTER_BOUND('',#4752,.T.);
#2665=FACE_OUTER_BOUND('',#4753,.T.);
#2666=FACE_OUTER_BOUND('',#4754,.T.);
#2667=FACE_OUTER_BOUND('',#4755,.T.);
#2668=FACE_OUTER_BOUND('',#4756,.T.);
#2669=FACE_OUTER_BOUND('',#4757,.T.);
#2670=FACE_OUTER_BOUND('',#4758,.T.);
#2671=FACE_OUTER_BOUND('',#4759,.T.);
#2672=FACE_OUTER_BOUND('',#4760,.T.);
#2673=FACE_OUTER_BOUND('',#4761,.T.);
#2674=FACE_OUTER_BOUND('',#4762,.T.);
#2675=FACE_OUTER_BOUND('',#4763,.T.);
#2676=FACE_OUTER_BOUND('',#4764,.T.);
#2677=FACE_OUTER_BOUND('',#4765,.T.);
#2678=FACE_OUTER_BOUND('',#4766,.T.);
#2679=FACE_OUTER_BOUND('',#4767,.T.);
#2680=FACE_OUTER_BOUND('',#4768,.T.);
#2681=FACE_OUTER_BOUND('',#4769,.T.);
#2682=FACE_OUTER_BOUND('',#4770,.T.);
#2683=FACE_OUTER_BOUND('',#4771,.T.);
#2684=FACE_OUTER_BOUND('',#4772,.T.);
#2685=FACE_OUTER_BOUND('',#4773,.T.);
#2686=FACE_OUTER_BOUND('',#4774,.T.);
#2687=FACE_OUTER_BOUND('',#4775,.T.);
#2688=FACE_OUTER_BOUND('',#4776,.T.);
#2689=FACE_OUTER_BOUND('',#4777,.T.);
#2690=FACE_OUTER_BOUND('',#4778,.T.);
#2691=FACE_OUTER_BOUND('',#4779,.T.);
#2692=FACE_OUTER_BOUND('',#4780,.T.);
#2693=FACE_OUTER_BOUND('',#4781,.T.);
#2694=FACE_OUTER_BOUND('',#4782,.T.);
#2695=FACE_OUTER_BOUND('',#4783,.T.);
#2696=FACE_OUTER_BOUND('',#4784,.T.);
#2697=FACE_OUTER_BOUND('',#4785,.T.);
#2698=FACE_OUTER_BOUND('',#4786,.T.);
#2699=FACE_OUTER_BOUND('',#4787,.T.);
#2700=FACE_OUTER_BOUND('',#4788,.T.);
#2701=FACE_OUTER_BOUND('',#4789,.T.);
#2702=FACE_OUTER_BOUND('',#4790,.T.);
#2703=FACE_OUTER_BOUND('',#4791,.T.);
#2704=FACE_OUTER_BOUND('',#4792,.T.);
#2705=FACE_OUTER_BOUND('',#4793,.T.);
#2706=FACE_OUTER_BOUND('',#4794,.T.);
#2707=FACE_OUTER_BOUND('',#4795,.T.);
#2708=FACE_OUTER_BOUND('',#4796,.T.);
#2709=FACE_OUTER_BOUND('',#4797,.T.);
#2710=FACE_OUTER_BOUND('',#4798,.T.);
#2711=FACE_OUTER_BOUND('',#4799,.T.);
#2712=FACE_OUTER_BOUND('',#4800,.T.);
#2713=FACE_OUTER_BOUND('',#4801,.T.);
#2714=FACE_OUTER_BOUND('',#4802,.T.);
#2715=FACE_OUTER_BOUND('',#4803,.T.);
#2716=FACE_OUTER_BOUND('',#4804,.T.);
#2717=FACE_OUTER_BOUND('',#4805,.T.);
#2718=FACE_OUTER_BOUND('',#4806,.T.);
#2719=FACE_OUTER_BOUND('',#4807,.T.);
#2720=FACE_OUTER_BOUND('',#4808,.T.);
#2721=FACE_OUTER_BOUND('',#4809,.T.);
#2722=FACE_OUTER_BOUND('',#4810,.T.);
#2723=FACE_OUTER_BOUND('',#4811,.T.);
#2724=FACE_OUTER_BOUND('',#4812,.T.);
#2725=FACE_OUTER_BOUND('',#4813,.T.);
#2726=FACE_OUTER_BOUND('',#4814,.T.);
#2727=FACE_OUTER_BOUND('',#4815,.T.);
#2728=FACE_OUTER_BOUND('',#4816,.T.);
#2729=FACE_OUTER_BOUND('',#4817,.T.);
#2730=FACE_OUTER_BOUND('',#4818,.T.);
#2731=FACE_OUTER_BOUND('',#4819,.T.);
#2732=FACE_OUTER_BOUND('',#4820,.T.);
#2733=FACE_OUTER_BOUND('',#4821,.T.);
#2734=FACE_OUTER_BOUND('',#4822,.T.);
#2735=FACE_OUTER_BOUND('',#4823,.T.);
#2736=FACE_OUTER_BOUND('',#4824,.T.);
#2737=FACE_OUTER_BOUND('',#4825,.T.);
#2738=FACE_OUTER_BOUND('',#4826,.T.);
#2739=FACE_OUTER_BOUND('',#4827,.T.);
#2740=FACE_OUTER_BOUND('',#4828,.T.);
#2741=FACE_OUTER_BOUND('',#4829,.T.);
#2742=FACE_OUTER_BOUND('',#4830,.T.);
#2743=FACE_OUTER_BOUND('',#4831,.T.);
#2744=FACE_OUTER_BOUND('',#4832,.T.);
#2745=FACE_OUTER_BOUND('',#4833,.T.);
#2746=FACE_OUTER_BOUND('',#4834,.T.);
#2747=FACE_OUTER_BOUND('',#4835,.T.);
#2748=FACE_OUTER_BOUND('',#4836,.T.);
#2749=FACE_OUTER_BOUND('',#4837,.T.);
#2750=FACE_OUTER_BOUND('',#4838,.T.);
#2751=FACE_OUTER_BOUND('',#4839,.T.);
#2752=FACE_OUTER_BOUND('',#4840,.T.);
#2753=FACE_OUTER_BOUND('',#4841,.T.);
#2754=FACE_OUTER_BOUND('',#4842,.T.);
#2755=FACE_OUTER_BOUND('',#4843,.T.);
#2756=FACE_OUTER_BOUND('',#4844,.T.);
#2757=FACE_OUTER_BOUND('',#4845,.T.);
#2758=FACE_OUTER_BOUND('',#4846,.T.);
#2759=FACE_OUTER_BOUND('',#4847,.T.);
#2760=FACE_OUTER_BOUND('',#4848,.T.);
#2761=FACE_OUTER_BOUND('',#4849,.T.);
#2762=FACE_OUTER_BOUND('',#4850,.T.);
#2763=FACE_OUTER_BOUND('',#4851,.T.);
#2764=FACE_OUTER_BOUND('',#4852,.T.);
#2765=FACE_OUTER_BOUND('',#4853,.T.);
#2766=FACE_OUTER_BOUND('',#4854,.T.);
#2767=FACE_OUTER_BOUND('',#4855,.T.);
#2768=FACE_OUTER_BOUND('',#4856,.T.);
#2769=FACE_OUTER_BOUND('',#4857,.T.);
#2770=FACE_OUTER_BOUND('',#4858,.T.);
#2771=FACE_OUTER_BOUND('',#4859,.T.);
#2772=FACE_OUTER_BOUND('',#4860,.T.);
#2773=FACE_OUTER_BOUND('',#4861,.T.);
#2774=FACE_OUTER_BOUND('',#4862,.T.);
#2775=FACE_OUTER_BOUND('',#4863,.T.);
#2776=FACE_OUTER_BOUND('',#4864,.T.);
#2777=FACE_OUTER_BOUND('',#4865,.T.);
#2778=FACE_OUTER_BOUND('',#4866,.T.);
#2779=FACE_OUTER_BOUND('',#4867,.T.);
#2780=FACE_OUTER_BOUND('',#4868,.T.);
#2781=FACE_OUTER_BOUND('',#4869,.T.);
#2782=FACE_OUTER_BOUND('',#4870,.T.);
#2783=FACE_OUTER_BOUND('',#4871,.T.);
#2784=FACE_OUTER_BOUND('',#4872,.T.);
#2785=FACE_OUTER_BOUND('',#4873,.T.);
#2786=FACE_OUTER_BOUND('',#4874,.T.);
#2787=FACE_OUTER_BOUND('',#4875,.T.);
#2788=FACE_OUTER_BOUND('',#4876,.T.);
#2789=FACE_OUTER_BOUND('',#4877,.T.);
#2790=FACE_OUTER_BOUND('',#4878,.T.);
#2791=FACE_OUTER_BOUND('',#4879,.T.);
#2792=FACE_OUTER_BOUND('',#4880,.T.);
#2793=FACE_OUTER_BOUND('',#4881,.T.);
#2794=FACE_OUTER_BOUND('',#4882,.T.);
#2795=FACE_OUTER_BOUND('',#4883,.T.);
#2796=FACE_OUTER_BOUND('',#4884,.T.);
#2797=FACE_OUTER_BOUND('',#4885,.T.);
#2798=FACE_OUTER_BOUND('',#4886,.T.);
#2799=FACE_OUTER_BOUND('',#4887,.T.);
#2800=FACE_OUTER_BOUND('',#4888,.T.);
#2801=FACE_OUTER_BOUND('',#4889,.T.);
#2802=FACE_OUTER_BOUND('',#4890,.T.);
#2803=FACE_OUTER_BOUND('',#4891,.T.);
#2804=FACE_OUTER_BOUND('',#4892,.T.);
#2805=FACE_OUTER_BOUND('',#4893,.T.);
#2806=FACE_OUTER_BOUND('',#4894,.T.);
#2807=FACE_OUTER_BOUND('',#4895,.T.);
#2808=FACE_OUTER_BOUND('',#4896,.T.);
#2809=FACE_OUTER_BOUND('',#4897,.T.);
#2810=FACE_OUTER_BOUND('',#4898,.T.);
#2811=FACE_OUTER_BOUND('',#4899,.T.);
#2812=FACE_OUTER_BOUND('',#4900,.T.);
#2813=FACE_OUTER_BOUND('',#4901,.T.);
#2814=FACE_OUTER_BOUND('',#4902,.T.);
#2815=FACE_OUTER_BOUND('',#4903,.T.);
#2816=FACE_OUTER_BOUND('',#4904,.T.);
#2817=FACE_OUTER_BOUND('',#4905,.T.);
#2818=FACE_OUTER_BOUND('',#4906,.T.);
#2819=FACE_OUTER_BOUND('',#4907,.T.);
#2820=FACE_OUTER_BOUND('',#4908,.T.);
#2821=FACE_OUTER_BOUND('',#4909,.T.);
#2822=FACE_OUTER_BOUND('',#4910,.T.);
#2823=FACE_OUTER_BOUND('',#4911,.T.);
#2824=FACE_OUTER_BOUND('',#4912,.T.);
#2825=FACE_OUTER_BOUND('',#4913,.T.);
#2826=FACE_OUTER_BOUND('',#4914,.T.);
#2827=FACE_OUTER_BOUND('',#4915,.T.);
#2828=FACE_OUTER_BOUND('',#4916,.T.);
#2829=FACE_OUTER_BOUND('',#4917,.T.);
#2830=FACE_OUTER_BOUND('',#4918,.T.);
#2831=FACE_OUTER_BOUND('',#4919,.T.);
#2832=FACE_OUTER_BOUND('',#4920,.T.);
#2833=FACE_OUTER_BOUND('',#4921,.T.);
#2834=FACE_OUTER_BOUND('',#4922,.T.);
#2835=FACE_OUTER_BOUND('',#4923,.T.);
#2836=FACE_OUTER_BOUND('',#4924,.T.);
#2837=FACE_OUTER_BOUND('',#4925,.T.);
#2838=FACE_OUTER_BOUND('',#4926,.T.);
#2839=FACE_OUTER_BOUND('',#4927,.T.);
#2840=FACE_OUTER_BOUND('',#4928,.T.);
#2841=FACE_OUTER_BOUND('',#4929,.T.);
#2842=FACE_OUTER_BOUND('',#4930,.T.);
#2843=FACE_OUTER_BOUND('',#4931,.T.);
#2844=FACE_OUTER_BOUND('',#4932,.T.);
#2845=FACE_OUTER_BOUND('',#4933,.T.);
#2846=FACE_OUTER_BOUND('',#4934,.T.);
#2847=FACE_OUTER_BOUND('',#4935,.T.);
#2848=FACE_OUTER_BOUND('',#4936,.T.);
#2849=FACE_OUTER_BOUND('',#4937,.T.);
#2850=FACE_OUTER_BOUND('',#4938,.T.);
#2851=FACE_OUTER_BOUND('',#4939,.T.);
#2852=FACE_OUTER_BOUND('',#4940,.T.);
#2853=FACE_OUTER_BOUND('',#4942,.T.);
#2854=FACE_OUTER_BOUND('',#4943,.T.);
#2855=FACE_OUTER_BOUND('',#4944,.T.);
#2856=FACE_OUTER_BOUND('',#4945,.T.);
#2857=FACE_OUTER_BOUND('',#4946,.T.);
#2858=FACE_OUTER_BOUND('',#4947,.T.);
#2859=FACE_OUTER_BOUND('',#4948,.T.);
#2860=FACE_OUTER_BOUND('',#4950,.T.);
#2861=FACE_OUTER_BOUND('',#4951,.T.);
#2862=FACE_OUTER_BOUND('',#4952,.T.);
#2863=FACE_OUTER_BOUND('',#4953,.T.);
#2864=FACE_OUTER_BOUND('',#4954,.T.);
#2865=FACE_OUTER_BOUND('',#4955,.T.);
#2866=FACE_OUTER_BOUND('',#4956,.T.);
#2867=FACE_OUTER_BOUND('',#4957,.T.);
#2868=FACE_OUTER_BOUND('',#4958,.T.);
#2869=FACE_OUTER_BOUND('',#4959,.T.);
#2870=FACE_OUTER_BOUND('',#4960,.T.);
#2871=FACE_OUTER_BOUND('',#4962,.T.);
#2872=FACE_OUTER_BOUND('',#4963,.T.);
#2873=FACE_OUTER_BOUND('',#4964,.T.);
#2874=FACE_OUTER_BOUND('',#4965,.T.);
#2875=FACE_OUTER_BOUND('',#4966,.T.);
#2876=FACE_OUTER_BOUND('',#4967,.T.);
#2877=FACE_OUTER_BOUND('',#4968,.T.);
#2878=FACE_OUTER_BOUND('',#4970,.T.);
#2879=FACE_OUTER_BOUND('',#4971,.T.);
#2880=FACE_OUTER_BOUND('',#4972,.T.);
#2881=FACE_OUTER_BOUND('',#4973,.T.);
#2882=FACE_OUTER_BOUND('',#4974,.T.);
#2883=FACE_OUTER_BOUND('',#4975,.T.);
#2884=FACE_OUTER_BOUND('',#4976,.T.);
#2885=FACE_OUTER_BOUND('',#4977,.T.);
#2886=FACE_OUTER_BOUND('',#4978,.T.);
#2887=FACE_OUTER_BOUND('',#4979,.T.);
#2888=FACE_OUTER_BOUND('',#4980,.T.);
#2889=FACE_OUTER_BOUND('',#4981,.T.);
#2890=FACE_OUTER_BOUND('',#4982,.T.);
#2891=FACE_OUTER_BOUND('',#4983,.T.);
#2892=FACE_OUTER_BOUND('',#4984,.T.);
#2893=FACE_OUTER_BOUND('',#4985,.T.);
#2894=FACE_OUTER_BOUND('',#4986,.T.);
#2895=FACE_OUTER_BOUND('',#4987,.T.);
#2896=FACE_OUTER_BOUND('',#4988,.T.);
#2897=FACE_OUTER_BOUND('',#4989,.T.);
#2898=FACE_OUTER_BOUND('',#4990,.T.);
#2899=FACE_OUTER_BOUND('',#4991,.T.);
#2900=FACE_OUTER_BOUND('',#4992,.T.);
#2901=FACE_OUTER_BOUND('',#4993,.T.);
#2902=FACE_OUTER_BOUND('',#4994,.T.);
#2903=FACE_OUTER_BOUND('',#4995,.T.);
#2904=FACE_OUTER_BOUND('',#4999,.T.);
#2905=FACE_OUTER_BOUND('',#5000,.T.);
#2906=FACE_OUTER_BOUND('',#5001,.T.);
#2907=FACE_OUTER_BOUND('',#5002,.T.);
#2908=FACE_OUTER_BOUND('',#5003,.T.);
#2909=FACE_OUTER_BOUND('',#5004,.T.);
#2910=FACE_OUTER_BOUND('',#5005,.T.);
#2911=FACE_OUTER_BOUND('',#5006,.T.);
#2912=FACE_OUTER_BOUND('',#5007,.T.);
#2913=FACE_OUTER_BOUND('',#5008,.T.);
#2914=FACE_OUTER_BOUND('',#5009,.T.);
#2915=FACE_OUTER_BOUND('',#5010,.T.);
#2916=FACE_OUTER_BOUND('',#5011,.T.);
#2917=FACE_OUTER_BOUND('',#5015,.T.);
#2918=FACE_OUTER_BOUND('',#5017,.T.);
#2919=FACE_OUTER_BOUND('',#5021,.T.);
#2920=FACE_OUTER_BOUND('',#5022,.T.);
#2921=FACE_OUTER_BOUND('',#5023,.T.);
#2922=FACE_OUTER_BOUND('',#5024,.T.);
#2923=FACE_OUTER_BOUND('',#5025,.T.);
#2924=FACE_OUTER_BOUND('',#5026,.T.);
#2925=FACE_OUTER_BOUND('',#5027,.T.);
#2926=FACE_OUTER_BOUND('',#5028,.T.);
#2927=FACE_OUTER_BOUND('',#5029,.T.);
#2928=FACE_OUTER_BOUND('',#5030,.T.);
#2929=FACE_OUTER_BOUND('',#5031,.T.);
#2930=FACE_OUTER_BOUND('',#5032,.T.);
#2931=FACE_OUTER_BOUND('',#5034,.T.);
#2932=FACE_OUTER_BOUND('',#5035,.T.);
#2933=FACE_OUTER_BOUND('',#5036,.T.);
#2934=FACE_OUTER_BOUND('',#5038,.T.);
#2935=FACE_OUTER_BOUND('',#5039,.T.);
#2936=FACE_OUTER_BOUND('',#5040,.T.);
#2937=FACE_OUTER_BOUND('',#5041,.T.);
#2938=FACE_OUTER_BOUND('',#5042,.T.);
#2939=FACE_OUTER_BOUND('',#5043,.T.);
#2940=FACE_OUTER_BOUND('',#5044,.T.);
#2941=FACE_OUTER_BOUND('',#5045,.T.);
#2942=FACE_OUTER_BOUND('',#5046,.T.);
#2943=FACE_OUTER_BOUND('',#5047,.T.);
#2944=FACE_OUTER_BOUND('',#5048,.T.);
#2945=FACE_OUTER_BOUND('',#5049,.T.);
#2946=FACE_OUTER_BOUND('',#5050,.T.);
#2947=FACE_OUTER_BOUND('',#5051,.T.);
#2948=FACE_OUTER_BOUND('',#5052,.T.);
#2949=FACE_OUTER_BOUND('',#5053,.T.);
#2950=FACE_OUTER_BOUND('',#5054,.T.);
#2951=FACE_OUTER_BOUND('',#5055,.T.);
#2952=FACE_OUTER_BOUND('',#5056,.T.);
#2953=FACE_OUTER_BOUND('',#5057,.T.);
#2954=FACE_OUTER_BOUND('',#5058,.T.);
#2955=FACE_OUTER_BOUND('',#5059,.T.);
#2956=FACE_OUTER_BOUND('',#5060,.T.);
#2957=FACE_OUTER_BOUND('',#5061,.T.);
#2958=FACE_OUTER_BOUND('',#5062,.T.);
#2959=FACE_OUTER_BOUND('',#5063,.T.);
#2960=FACE_OUTER_BOUND('',#5064,.T.);
#2961=FACE_OUTER_BOUND('',#5065,.T.);
#2962=FACE_OUTER_BOUND('',#5066,.T.);
#2963=FACE_OUTER_BOUND('',#5067,.T.);
#2964=FACE_OUTER_BOUND('',#5068,.T.);
#2965=FACE_OUTER_BOUND('',#5069,.T.);
#2966=FACE_OUTER_BOUND('',#5070,.T.);
#2967=FACE_OUTER_BOUND('',#5071,.T.);
#2968=FACE_OUTER_BOUND('',#5072,.T.);
#2969=FACE_OUTER_BOUND('',#5073,.T.);
#2970=FACE_OUTER_BOUND('',#5074,.T.);
#2971=FACE_OUTER_BOUND('',#5075,.T.);
#2972=FACE_OUTER_BOUND('',#5076,.T.);
#2973=FACE_OUTER_BOUND('',#5077,.T.);
#2974=FACE_OUTER_BOUND('',#5078,.T.);
#2975=FACE_OUTER_BOUND('',#5079,.T.);
#2976=FACE_OUTER_BOUND('',#5081,.T.);
#2977=FACE_OUTER_BOUND('',#5082,.T.);
#2978=FACE_OUTER_BOUND('',#5083,.T.);
#2979=FACE_OUTER_BOUND('',#5084,.T.);
#2980=FACE_OUTER_BOUND('',#5085,.T.);
#2981=FACE_OUTER_BOUND('',#5086,.T.);
#2982=FACE_OUTER_BOUND('',#5087,.T.);
#2983=FACE_OUTER_BOUND('',#5088,.T.);
#2984=FACE_OUTER_BOUND('',#5089,.T.);
#2985=FACE_OUTER_BOUND('',#5091,.T.);
#2986=FACE_OUTER_BOUND('',#5092,.T.);
#2987=FACE_OUTER_BOUND('',#5094,.T.);
#2988=FACE_OUTER_BOUND('',#5095,.T.);
#2989=FACE_OUTER_BOUND('',#5096,.T.);
#2990=FACE_OUTER_BOUND('',#5097,.T.);
#2991=FACE_OUTER_BOUND('',#5098,.T.);
#2992=FACE_OUTER_BOUND('',#5100,.T.);
#2993=FACE_OUTER_BOUND('',#5101,.T.);
#2994=FACE_OUTER_BOUND('',#5102,.T.);
#2995=FACE_OUTER_BOUND('',#5103,.T.);
#2996=FACE_OUTER_BOUND('',#5104,.T.);
#2997=FACE_OUTER_BOUND('',#5105,.T.);
#2998=FACE_OUTER_BOUND('',#5107,.T.);
#2999=FACE_OUTER_BOUND('',#5109,.T.);
#3000=FACE_OUTER_BOUND('',#5111,.T.);
#3001=FACE_OUTER_BOUND('',#5112,.T.);
#3002=FACE_OUTER_BOUND('',#5113,.T.);
#3003=FACE_OUTER_BOUND('',#5114,.T.);
#3004=FACE_OUTER_BOUND('',#5115,.T.);
#3005=FACE_OUTER_BOUND('',#5116,.T.);
#3006=FACE_OUTER_BOUND('',#5117,.T.);
#3007=FACE_OUTER_BOUND('',#5118,.T.);
#3008=FACE_OUTER_BOUND('',#5119,.T.);
#3009=FACE_OUTER_BOUND('',#5120,.T.);
#3010=FACE_OUTER_BOUND('',#5122,.T.);
#3011=FACE_OUTER_BOUND('',#5124,.T.);
#3012=FACE_OUTER_BOUND('',#5125,.T.);
#3013=FACE_OUTER_BOUND('',#5126,.T.);
#3014=FACE_OUTER_BOUND('',#5127,.T.);
#3015=FACE_OUTER_BOUND('',#5128,.T.);
#3016=FACE_OUTER_BOUND('',#5129,.T.);
#3017=FACE_OUTER_BOUND('',#5130,.T.);
#3018=FACE_OUTER_BOUND('',#5131,.T.);
#3019=FACE_OUTER_BOUND('',#5132,.T.);
#3020=FACE_OUTER_BOUND('',#5133,.T.);
#3021=FACE_OUTER_BOUND('',#5134,.T.);
#3022=FACE_OUTER_BOUND('',#5135,.T.);
#3023=FACE_OUTER_BOUND('',#5136,.T.);
#3024=FACE_OUTER_BOUND('',#5137,.T.);
#3025=FACE_OUTER_BOUND('',#5138,.T.);
#3026=FACE_OUTER_BOUND('',#5139,.T.);
#3027=FACE_OUTER_BOUND('',#5140,.T.);
#3028=FACE_OUTER_BOUND('',#5141,.T.);
#3029=FACE_OUTER_BOUND('',#5144,.T.);
#3030=FACE_OUTER_BOUND('',#5146,.T.);
#3031=FACE_OUTER_BOUND('',#5147,.T.);
#3032=FACE_OUTER_BOUND('',#5148,.T.);
#3033=FACE_OUTER_BOUND('',#5149,.T.);
#3034=FACE_OUTER_BOUND('',#5150,.T.);
#3035=FACE_OUTER_BOUND('',#5152,.T.);
#3036=FACE_OUTER_BOUND('',#5153,.T.);
#3037=FACE_OUTER_BOUND('',#5154,.T.);
#3038=FACE_OUTER_BOUND('',#5155,.T.);
#3039=FACE_OUTER_BOUND('',#5156,.T.);
#3040=FACE_OUTER_BOUND('',#5157,.T.);
#3041=FACE_OUTER_BOUND('',#5158,.T.);
#3042=FACE_OUTER_BOUND('',#5159,.T.);
#3043=FACE_OUTER_BOUND('',#5160,.T.);
#3044=FACE_OUTER_BOUND('',#5161,.T.);
#3045=FACE_OUTER_BOUND('',#5162,.T.);
#3046=FACE_OUTER_BOUND('',#5163,.T.);
#3047=FACE_OUTER_BOUND('',#5164,.T.);
#3048=FACE_OUTER_BOUND('',#5165,.T.);
#3049=FACE_OUTER_BOUND('',#5166,.T.);
#3050=FACE_OUTER_BOUND('',#5168,.T.);
#3051=FACE_OUTER_BOUND('',#5170,.T.);
#3052=FACE_OUTER_BOUND('',#5171,.T.);
#3053=FACE_OUTER_BOUND('',#5173,.T.);
#3054=FACE_OUTER_BOUND('',#5175,.T.);
#3055=FACE_OUTER_BOUND('',#5176,.T.);
#3056=FACE_OUTER_BOUND('',#5177,.T.);
#3057=FACE_OUTER_BOUND('',#5178,.T.);
#3058=FACE_OUTER_BOUND('',#5179,.T.);
#3059=FACE_OUTER_BOUND('',#5180,.T.);
#3060=FACE_OUTER_BOUND('',#5181,.T.);
#3061=FACE_OUTER_BOUND('',#5182,.T.);
#3062=FACE_OUTER_BOUND('',#5183,.T.);
#3063=FACE_OUTER_BOUND('',#5184,.T.);
#3064=FACE_OUTER_BOUND('',#5185,.T.);
#3065=FACE_OUTER_BOUND('',#5186,.T.);
#3066=FACE_OUTER_BOUND('',#5187,.T.);
#3067=FACE_OUTER_BOUND('',#5188,.T.);
#3068=FACE_OUTER_BOUND('',#5189,.T.);
#3069=FACE_OUTER_BOUND('',#5190,.T.);
#3070=FACE_OUTER_BOUND('',#5191,.T.);
#3071=FACE_OUTER_BOUND('',#5192,.T.);
#3072=FACE_OUTER_BOUND('',#5193,.T.);
#3073=FACE_OUTER_BOUND('',#5194,.T.);
#3074=FACE_OUTER_BOUND('',#5195,.T.);
#3075=FACE_OUTER_BOUND('',#5196,.T.);
#3076=FACE_OUTER_BOUND('',#5197,.T.);
#3077=FACE_OUTER_BOUND('',#5198,.T.);
#3078=FACE_OUTER_BOUND('',#5199,.T.);
#3079=FACE_OUTER_BOUND('',#5200,.T.);
#3080=FACE_OUTER_BOUND('',#5201,.T.);
#3081=FACE_OUTER_BOUND('',#5202,.T.);
#3082=FACE_OUTER_BOUND('',#5204,.T.);
#3083=FACE_OUTER_BOUND('',#5206,.T.);
#3084=FACE_OUTER_BOUND('',#5207,.T.);
#3085=FACE_OUTER_BOUND('',#5208,.T.);
#3086=FACE_OUTER_BOUND('',#5209,.T.);
#3087=FACE_OUTER_BOUND('',#5210,.T.);
#3088=FACE_OUTER_BOUND('',#5211,.T.);
#3089=FACE_OUTER_BOUND('',#5212,.T.);
#3090=FACE_OUTER_BOUND('',#5213,.T.);
#3091=FACE_OUTER_BOUND('',#5214,.T.);
#3092=FACE_OUTER_BOUND('',#5215,.T.);
#3093=FACE_OUTER_BOUND('',#5216,.T.);
#3094=FACE_OUTER_BOUND('',#5217,.T.);
#3095=FACE_OUTER_BOUND('',#5218,.T.);
#3096=FACE_OUTER_BOUND('',#5219,.T.);
#3097=FACE_OUTER_BOUND('',#5220,.T.);
#3098=FACE_OUTER_BOUND('',#5221,.T.);
#3099=FACE_OUTER_BOUND('',#5222,.T.);
#3100=FACE_OUTER_BOUND('',#5223,.T.);
#3101=FACE_OUTER_BOUND('',#5224,.T.);
#3102=FACE_OUTER_BOUND('',#5225,.T.);
#3103=FACE_OUTER_BOUND('',#5226,.T.);
#3104=FACE_OUTER_BOUND('',#5227,.T.);
#3105=FACE_OUTER_BOUND('',#5228,.T.);
#3106=FACE_OUTER_BOUND('',#5229,.T.);
#3107=FACE_OUTER_BOUND('',#5230,.T.);
#3108=FACE_OUTER_BOUND('',#5231,.T.);
#3109=FACE_OUTER_BOUND('',#5232,.T.);
#3110=FACE_OUTER_BOUND('',#5233,.T.);
#3111=FACE_OUTER_BOUND('',#5234,.T.);
#3112=FACE_OUTER_BOUND('',#5235,.T.);
#3113=FACE_OUTER_BOUND('',#5236,.T.);
#3114=FACE_OUTER_BOUND('',#5237,.T.);
#3115=FACE_OUTER_BOUND('',#5238,.T.);
#3116=FACE_OUTER_BOUND('',#5239,.T.);
#3117=FACE_OUTER_BOUND('',#5240,.T.);
#3118=FACE_OUTER_BOUND('',#5241,.T.);
#3119=FACE_OUTER_BOUND('',#5242,.T.);
#3120=FACE_OUTER_BOUND('',#5243,.T.);
#3121=FACE_OUTER_BOUND('',#5244,.T.);
#3122=FACE_OUTER_BOUND('',#5245,.T.);
#3123=FACE_OUTER_BOUND('',#5246,.T.);
#3124=FACE_OUTER_BOUND('',#5247,.T.);
#3125=FACE_OUTER_BOUND('',#5248,.T.);
#3126=FACE_OUTER_BOUND('',#5249,.T.);
#3127=FACE_OUTER_BOUND('',#5250,.T.);
#3128=FACE_OUTER_BOUND('',#5437,.T.);
#3129=FACE_OUTER_BOUND('',#5624,.T.);
#3130=FACE_OUTER_BOUND('',#5625,.T.);
#3131=FACE_OUTER_BOUND('',#5626,.T.);
#3132=FACE_OUTER_BOUND('',#5627,.T.);
#3133=FACE_OUTER_BOUND('',#5628,.T.);
#3134=FACE_OUTER_BOUND('',#5629,.T.);
#3135=FACE_OUTER_BOUND('',#5630,.T.);
#3136=FACE_OUTER_BOUND('',#5631,.T.);
#3137=FACE_OUTER_BOUND('',#5632,.T.);
#3138=FACE_OUTER_BOUND('',#5633,.T.);
#3139=FACE_OUTER_BOUND('',#5634,.T.);
#3140=FACE_OUTER_BOUND('',#5635,.T.);
#3141=FACE_OUTER_BOUND('',#5636,.T.);
#3142=FACE_OUTER_BOUND('',#5637,.T.);
#3143=FACE_OUTER_BOUND('',#5638,.T.);
#3144=FACE_OUTER_BOUND('',#5639,.T.);
#3145=FACE_OUTER_BOUND('',#5640,.T.);
#3146=FACE_OUTER_BOUND('',#5641,.T.);
#3147=FACE_OUTER_BOUND('',#5642,.T.);
#3148=FACE_OUTER_BOUND('',#5643,.T.);
#3149=FACE_OUTER_BOUND('',#5644,.T.);
#3150=FACE_OUTER_BOUND('',#5645,.T.);
#3151=FACE_OUTER_BOUND('',#5646,.T.);
#3152=FACE_OUTER_BOUND('',#5647,.T.);
#3153=FACE_OUTER_BOUND('',#5648,.T.);
#3154=FACE_OUTER_BOUND('',#5649,.T.);
#3155=FACE_OUTER_BOUND('',#5650,.T.);
#3156=FACE_OUTER_BOUND('',#5651,.T.);
#3157=FACE_OUTER_BOUND('',#5652,.T.);
#3158=FACE_OUTER_BOUND('',#5653,.T.);
#3159=FACE_OUTER_BOUND('',#5654,.T.);
#3160=FACE_OUTER_BOUND('',#5655,.T.);
#3161=FACE_OUTER_BOUND('',#5656,.T.);
#3162=FACE_OUTER_BOUND('',#5657,.T.);
#3163=FACE_OUTER_BOUND('',#5658,.T.);
#3164=FACE_OUTER_BOUND('',#5659,.T.);
#3165=FACE_OUTER_BOUND('',#5660,.T.);
#3166=FACE_OUTER_BOUND('',#5661,.T.);
#3167=FACE_OUTER_BOUND('',#5662,.T.);
#3168=FACE_OUTER_BOUND('',#5663,.T.);
#3169=FACE_OUTER_BOUND('',#5664,.T.);
#3170=FACE_OUTER_BOUND('',#5665,.T.);
#3171=FACE_OUTER_BOUND('',#5666,.T.);
#3172=FACE_OUTER_BOUND('',#5667,.T.);
#3173=FACE_OUTER_BOUND('',#5668,.T.);
#3174=FACE_OUTER_BOUND('',#5669,.T.);
#3175=FACE_OUTER_BOUND('',#5670,.T.);
#3176=FACE_OUTER_BOUND('',#5671,.T.);
#3177=FACE_OUTER_BOUND('',#5672,.T.);
#3178=FACE_OUTER_BOUND('',#5673,.T.);
#3179=FACE_OUTER_BOUND('',#5674,.T.);
#3180=FACE_OUTER_BOUND('',#5675,.T.);
#3181=FACE_OUTER_BOUND('',#5676,.T.);
#3182=FACE_OUTER_BOUND('',#5677,.T.);
#3183=FACE_OUTER_BOUND('',#5678,.T.);
#3184=FACE_OUTER_BOUND('',#5679,.T.);
#3185=FACE_OUTER_BOUND('',#5680,.T.);
#3186=FACE_OUTER_BOUND('',#5681,.T.);
#3187=FACE_OUTER_BOUND('',#5682,.T.);
#3188=FACE_OUTER_BOUND('',#5683,.T.);
#3189=FACE_OUTER_BOUND('',#5684,.T.);
#3190=FACE_OUTER_BOUND('',#5685,.T.);
#3191=FACE_OUTER_BOUND('',#5686,.T.);
#3192=FACE_OUTER_BOUND('',#5687,.T.);
#3193=FACE_OUTER_BOUND('',#5688,.T.);
#3194=FACE_OUTER_BOUND('',#5689,.T.);
#3195=FACE_OUTER_BOUND('',#5690,.T.);
#3196=FACE_OUTER_BOUND('',#5691,.T.);
#3197=FACE_OUTER_BOUND('',#5692,.T.);
#3198=FACE_OUTER_BOUND('',#5693,.T.);
#3199=FACE_OUTER_BOUND('',#5694,.T.);
#3200=FACE_OUTER_BOUND('',#5695,.T.);
#3201=FACE_OUTER_BOUND('',#5696,.T.);
#3202=FACE_OUTER_BOUND('',#5697,.T.);
#3203=FACE_OUTER_BOUND('',#5698,.T.);
#3204=FACE_OUTER_BOUND('',#5699,.T.);
#3205=FACE_OUTER_BOUND('',#5700,.T.);
#3206=FACE_OUTER_BOUND('',#5701,.T.);
#3207=FACE_OUTER_BOUND('',#5702,.T.);
#3208=FACE_OUTER_BOUND('',#5703,.T.);
#3209=FACE_OUTER_BOUND('',#5704,.T.);
#3210=FACE_OUTER_BOUND('',#5705,.T.);
#3211=FACE_OUTER_BOUND('',#5706,.T.);
#3212=FACE_OUTER_BOUND('',#5707,.T.);
#3213=FACE_OUTER_BOUND('',#5708,.T.);
#3214=FACE_OUTER_BOUND('',#5709,.T.);
#3215=FACE_OUTER_BOUND('',#5710,.T.);
#3216=FACE_OUTER_BOUND('',#5711,.T.);
#3217=FACE_OUTER_BOUND('',#5712,.T.);
#3218=FACE_OUTER_BOUND('',#5713,.T.);
#3219=FACE_OUTER_BOUND('',#5714,.T.);
#3220=FACE_OUTER_BOUND('',#5715,.T.);
#3221=FACE_OUTER_BOUND('',#5716,.T.);
#3222=FACE_OUTER_BOUND('',#5717,.T.);
#3223=FACE_OUTER_BOUND('',#5718,.T.);
#3224=FACE_OUTER_BOUND('',#5719,.T.);
#3225=FACE_OUTER_BOUND('',#5720,.T.);
#3226=FACE_OUTER_BOUND('',#5721,.T.);
#3227=FACE_OUTER_BOUND('',#5722,.T.);
#3228=FACE_OUTER_BOUND('',#5723,.T.);
#3229=FACE_OUTER_BOUND('',#5724,.T.);
#3230=FACE_OUTER_BOUND('',#5725,.T.);
#3231=FACE_OUTER_BOUND('',#5726,.T.);
#3232=FACE_OUTER_BOUND('',#5727,.T.);
#3233=FACE_OUTER_BOUND('',#5728,.T.);
#3234=FACE_OUTER_BOUND('',#5729,.T.);
#3235=FACE_OUTER_BOUND('',#5730,.T.);
#3236=FACE_OUTER_BOUND('',#5731,.T.);
#3237=FACE_OUTER_BOUND('',#5732,.T.);
#3238=FACE_OUTER_BOUND('',#5733,.T.);
#3239=FACE_OUTER_BOUND('',#5734,.T.);
#3240=FACE_OUTER_BOUND('',#5735,.T.);
#3241=FACE_OUTER_BOUND('',#5736,.T.);
#3242=FACE_OUTER_BOUND('',#5737,.T.);
#3243=FACE_OUTER_BOUND('',#5738,.T.);
#3244=FACE_OUTER_BOUND('',#5739,.T.);
#3245=FACE_OUTER_BOUND('',#5740,.T.);
#3246=FACE_OUTER_BOUND('',#5741,.T.);
#3247=FACE_OUTER_BOUND('',#5742,.T.);
#3248=FACE_OUTER_BOUND('',#5743,.T.);
#3249=FACE_OUTER_BOUND('',#5744,.T.);
#3250=FACE_OUTER_BOUND('',#5745,.T.);
#3251=FACE_OUTER_BOUND('',#5746,.T.);
#3252=FACE_OUTER_BOUND('',#5747,.T.);
#3253=FACE_OUTER_BOUND('',#5748,.T.);
#3254=FACE_OUTER_BOUND('',#5749,.T.);
#3255=FACE_OUTER_BOUND('',#5750,.T.);
#3256=FACE_OUTER_BOUND('',#5751,.T.);
#3257=FACE_OUTER_BOUND('',#5752,.T.);
#3258=FACE_OUTER_BOUND('',#5753,.T.);
#3259=FACE_OUTER_BOUND('',#5754,.T.);
#3260=FACE_OUTER_BOUND('',#5755,.T.);
#3261=FACE_OUTER_BOUND('',#5756,.T.);
#3262=FACE_OUTER_BOUND('',#5757,.T.);
#3263=FACE_OUTER_BOUND('',#5758,.T.);
#3264=FACE_OUTER_BOUND('',#5759,.T.);
#3265=FACE_OUTER_BOUND('',#5760,.T.);
#3266=FACE_OUTER_BOUND('',#5761,.T.);
#3267=FACE_OUTER_BOUND('',#5762,.T.);
#3268=FACE_OUTER_BOUND('',#5763,.T.);
#3269=FACE_OUTER_BOUND('',#5764,.T.);
#3270=FACE_OUTER_BOUND('',#5765,.T.);
#3271=FACE_OUTER_BOUND('',#5766,.T.);
#3272=FACE_OUTER_BOUND('',#5767,.T.);
#3273=FACE_OUTER_BOUND('',#5768,.T.);
#3274=FACE_OUTER_BOUND('',#5769,.T.);
#3275=FACE_OUTER_BOUND('',#5770,.T.);
#3276=FACE_OUTER_BOUND('',#5771,.T.);
#3277=FACE_OUTER_BOUND('',#5772,.T.);
#3278=FACE_OUTER_BOUND('',#5773,.T.);
#3279=FACE_OUTER_BOUND('',#5774,.T.);
#3280=FACE_OUTER_BOUND('',#5775,.T.);
#3281=FACE_OUTER_BOUND('',#5776,.T.);
#3282=FACE_OUTER_BOUND('',#5777,.T.);
#3283=FACE_OUTER_BOUND('',#5778,.T.);
#3284=FACE_OUTER_BOUND('',#5779,.T.);
#3285=FACE_OUTER_BOUND('',#5780,.T.);
#3286=FACE_OUTER_BOUND('',#5781,.T.);
#3287=FACE_OUTER_BOUND('',#5782,.T.);
#3288=FACE_OUTER_BOUND('',#5783,.T.);
#3289=FACE_OUTER_BOUND('',#5784,.T.);
#3290=FACE_OUTER_BOUND('',#5785,.T.);
#3291=FACE_OUTER_BOUND('',#5786,.T.);
#3292=FACE_OUTER_BOUND('',#5787,.T.);
#3293=FACE_OUTER_BOUND('',#5788,.T.);
#3294=FACE_OUTER_BOUND('',#5789,.T.);
#3295=FACE_OUTER_BOUND('',#5790,.T.);
#3296=FACE_OUTER_BOUND('',#5791,.T.);
#3297=FACE_OUTER_BOUND('',#5792,.T.);
#3298=FACE_OUTER_BOUND('',#5793,.T.);
#3299=FACE_OUTER_BOUND('',#5794,.T.);
#3300=FACE_OUTER_BOUND('',#5795,.T.);
#3301=FACE_OUTER_BOUND('',#5796,.T.);
#3302=FACE_OUTER_BOUND('',#5797,.T.);
#3303=FACE_OUTER_BOUND('',#5798,.T.);
#3304=FACE_OUTER_BOUND('',#5799,.T.);
#3305=FACE_OUTER_BOUND('',#5800,.T.);
#3306=FACE_OUTER_BOUND('',#5801,.T.);
#3307=FACE_OUTER_BOUND('',#5802,.T.);
#3308=FACE_OUTER_BOUND('',#5803,.T.);
#3309=FACE_OUTER_BOUND('',#5804,.T.);
#3310=FACE_OUTER_BOUND('',#5805,.T.);
#3311=FACE_OUTER_BOUND('',#5806,.T.);
#3312=FACE_OUTER_BOUND('',#5807,.T.);
#3313=FACE_OUTER_BOUND('',#5808,.T.);
#3314=FACE_OUTER_BOUND('',#5809,.T.);
#3315=FACE_OUTER_BOUND('',#5810,.T.);
#3316=FACE_OUTER_BOUND('',#5811,.T.);
#3317=FACE_OUTER_BOUND('',#5812,.T.);
#3318=FACE_OUTER_BOUND('',#5813,.T.);
#3319=FACE_OUTER_BOUND('',#5814,.T.);
#3320=FACE_OUTER_BOUND('',#5815,.T.);
#3321=FACE_OUTER_BOUND('',#5816,.T.);
#3322=FACE_OUTER_BOUND('',#5817,.T.);
#3323=FACE_OUTER_BOUND('',#5818,.T.);
#3324=FACE_OUTER_BOUND('',#5819,.T.);
#3325=FACE_OUTER_BOUND('',#5820,.T.);
#3326=FACE_OUTER_BOUND('',#5821,.T.);
#3327=FACE_OUTER_BOUND('',#5822,.T.);
#3328=FACE_OUTER_BOUND('',#5823,.T.);
#3329=FACE_OUTER_BOUND('',#5824,.T.);
#3330=FACE_OUTER_BOUND('',#5825,.T.);
#3331=FACE_OUTER_BOUND('',#5826,.T.);
#3332=FACE_OUTER_BOUND('',#5827,.T.);
#3333=FACE_OUTER_BOUND('',#5828,.T.);
#3334=FACE_OUTER_BOUND('',#5829,.T.);
#3335=FACE_OUTER_BOUND('',#5830,.T.);
#3336=FACE_OUTER_BOUND('',#5831,.T.);
#3337=FACE_OUTER_BOUND('',#5832,.T.);
#3338=FACE_OUTER_BOUND('',#5833,.T.);
#3339=FACE_OUTER_BOUND('',#5834,.T.);
#3340=FACE_OUTER_BOUND('',#5835,.T.);
#3341=FACE_OUTER_BOUND('',#5836,.T.);
#3342=FACE_OUTER_BOUND('',#5837,.T.);
#3343=FACE_OUTER_BOUND('',#5838,.T.);
#3344=FACE_OUTER_BOUND('',#5839,.T.);
#3345=FACE_OUTER_BOUND('',#5840,.T.);
#3346=FACE_OUTER_BOUND('',#5841,.T.);
#3347=FACE_OUTER_BOUND('',#5842,.T.);
#3348=FACE_OUTER_BOUND('',#5843,.T.);
#3349=FACE_OUTER_BOUND('',#5844,.T.);
#3350=FACE_OUTER_BOUND('',#5845,.T.);
#3351=FACE_OUTER_BOUND('',#5846,.T.);
#3352=FACE_OUTER_BOUND('',#5847,.T.);
#3353=FACE_OUTER_BOUND('',#5848,.T.);
#3354=FACE_OUTER_BOUND('',#5849,.T.);
#3355=FACE_OUTER_BOUND('',#5850,.T.);
#3356=FACE_OUTER_BOUND('',#5851,.T.);
#3357=FACE_OUTER_BOUND('',#5852,.T.);
#3358=FACE_OUTER_BOUND('',#5853,.T.);
#3359=FACE_OUTER_BOUND('',#5854,.T.);
#3360=FACE_OUTER_BOUND('',#5855,.T.);
#3361=FACE_OUTER_BOUND('',#5856,.T.);
#3362=FACE_OUTER_BOUND('',#5857,.T.);
#3363=FACE_OUTER_BOUND('',#5858,.T.);
#3364=FACE_OUTER_BOUND('',#5859,.T.);
#3365=FACE_OUTER_BOUND('',#5860,.T.);
#3366=FACE_OUTER_BOUND('',#5861,.T.);
#3367=FACE_OUTER_BOUND('',#5862,.T.);
#3368=FACE_OUTER_BOUND('',#5863,.T.);
#3369=FACE_OUTER_BOUND('',#5864,.T.);
#3370=FACE_OUTER_BOUND('',#5865,.T.);
#3371=FACE_OUTER_BOUND('',#5866,.T.);
#3372=FACE_OUTER_BOUND('',#5867,.T.);
#3373=FACE_OUTER_BOUND('',#5868,.T.);
#3374=FACE_OUTER_BOUND('',#5869,.T.);
#3375=FACE_OUTER_BOUND('',#5870,.T.);
#3376=FACE_OUTER_BOUND('',#5871,.T.);
#3377=FACE_OUTER_BOUND('',#5872,.T.);
#3378=FACE_OUTER_BOUND('',#5873,.T.);
#3379=FACE_OUTER_BOUND('',#5874,.T.);
#3380=FACE_OUTER_BOUND('',#5875,.T.);
#3381=FACE_OUTER_BOUND('',#5876,.T.);
#3382=FACE_OUTER_BOUND('',#5877,.T.);
#3383=FACE_OUTER_BOUND('',#5878,.T.);
#3384=FACE_OUTER_BOUND('',#5879,.T.);
#3385=FACE_OUTER_BOUND('',#5880,.T.);
#3386=FACE_OUTER_BOUND('',#5881,.T.);
#3387=FACE_OUTER_BOUND('',#5882,.T.);
#3388=FACE_OUTER_BOUND('',#5883,.T.);
#3389=FACE_OUTER_BOUND('',#5884,.T.);
#3390=FACE_OUTER_BOUND('',#5885,.T.);
#3391=FACE_OUTER_BOUND('',#5886,.T.);
#3392=FACE_OUTER_BOUND('',#5887,.T.);
#3393=FACE_OUTER_BOUND('',#5888,.T.);
#3394=FACE_OUTER_BOUND('',#5889,.T.);
#3395=FACE_OUTER_BOUND('',#5890,.T.);
#3396=FACE_OUTER_BOUND('',#5891,.T.);
#3397=FACE_OUTER_BOUND('',#5892,.T.);
#3398=FACE_OUTER_BOUND('',#5893,.T.);
#3399=FACE_OUTER_BOUND('',#5894,.T.);
#3400=FACE_OUTER_BOUND('',#5895,.T.);
#3401=FACE_OUTER_BOUND('',#5896,.T.);
#3402=FACE_OUTER_BOUND('',#5897,.T.);
#3403=FACE_OUTER_BOUND('',#5898,.T.);
#3404=FACE_OUTER_BOUND('',#5899,.T.);
#3405=FACE_OUTER_BOUND('',#5900,.T.);
#3406=FACE_OUTER_BOUND('',#5901,.T.);
#3407=FACE_OUTER_BOUND('',#5902,.T.);
#3408=FACE_OUTER_BOUND('',#5903,.T.);
#3409=FACE_OUTER_BOUND('',#5904,.T.);
#3410=FACE_OUTER_BOUND('',#5905,.T.);
#3411=FACE_OUTER_BOUND('',#5906,.T.);
#3412=FACE_OUTER_BOUND('',#5907,.T.);
#3413=FACE_OUTER_BOUND('',#5908,.T.);
#3414=FACE_OUTER_BOUND('',#5909,.T.);
#3415=FACE_OUTER_BOUND('',#5910,.T.);
#3416=FACE_OUTER_BOUND('',#5911,.T.);
#3417=FACE_OUTER_BOUND('',#5912,.T.);
#3418=FACE_OUTER_BOUND('',#5913,.T.);
#3419=FACE_OUTER_BOUND('',#5914,.T.);
#3420=FACE_OUTER_BOUND('',#5915,.T.);
#3421=FACE_OUTER_BOUND('',#5916,.T.);
#3422=FACE_OUTER_BOUND('',#5917,.T.);
#3423=FACE_OUTER_BOUND('',#5918,.T.);
#3424=FACE_OUTER_BOUND('',#5919,.T.);
#3425=FACE_OUTER_BOUND('',#5920,.T.);
#3426=FACE_OUTER_BOUND('',#5921,.T.);
#3427=FACE_OUTER_BOUND('',#5922,.T.);
#3428=FACE_OUTER_BOUND('',#5923,.T.);
#3429=FACE_OUTER_BOUND('',#5924,.T.);
#3430=FACE_OUTER_BOUND('',#5925,.T.);
#3431=FACE_OUTER_BOUND('',#5926,.T.);
#3432=FACE_OUTER_BOUND('',#5927,.T.);
#3433=FACE_OUTER_BOUND('',#5928,.T.);
#3434=FACE_OUTER_BOUND('',#5929,.T.);
#3435=FACE_OUTER_BOUND('',#5930,.T.);
#3436=FACE_OUTER_BOUND('',#5931,.T.);
#3437=FACE_OUTER_BOUND('',#5932,.T.);
#3438=FACE_OUTER_BOUND('',#5933,.T.);
#3439=FACE_OUTER_BOUND('',#5934,.T.);
#3440=FACE_OUTER_BOUND('',#5935,.T.);
#3441=FACE_OUTER_BOUND('',#5936,.T.);
#3442=FACE_OUTER_BOUND('',#5937,.T.);
#3443=FACE_OUTER_BOUND('',#5938,.T.);
#3444=FACE_OUTER_BOUND('',#5939,.T.);
#3445=FACE_OUTER_BOUND('',#5940,.T.);
#3446=FACE_OUTER_BOUND('',#5941,.T.);
#3447=FACE_OUTER_BOUND('',#5942,.T.);
#3448=FACE_OUTER_BOUND('',#5943,.T.);
#3449=FACE_OUTER_BOUND('',#5944,.T.);
#3450=FACE_OUTER_BOUND('',#5945,.T.);
#3451=FACE_OUTER_BOUND('',#5946,.T.);
#3452=FACE_OUTER_BOUND('',#5947,.T.);
#3453=FACE_OUTER_BOUND('',#5948,.T.);
#3454=FACE_OUTER_BOUND('',#5949,.T.);
#3455=FACE_OUTER_BOUND('',#5950,.T.);
#3456=FACE_OUTER_BOUND('',#5951,.T.);
#3457=FACE_OUTER_BOUND('',#5952,.T.);
#3458=FACE_OUTER_BOUND('',#5953,.T.);
#3459=FACE_OUTER_BOUND('',#5954,.T.);
#3460=FACE_OUTER_BOUND('',#5955,.T.);
#3461=FACE_OUTER_BOUND('',#5956,.T.);
#3462=FACE_OUTER_BOUND('',#5957,.T.);
#3463=FACE_OUTER_BOUND('',#5958,.T.);
#3464=FACE_OUTER_BOUND('',#5959,.T.);
#3465=FACE_OUTER_BOUND('',#5960,.T.);
#3466=FACE_OUTER_BOUND('',#5961,.T.);
#3467=FACE_OUTER_BOUND('',#5962,.T.);
#3468=FACE_OUTER_BOUND('',#5963,.T.);
#3469=FACE_OUTER_BOUND('',#5964,.T.);
#3470=FACE_OUTER_BOUND('',#5965,.T.);
#3471=FACE_OUTER_BOUND('',#5966,.T.);
#3472=FACE_OUTER_BOUND('',#5967,.T.);
#3473=FACE_OUTER_BOUND('',#5968,.T.);
#3474=FACE_OUTER_BOUND('',#5969,.T.);
#3475=FACE_OUTER_BOUND('',#5970,.T.);
#3476=FACE_OUTER_BOUND('',#5971,.T.);
#3477=FACE_OUTER_BOUND('',#5972,.T.);
#3478=FACE_OUTER_BOUND('',#5973,.T.);
#3479=FACE_OUTER_BOUND('',#5974,.T.);
#3480=FACE_OUTER_BOUND('',#5975,.T.);
#3481=FACE_OUTER_BOUND('',#5976,.T.);
#3482=FACE_OUTER_BOUND('',#5977,.T.);
#3483=FACE_OUTER_BOUND('',#5978,.T.);
#3484=FACE_OUTER_BOUND('',#5979,.T.);
#3485=FACE_OUTER_BOUND('',#5980,.T.);
#3486=FACE_OUTER_BOUND('',#5981,.T.);
#3487=FACE_OUTER_BOUND('',#5982,.T.);
#3488=FACE_OUTER_BOUND('',#5983,.T.);
#3489=FACE_OUTER_BOUND('',#5984,.T.);
#3490=FACE_OUTER_BOUND('',#5985,.T.);
#3491=FACE_OUTER_BOUND('',#5986,.T.);
#3492=FACE_OUTER_BOUND('',#5987,.T.);
#3493=FACE_OUTER_BOUND('',#5988,.T.);
#3494=FACE_OUTER_BOUND('',#5989,.T.);
#3495=FACE_OUTER_BOUND('',#5990,.T.);
#3496=FACE_OUTER_BOUND('',#5991,.T.);
#3497=FACE_OUTER_BOUND('',#5992,.T.);
#3498=FACE_OUTER_BOUND('',#5993,.T.);
#3499=FACE_OUTER_BOUND('',#5994,.T.);
#3500=FACE_OUTER_BOUND('',#5995,.T.);
#3501=FACE_OUTER_BOUND('',#5996,.T.);
#3502=FACE_OUTER_BOUND('',#5997,.T.);
#3503=FACE_OUTER_BOUND('',#5998,.T.);
#3504=FACE_OUTER_BOUND('',#5999,.T.);
#3505=FACE_OUTER_BOUND('',#6000,.T.);
#3506=FACE_OUTER_BOUND('',#6001,.T.);
#3507=FACE_OUTER_BOUND('',#6002,.T.);
#3508=FACE_OUTER_BOUND('',#6003,.T.);
#3509=FACE_OUTER_BOUND('',#6004,.T.);
#3510=FACE_OUTER_BOUND('',#6005,.T.);
#3511=FACE_OUTER_BOUND('',#6006,.T.);
#3512=FACE_OUTER_BOUND('',#6007,.T.);
#3513=FACE_OUTER_BOUND('',#6008,.T.);
#3514=FACE_OUTER_BOUND('',#6009,.T.);
#3515=FACE_OUTER_BOUND('',#6010,.T.);
#3516=FACE_OUTER_BOUND('',#6011,.T.);
#3517=FACE_OUTER_BOUND('',#6012,.T.);
#3518=FACE_OUTER_BOUND('',#6013,.T.);
#3519=FACE_OUTER_BOUND('',#6014,.T.);
#3520=FACE_OUTER_BOUND('',#6015,.T.);
#3521=FACE_OUTER_BOUND('',#6016,.T.);
#3522=FACE_OUTER_BOUND('',#6017,.T.);
#3523=FACE_OUTER_BOUND('',#6018,.T.);
#3524=FACE_OUTER_BOUND('',#6019,.T.);
#3525=FACE_OUTER_BOUND('',#6020,.T.);
#3526=FACE_OUTER_BOUND('',#6021,.T.);
#3527=FACE_OUTER_BOUND('',#6022,.T.);
#3528=FACE_OUTER_BOUND('',#6023,.T.);
#3529=FACE_OUTER_BOUND('',#6024,.T.);
#3530=FACE_OUTER_BOUND('',#6025,.T.);
#3531=FACE_OUTER_BOUND('',#6026,.T.);
#3532=FACE_OUTER_BOUND('',#6027,.T.);
#3533=FACE_OUTER_BOUND('',#6028,.T.);
#3534=FACE_OUTER_BOUND('',#6029,.T.);
#3535=FACE_OUTER_BOUND('',#6030,.T.);
#3536=FACE_OUTER_BOUND('',#6031,.T.);
#3537=FACE_OUTER_BOUND('',#6032,.T.);
#3538=FACE_OUTER_BOUND('',#6033,.T.);
#3539=FACE_OUTER_BOUND('',#6034,.T.);
#3540=FACE_OUTER_BOUND('',#6035,.T.);
#3541=FACE_OUTER_BOUND('',#6036,.T.);
#3542=FACE_OUTER_BOUND('',#6037,.T.);
#3543=FACE_OUTER_BOUND('',#6038,.T.);
#3544=FACE_OUTER_BOUND('',#6039,.T.);
#3545=FACE_OUTER_BOUND('',#6040,.T.);
#3546=FACE_OUTER_BOUND('',#6041,.T.);
#3547=FACE_OUTER_BOUND('',#6042,.T.);
#3548=FACE_OUTER_BOUND('',#6043,.T.);
#3549=FACE_OUTER_BOUND('',#6044,.T.);
#3550=FACE_OUTER_BOUND('',#6045,.T.);
#3551=FACE_OUTER_BOUND('',#6046,.T.);
#3552=FACE_OUTER_BOUND('',#6047,.T.);
#3553=FACE_OUTER_BOUND('',#6048,.T.);
#3554=FACE_OUTER_BOUND('',#6049,.T.);
#3555=FACE_OUTER_BOUND('',#6050,.T.);
#3556=FACE_OUTER_BOUND('',#6051,.T.);
#3557=FACE_OUTER_BOUND('',#6052,.T.);
#3558=FACE_OUTER_BOUND('',#6053,.T.);
#3559=FACE_OUTER_BOUND('',#6054,.T.);
#3560=FACE_OUTER_BOUND('',#6055,.T.);
#3561=FACE_OUTER_BOUND('',#6056,.T.);
#3562=FACE_OUTER_BOUND('',#6057,.T.);
#3563=FACE_OUTER_BOUND('',#6058,.T.);
#3564=FACE_OUTER_BOUND('',#6059,.T.);
#3565=FACE_OUTER_BOUND('',#6060,.T.);
#3566=FACE_OUTER_BOUND('',#6061,.T.);
#3567=FACE_OUTER_BOUND('',#6062,.T.);
#3568=FACE_OUTER_BOUND('',#6063,.T.);
#3569=FACE_OUTER_BOUND('',#6064,.T.);
#3570=FACE_OUTER_BOUND('',#6065,.T.);
#3571=FACE_OUTER_BOUND('',#6066,.T.);
#3572=FACE_OUTER_BOUND('',#6067,.T.);
#3573=FACE_OUTER_BOUND('',#6068,.T.);
#3574=FACE_OUTER_BOUND('',#6069,.T.);
#3575=FACE_OUTER_BOUND('',#6070,.T.);
#3576=FACE_OUTER_BOUND('',#6071,.T.);
#3577=FACE_OUTER_BOUND('',#6072,.T.);
#3578=FACE_OUTER_BOUND('',#6073,.T.);
#3579=FACE_OUTER_BOUND('',#6074,.T.);
#3580=FACE_OUTER_BOUND('',#6075,.T.);
#3581=FACE_OUTER_BOUND('',#6076,.T.);
#3582=FACE_OUTER_BOUND('',#6077,.T.);
#3583=FACE_OUTER_BOUND('',#6078,.T.);
#3584=FACE_OUTER_BOUND('',#6079,.T.);
#3585=FACE_OUTER_BOUND('',#6080,.T.);
#3586=FACE_OUTER_BOUND('',#6081,.T.);
#3587=FACE_OUTER_BOUND('',#6082,.T.);
#3588=FACE_OUTER_BOUND('',#6083,.T.);
#3589=FACE_OUTER_BOUND('',#6084,.T.);
#3590=FACE_OUTER_BOUND('',#6085,.T.);
#3591=FACE_OUTER_BOUND('',#6086,.T.);
#3592=FACE_OUTER_BOUND('',#6087,.T.);
#3593=FACE_OUTER_BOUND('',#6088,.T.);
#3594=FACE_OUTER_BOUND('',#6089,.T.);
#3595=FACE_OUTER_BOUND('',#6090,.T.);
#3596=FACE_OUTER_BOUND('',#6091,.T.);
#3597=FACE_OUTER_BOUND('',#6092,.T.);
#3598=FACE_OUTER_BOUND('',#6093,.T.);
#3599=FACE_OUTER_BOUND('',#6094,.T.);
#3600=FACE_OUTER_BOUND('',#6095,.T.);
#3601=FACE_OUTER_BOUND('',#6096,.T.);
#3602=FACE_OUTER_BOUND('',#6097,.T.);
#3603=FACE_OUTER_BOUND('',#6098,.T.);
#3604=FACE_OUTER_BOUND('',#6099,.T.);
#3605=FACE_OUTER_BOUND('',#6100,.T.);
#3606=FACE_OUTER_BOUND('',#6101,.T.);
#3607=FACE_OUTER_BOUND('',#6102,.T.);
#3608=FACE_OUTER_BOUND('',#6103,.T.);
#3609=FACE_OUTER_BOUND('',#6104,.T.);
#3610=FACE_OUTER_BOUND('',#6105,.T.);
#3611=FACE_OUTER_BOUND('',#6106,.T.);
#3612=FACE_OUTER_BOUND('',#6107,.T.);
#3613=FACE_OUTER_BOUND('',#6108,.T.);
#3614=FACE_OUTER_BOUND('',#6109,.T.);
#3615=FACE_OUTER_BOUND('',#6110,.T.);
#3616=FACE_OUTER_BOUND('',#6111,.T.);
#3617=FACE_OUTER_BOUND('',#6112,.T.);
#3618=FACE_OUTER_BOUND('',#6113,.T.);
#3619=FACE_OUTER_BOUND('',#6114,.T.);
#3620=FACE_OUTER_BOUND('',#6115,.T.);
#3621=FACE_OUTER_BOUND('',#6116,.T.);
#3622=FACE_OUTER_BOUND('',#6117,.T.);
#3623=FACE_OUTER_BOUND('',#6118,.T.);
#3624=FACE_OUTER_BOUND('',#6119,.T.);
#3625=FACE_OUTER_BOUND('',#6120,.T.);
#3626=FACE_OUTER_BOUND('',#6121,.T.);
#3627=FACE_OUTER_BOUND('',#6122,.T.);
#3628=FACE_OUTER_BOUND('',#6123,.T.);
#3629=FACE_OUTER_BOUND('',#6124,.T.);
#3630=FACE_OUTER_BOUND('',#6125,.T.);
#3631=FACE_OUTER_BOUND('',#6126,.T.);
#3632=FACE_OUTER_BOUND('',#6127,.T.);
#3633=FACE_OUTER_BOUND('',#6128,.T.);
#3634=FACE_OUTER_BOUND('',#6129,.T.);
#3635=FACE_OUTER_BOUND('',#6130,.T.);
#3636=FACE_OUTER_BOUND('',#6131,.T.);
#3637=FACE_OUTER_BOUND('',#6132,.T.);
#3638=FACE_OUTER_BOUND('',#6133,.T.);
#3639=FACE_OUTER_BOUND('',#6134,.T.);
#3640=FACE_OUTER_BOUND('',#6135,.T.);
#3641=FACE_OUTER_BOUND('',#6136,.T.);
#3642=FACE_OUTER_BOUND('',#6137,.T.);
#3643=FACE_OUTER_BOUND('',#6138,.T.);
#3644=FACE_OUTER_BOUND('',#6139,.T.);
#3645=FACE_OUTER_BOUND('',#6140,.T.);
#3646=FACE_OUTER_BOUND('',#6141,.T.);
#3647=FACE_OUTER_BOUND('',#6142,.T.);
#3648=FACE_OUTER_BOUND('',#6143,.T.);
#3649=FACE_OUTER_BOUND('',#6144,.T.);
#3650=FACE_OUTER_BOUND('',#6145,.T.);
#3651=FACE_OUTER_BOUND('',#6146,.T.);
#3652=FACE_OUTER_BOUND('',#6147,.T.);
#3653=FACE_OUTER_BOUND('',#6148,.T.);
#3654=FACE_OUTER_BOUND('',#6149,.T.);
#3655=FACE_OUTER_BOUND('',#6150,.T.);
#3656=FACE_OUTER_BOUND('',#6151,.T.);
#3657=FACE_OUTER_BOUND('',#6152,.T.);
#3658=FACE_OUTER_BOUND('',#6153,.T.);
#3659=FACE_OUTER_BOUND('',#6154,.T.);
#3660=FACE_OUTER_BOUND('',#6155,.T.);
#3661=FACE_OUTER_BOUND('',#6156,.T.);
#3662=FACE_OUTER_BOUND('',#6157,.T.);
#3663=FACE_OUTER_BOUND('',#6158,.T.);
#3664=FACE_OUTER_BOUND('',#6159,.T.);
#3665=FACE_OUTER_BOUND('',#6160,.T.);
#3666=FACE_OUTER_BOUND('',#6161,.T.);
#3667=FACE_OUTER_BOUND('',#6162,.T.);
#3668=FACE_OUTER_BOUND('',#6163,.T.);
#3669=FACE_OUTER_BOUND('',#6164,.T.);
#3670=FACE_OUTER_BOUND('',#6165,.T.);
#3671=FACE_OUTER_BOUND('',#6166,.T.);
#3672=FACE_OUTER_BOUND('',#6167,.T.);
#3673=FACE_OUTER_BOUND('',#6168,.T.);
#3674=FACE_OUTER_BOUND('',#6169,.T.);
#3675=FACE_OUTER_BOUND('',#6170,.T.);
#3676=FACE_OUTER_BOUND('',#6171,.T.);
#3677=FACE_OUTER_BOUND('',#6172,.T.);
#3678=FACE_OUTER_BOUND('',#6173,.T.);
#3679=FACE_OUTER_BOUND('',#6174,.T.);
#3680=FACE_OUTER_BOUND('',#6175,.T.);
#3681=FACE_OUTER_BOUND('',#6176,.T.);
#3682=FACE_OUTER_BOUND('',#6177,.T.);
#3683=FACE_OUTER_BOUND('',#6178,.T.);
#3684=FACE_OUTER_BOUND('',#6179,.T.);
#3685=FACE_OUTER_BOUND('',#6180,.T.);
#3686=FACE_OUTER_BOUND('',#6181,.T.);
#3687=FACE_OUTER_BOUND('',#6182,.T.);
#3688=FACE_OUTER_BOUND('',#6183,.T.);
#3689=FACE_OUTER_BOUND('',#6184,.T.);
#3690=FACE_OUTER_BOUND('',#6185,.T.);
#3691=FACE_OUTER_BOUND('',#6186,.T.);
#3692=FACE_OUTER_BOUND('',#6187,.T.);
#3693=FACE_OUTER_BOUND('',#6188,.T.);
#3694=FACE_OUTER_BOUND('',#6189,.T.);
#3695=FACE_OUTER_BOUND('',#6190,.T.);
#3696=FACE_OUTER_BOUND('',#6191,.T.);
#3697=FACE_OUTER_BOUND('',#6192,.T.);
#3698=FACE_OUTER_BOUND('',#6193,.T.);
#3699=FACE_OUTER_BOUND('',#6194,.T.);
#3700=FACE_OUTER_BOUND('',#6195,.T.);
#3701=FACE_OUTER_BOUND('',#6196,.T.);
#3702=FACE_OUTER_BOUND('',#6197,.T.);
#3703=FACE_OUTER_BOUND('',#6198,.T.);
#3704=FACE_OUTER_BOUND('',#6199,.T.);
#3705=FACE_OUTER_BOUND('',#6200,.T.);
#3706=FACE_OUTER_BOUND('',#6201,.T.);
#3707=FACE_OUTER_BOUND('',#6202,.T.);
#3708=FACE_OUTER_BOUND('',#6203,.T.);
#3709=FACE_OUTER_BOUND('',#6204,.T.);
#3710=FACE_OUTER_BOUND('',#6205,.T.);
#3711=FACE_OUTER_BOUND('',#6206,.T.);
#3712=FACE_OUTER_BOUND('',#6207,.T.);
#3713=FACE_OUTER_BOUND('',#6208,.T.);
#3714=FACE_OUTER_BOUND('',#6209,.T.);
#3715=FACE_OUTER_BOUND('',#6210,.T.);
#3716=FACE_OUTER_BOUND('',#6211,.T.);
#3717=FACE_OUTER_BOUND('',#6212,.T.);
#3718=FACE_OUTER_BOUND('',#6213,.T.);
#3719=FACE_OUTER_BOUND('',#6214,.T.);
#3720=FACE_OUTER_BOUND('',#6215,.T.);
#3721=FACE_OUTER_BOUND('',#6216,.T.);
#3722=FACE_OUTER_BOUND('',#6217,.T.);
#3723=FACE_OUTER_BOUND('',#6218,.T.);
#3724=FACE_OUTER_BOUND('',#6219,.T.);
#3725=FACE_OUTER_BOUND('',#6220,.T.);
#3726=FACE_OUTER_BOUND('',#6221,.T.);
#3727=FACE_OUTER_BOUND('',#6222,.T.);
#3728=FACE_OUTER_BOUND('',#6223,.T.);
#3729=FACE_OUTER_BOUND('',#6224,.T.);
#3730=FACE_OUTER_BOUND('',#6225,.T.);
#3731=FACE_OUTER_BOUND('',#6226,.T.);
#3732=FACE_OUTER_BOUND('',#6227,.T.);
#3733=FACE_OUTER_BOUND('',#6228,.T.);
#3734=FACE_OUTER_BOUND('',#6229,.T.);
#3735=FACE_OUTER_BOUND('',#6230,.T.);
#3736=FACE_OUTER_BOUND('',#6231,.T.);
#3737=FACE_OUTER_BOUND('',#6232,.T.);
#3738=FACE_OUTER_BOUND('',#6233,.T.);
#3739=FACE_OUTER_BOUND('',#6234,.T.);
#3740=FACE_OUTER_BOUND('',#6235,.T.);
#3741=FACE_OUTER_BOUND('',#6236,.T.);
#3742=FACE_OUTER_BOUND('',#6237,.T.);
#3743=FACE_OUTER_BOUND('',#6238,.T.);
#3744=FACE_OUTER_BOUND('',#6239,.T.);
#3745=FACE_OUTER_BOUND('',#6240,.T.);
#3746=FACE_OUTER_BOUND('',#6241,.T.);
#3747=FACE_OUTER_BOUND('',#6242,.T.);
#3748=FACE_OUTER_BOUND('',#6243,.T.);
#3749=FACE_OUTER_BOUND('',#6244,.T.);
#3750=FACE_OUTER_BOUND('',#6245,.T.);
#3751=FACE_OUTER_BOUND('',#6246,.T.);
#3752=FACE_OUTER_BOUND('',#6247,.T.);
#3753=FACE_OUTER_BOUND('',#6248,.T.);
#3754=FACE_OUTER_BOUND('',#6249,.T.);
#3755=FACE_OUTER_BOUND('',#6250,.T.);
#3756=FACE_OUTER_BOUND('',#6251,.T.);
#3757=FACE_OUTER_BOUND('',#6252,.T.);
#3758=FACE_OUTER_BOUND('',#6253,.T.);
#3759=FACE_OUTER_BOUND('',#6254,.T.);
#3760=FACE_OUTER_BOUND('',#6255,.T.);
#3761=FACE_OUTER_BOUND('',#6256,.T.);
#3762=FACE_OUTER_BOUND('',#6257,.T.);
#3763=FACE_OUTER_BOUND('',#6258,.T.);
#3764=FACE_OUTER_BOUND('',#6259,.T.);
#3765=FACE_OUTER_BOUND('',#6260,.T.);
#3766=FACE_OUTER_BOUND('',#6261,.T.);
#3767=FACE_OUTER_BOUND('',#6262,.T.);
#3768=FACE_OUTER_BOUND('',#6263,.T.);
#3769=FACE_OUTER_BOUND('',#6264,.T.);
#3770=FACE_OUTER_BOUND('',#6265,.T.);
#3771=FACE_OUTER_BOUND('',#6266,.T.);
#3772=FACE_OUTER_BOUND('',#6267,.T.);
#3773=FACE_OUTER_BOUND('',#6268,.T.);
#3774=FACE_OUTER_BOUND('',#6269,.T.);
#3775=FACE_OUTER_BOUND('',#6270,.T.);
#3776=FACE_OUTER_BOUND('',#6271,.T.);
#3777=FACE_OUTER_BOUND('',#6272,.T.);
#3778=FACE_OUTER_BOUND('',#6273,.T.);
#3779=FACE_OUTER_BOUND('',#6274,.T.);
#3780=FACE_OUTER_BOUND('',#6275,.T.);
#3781=FACE_OUTER_BOUND('',#6276,.T.);
#3782=FACE_OUTER_BOUND('',#6277,.T.);
#3783=FACE_OUTER_BOUND('',#6278,.T.);
#3784=FACE_OUTER_BOUND('',#6279,.T.);
#3785=FACE_OUTER_BOUND('',#6280,.T.);
#3786=FACE_OUTER_BOUND('',#6281,.T.);
#3787=FACE_OUTER_BOUND('',#6282,.T.);
#3788=FACE_OUTER_BOUND('',#6283,.T.);
#3789=FACE_OUTER_BOUND('',#6284,.T.);
#3790=FACE_OUTER_BOUND('',#6285,.T.);
#3791=FACE_OUTER_BOUND('',#6286,.T.);
#3792=FACE_OUTER_BOUND('',#6287,.T.);
#3793=FACE_OUTER_BOUND('',#6288,.T.);
#3794=FACE_OUTER_BOUND('',#6289,.T.);
#3795=FACE_OUTER_BOUND('',#6290,.T.);
#3796=FACE_OUTER_BOUND('',#6291,.T.);
#3797=FACE_OUTER_BOUND('',#6292,.T.);
#3798=FACE_OUTER_BOUND('',#6293,.T.);
#3799=FACE_OUTER_BOUND('',#6294,.T.);
#3800=FACE_OUTER_BOUND('',#6295,.T.);
#3801=FACE_OUTER_BOUND('',#6296,.T.);
#3802=FACE_OUTER_BOUND('',#6297,.T.);
#3803=FACE_OUTER_BOUND('',#6298,.T.);
#3804=FACE_OUTER_BOUND('',#6299,.T.);
#3805=FACE_OUTER_BOUND('',#6300,.T.);
#3806=FACE_OUTER_BOUND('',#6301,.T.);
#3807=FACE_OUTER_BOUND('',#6302,.T.);
#3808=FACE_OUTER_BOUND('',#6303,.T.);
#3809=FACE_OUTER_BOUND('',#6304,.T.);
#3810=FACE_OUTER_BOUND('',#6305,.T.);
#3811=FACE_OUTER_BOUND('',#6306,.T.);
#3812=FACE_OUTER_BOUND('',#6307,.T.);
#3813=FACE_OUTER_BOUND('',#6308,.T.);
#3814=FACE_OUTER_BOUND('',#6309,.T.);
#3815=FACE_OUTER_BOUND('',#6310,.T.);
#3816=FACE_OUTER_BOUND('',#6311,.T.);
#3817=FACE_OUTER_BOUND('',#6312,.T.);
#3818=FACE_OUTER_BOUND('',#6313,.T.);
#3819=FACE_OUTER_BOUND('',#6314,.T.);
#3820=FACE_OUTER_BOUND('',#6315,.T.);
#3821=FACE_OUTER_BOUND('',#6316,.T.);
#3822=FACE_OUTER_BOUND('',#6317,.T.);
#3823=FACE_OUTER_BOUND('',#6318,.T.);
#3824=FACE_OUTER_BOUND('',#6319,.T.);
#3825=FACE_OUTER_BOUND('',#6320,.T.);
#3826=FACE_OUTER_BOUND('',#6321,.T.);
#3827=FACE_OUTER_BOUND('',#6322,.T.);
#3828=FACE_OUTER_BOUND('',#6323,.T.);
#3829=FACE_OUTER_BOUND('',#6324,.T.);
#3830=FACE_OUTER_BOUND('',#6325,.T.);
#3831=FACE_OUTER_BOUND('',#6326,.T.);
#3832=FACE_OUTER_BOUND('',#6327,.T.);
#3833=FACE_OUTER_BOUND('',#6328,.T.);
#3834=FACE_OUTER_BOUND('',#6329,.T.);
#3835=FACE_OUTER_BOUND('',#6330,.T.);
#3836=FACE_OUTER_BOUND('',#6331,.T.);
#3837=FACE_OUTER_BOUND('',#6332,.T.);
#3838=FACE_OUTER_BOUND('',#6333,.T.);
#3839=FACE_OUTER_BOUND('',#6334,.T.);
#3840=FACE_OUTER_BOUND('',#6335,.T.);
#3841=FACE_OUTER_BOUND('',#6336,.T.);
#3842=FACE_OUTER_BOUND('',#6337,.T.);
#3843=FACE_OUTER_BOUND('',#6338,.T.);
#3844=FACE_OUTER_BOUND('',#6339,.T.);
#3845=FACE_OUTER_BOUND('',#6340,.T.);
#3846=FACE_OUTER_BOUND('',#6341,.T.);
#3847=FACE_OUTER_BOUND('',#6342,.T.);
#3848=FACE_OUTER_BOUND('',#6343,.T.);
#3849=FACE_OUTER_BOUND('',#6344,.T.);
#3850=FACE_OUTER_BOUND('',#6345,.T.);
#3851=FACE_OUTER_BOUND('',#6346,.T.);
#3852=FACE_OUTER_BOUND('',#6347,.T.);
#3853=FACE_OUTER_BOUND('',#6348,.T.);
#3854=FACE_OUTER_BOUND('',#6349,.T.);
#3855=FACE_OUTER_BOUND('',#6350,.T.);
#3856=FACE_OUTER_BOUND('',#6351,.T.);
#3857=FACE_OUTER_BOUND('',#6352,.T.);
#3858=FACE_OUTER_BOUND('',#6353,.T.);
#3859=FACE_OUTER_BOUND('',#6354,.T.);
#3860=FACE_OUTER_BOUND('',#6355,.T.);
#3861=FACE_OUTER_BOUND('',#6356,.T.);
#3862=FACE_OUTER_BOUND('',#6357,.T.);
#3863=FACE_OUTER_BOUND('',#6358,.T.);
#3864=FACE_OUTER_BOUND('',#6359,.T.);
#3865=FACE_OUTER_BOUND('',#6360,.T.);
#3866=FACE_OUTER_BOUND('',#6361,.T.);
#3867=FACE_OUTER_BOUND('',#6362,.T.);
#3868=FACE_OUTER_BOUND('',#6363,.T.);
#3869=FACE_OUTER_BOUND('',#6364,.T.);
#3870=FACE_OUTER_BOUND('',#6365,.T.);
#3871=FACE_OUTER_BOUND('',#6366,.T.);
#3872=FACE_OUTER_BOUND('',#6367,.T.);
#3873=FACE_OUTER_BOUND('',#6368,.T.);
#3874=FACE_OUTER_BOUND('',#6369,.T.);
#3875=FACE_OUTER_BOUND('',#6370,.T.);
#3876=FACE_OUTER_BOUND('',#6371,.T.);
#3877=FACE_OUTER_BOUND('',#6372,.T.);
#3878=FACE_OUTER_BOUND('',#6373,.T.);
#3879=FACE_OUTER_BOUND('',#6374,.T.);
#3880=FACE_OUTER_BOUND('',#6375,.T.);
#3881=FACE_OUTER_BOUND('',#6376,.T.);
#3882=FACE_OUTER_BOUND('',#6377,.T.);
#3883=FACE_OUTER_BOUND('',#6378,.T.);
#3884=FACE_OUTER_BOUND('',#6379,.T.);
#3885=FACE_OUTER_BOUND('',#6380,.T.);
#3886=FACE_OUTER_BOUND('',#6381,.T.);
#3887=FACE_OUTER_BOUND('',#6382,.T.);
#3888=FACE_OUTER_BOUND('',#6383,.T.);
#3889=FACE_OUTER_BOUND('',#6384,.T.);
#3890=FACE_OUTER_BOUND('',#6385,.T.);
#3891=FACE_OUTER_BOUND('',#6386,.T.);
#3892=FACE_OUTER_BOUND('',#6387,.T.);
#3893=FACE_OUTER_BOUND('',#6388,.T.);
#3894=FACE_OUTER_BOUND('',#6389,.T.);
#3895=FACE_OUTER_BOUND('',#6390,.T.);
#3896=FACE_OUTER_BOUND('',#6391,.T.);
#3897=FACE_OUTER_BOUND('',#6392,.T.);
#3898=FACE_OUTER_BOUND('',#6393,.T.);
#3899=FACE_OUTER_BOUND('',#6394,.T.);
#3900=FACE_OUTER_BOUND('',#6395,.T.);
#3901=FACE_OUTER_BOUND('',#6396,.T.);
#3902=FACE_OUTER_BOUND('',#6397,.T.);
#3903=FACE_OUTER_BOUND('',#6398,.T.);
#3904=FACE_OUTER_BOUND('',#6399,.T.);
#3905=FACE_OUTER_BOUND('',#6400,.T.);
#3906=FACE_OUTER_BOUND('',#6401,.T.);
#3907=FACE_OUTER_BOUND('',#6402,.T.);
#3908=FACE_OUTER_BOUND('',#6403,.T.);
#3909=FACE_OUTER_BOUND('',#6404,.T.);
#3910=FACE_OUTER_BOUND('',#6405,.T.);
#3911=FACE_OUTER_BOUND('',#6406,.T.);
#3912=FACE_OUTER_BOUND('',#6407,.T.);
#3913=FACE_OUTER_BOUND('',#6408,.T.);
#3914=FACE_OUTER_BOUND('',#6409,.T.);
#3915=FACE_OUTER_BOUND('',#6410,.T.);
#3916=FACE_OUTER_BOUND('',#6411,.T.);
#3917=FACE_OUTER_BOUND('',#6412,.T.);
#3918=FACE_OUTER_BOUND('',#6413,.T.);
#3919=FACE_OUTER_BOUND('',#6414,.T.);
#3920=FACE_OUTER_BOUND('',#6415,.T.);
#3921=FACE_OUTER_BOUND('',#6416,.T.);
#3922=FACE_OUTER_BOUND('',#6417,.T.);
#3923=FACE_OUTER_BOUND('',#6418,.T.);
#3924=FACE_OUTER_BOUND('',#6419,.T.);
#3925=FACE_OUTER_BOUND('',#6420,.T.);
#3926=FACE_OUTER_BOUND('',#6421,.T.);
#3927=FACE_OUTER_BOUND('',#6422,.T.);
#3928=FACE_OUTER_BOUND('',#6423,.T.);
#3929=FACE_OUTER_BOUND('',#6424,.T.);
#3930=FACE_OUTER_BOUND('',#6425,.T.);
#3931=FACE_OUTER_BOUND('',#6426,.T.);
#3932=FACE_OUTER_BOUND('',#6427,.T.);
#3933=FACE_OUTER_BOUND('',#6428,.T.);
#3934=FACE_OUTER_BOUND('',#6429,.T.);
#3935=FACE_OUTER_BOUND('',#6430,.T.);
#3936=FACE_OUTER_BOUND('',#6431,.T.);
#3937=FACE_OUTER_BOUND('',#6432,.T.);
#3938=FACE_OUTER_BOUND('',#6433,.T.);
#3939=FACE_OUTER_BOUND('',#6434,.T.);
#3940=FACE_OUTER_BOUND('',#6435,.T.);
#3941=FACE_OUTER_BOUND('',#6436,.T.);
#3942=FACE_OUTER_BOUND('',#6437,.T.);
#3943=FACE_OUTER_BOUND('',#6438,.T.);
#3944=FACE_OUTER_BOUND('',#6439,.T.);
#3945=FACE_OUTER_BOUND('',#6440,.T.);
#3946=FACE_OUTER_BOUND('',#6441,.T.);
#3947=FACE_OUTER_BOUND('',#6442,.T.);
#3948=FACE_OUTER_BOUND('',#6443,.T.);
#3949=FACE_OUTER_BOUND('',#6444,.T.);
#3950=FACE_OUTER_BOUND('',#6445,.T.);
#3951=FACE_OUTER_BOUND('',#6446,.T.);
#3952=FACE_OUTER_BOUND('',#6447,.T.);
#3953=FACE_OUTER_BOUND('',#6448,.T.);
#3954=FACE_OUTER_BOUND('',#6449,.T.);
#3955=FACE_OUTER_BOUND('',#6450,.T.);
#3956=FACE_OUTER_BOUND('',#6451,.T.);
#3957=FACE_OUTER_BOUND('',#6452,.T.);
#3958=FACE_OUTER_BOUND('',#6453,.T.);
#3959=FACE_OUTER_BOUND('',#6454,.T.);
#3960=FACE_OUTER_BOUND('',#6455,.T.);
#3961=FACE_OUTER_BOUND('',#6456,.T.);
#3962=FACE_OUTER_BOUND('',#6457,.T.);
#3963=FACE_OUTER_BOUND('',#6458,.T.);
#3964=FACE_OUTER_BOUND('',#6459,.T.);
#3965=FACE_OUTER_BOUND('',#6460,.T.);
#3966=FACE_OUTER_BOUND('',#6461,.T.);
#3967=FACE_OUTER_BOUND('',#6462,.T.);
#3968=FACE_OUTER_BOUND('',#6463,.T.);
#3969=FACE_OUTER_BOUND('',#6464,.T.);
#3970=FACE_OUTER_BOUND('',#6465,.T.);
#3971=FACE_OUTER_BOUND('',#6466,.T.);
#3972=FACE_OUTER_BOUND('',#6467,.T.);
#3973=FACE_OUTER_BOUND('',#6468,.T.);
#3974=FACE_OUTER_BOUND('',#6469,.T.);
#3975=FACE_OUTER_BOUND('',#6470,.T.);
#3976=FACE_OUTER_BOUND('',#6471,.T.);
#3977=FACE_OUTER_BOUND('',#6472,.T.);
#3978=FACE_OUTER_BOUND('',#6473,.T.);
#3979=FACE_OUTER_BOUND('',#6474,.T.);
#3980=FACE_OUTER_BOUND('',#6475,.T.);
#3981=FACE_OUTER_BOUND('',#6476,.T.);
#3982=FACE_OUTER_BOUND('',#6477,.T.);
#3983=FACE_OUTER_BOUND('',#6478,.T.);
#3984=FACE_OUTER_BOUND('',#6479,.T.);
#3985=FACE_OUTER_BOUND('',#6480,.T.);
#3986=FACE_OUTER_BOUND('',#6481,.T.);
#3987=FACE_OUTER_BOUND('',#6482,.T.);
#3988=FACE_OUTER_BOUND('',#6483,.T.);
#3989=FACE_OUTER_BOUND('',#6484,.T.);
#3990=FACE_OUTER_BOUND('',#6485,.T.);
#3991=FACE_OUTER_BOUND('',#6486,.T.);
#3992=FACE_OUTER_BOUND('',#6487,.T.);
#3993=FACE_OUTER_BOUND('',#6488,.T.);
#3994=FACE_OUTER_BOUND('',#6489,.T.);
#3995=FACE_OUTER_BOUND('',#6490,.T.);
#3996=FACE_OUTER_BOUND('',#6491,.T.);
#3997=FACE_OUTER_BOUND('',#6492,.T.);
#3998=FACE_OUTER_BOUND('',#6493,.T.);
#3999=FACE_OUTER_BOUND('',#6494,.T.);
#4000=FACE_OUTER_BOUND('',#6495,.T.);
#4001=FACE_OUTER_BOUND('',#6496,.T.);
#4002=FACE_OUTER_BOUND('',#6497,.T.);
#4003=FACE_OUTER_BOUND('',#6498,.T.);
#4004=FACE_OUTER_BOUND('',#6499,.T.);
#4005=FACE_OUTER_BOUND('',#6500,.T.);
#4006=FACE_OUTER_BOUND('',#6501,.T.);
#4007=FACE_OUTER_BOUND('',#6502,.T.);
#4008=FACE_OUTER_BOUND('',#6503,.T.);
#4009=FACE_OUTER_BOUND('',#6504,.T.);
#4010=FACE_OUTER_BOUND('',#6505,.T.);
#4011=FACE_OUTER_BOUND('',#6506,.T.);
#4012=FACE_OUTER_BOUND('',#6507,.T.);
#4013=FACE_OUTER_BOUND('',#6508,.T.);
#4014=FACE_OUTER_BOUND('',#6509,.T.);
#4015=FACE_OUTER_BOUND('',#6510,.T.);
#4016=FACE_OUTER_BOUND('',#6511,.T.);
#4017=FACE_OUTER_BOUND('',#6512,.T.);
#4018=FACE_OUTER_BOUND('',#6513,.T.);
#4019=FACE_OUTER_BOUND('',#6514,.T.);
#4020=FACE_OUTER_BOUND('',#6515,.T.);
#4021=FACE_OUTER_BOUND('',#6516,.T.);
#4022=FACE_OUTER_BOUND('',#6517,.T.);
#4023=FACE_OUTER_BOUND('',#6518,.T.);
#4024=FACE_OUTER_BOUND('',#6519,.T.);
#4025=FACE_OUTER_BOUND('',#6520,.T.);
#4026=FACE_OUTER_BOUND('',#6521,.T.);
#4027=FACE_OUTER_BOUND('',#6522,.T.);
#4028=FACE_OUTER_BOUND('',#6523,.T.);
#4029=FACE_OUTER_BOUND('',#6524,.T.);
#4030=FACE_OUTER_BOUND('',#6525,.T.);
#4031=FACE_OUTER_BOUND('',#6526,.T.);
#4032=FACE_OUTER_BOUND('',#6527,.T.);
#4033=FACE_OUTER_BOUND('',#6528,.T.);
#4034=FACE_OUTER_BOUND('',#6529,.T.);
#4035=FACE_OUTER_BOUND('',#6530,.T.);
#4036=FACE_OUTER_BOUND('',#6531,.T.);
#4037=FACE_OUTER_BOUND('',#6532,.T.);
#4038=FACE_OUTER_BOUND('',#6533,.T.);
#4039=FACE_OUTER_BOUND('',#6534,.T.);
#4040=FACE_OUTER_BOUND('',#6535,.T.);
#4041=FACE_OUTER_BOUND('',#6536,.T.);
#4042=FACE_OUTER_BOUND('',#6537,.T.);
#4043=FACE_OUTER_BOUND('',#6538,.T.);
#4044=FACE_OUTER_BOUND('',#6539,.T.);
#4045=FACE_OUTER_BOUND('',#6540,.T.);
#4046=FACE_OUTER_BOUND('',#6541,.T.);
#4047=FACE_OUTER_BOUND('',#6542,.T.);
#4048=FACE_OUTER_BOUND('',#6543,.T.);
#4049=FACE_OUTER_BOUND('',#6544,.T.);
#4050=FACE_OUTER_BOUND('',#6545,.T.);
#4051=FACE_OUTER_BOUND('',#6546,.T.);
#4052=FACE_OUTER_BOUND('',#6547,.T.);
#4053=FACE_OUTER_BOUND('',#6548,.T.);
#4054=FACE_OUTER_BOUND('',#6549,.T.);
#4055=FACE_OUTER_BOUND('',#6550,.T.);
#4056=FACE_OUTER_BOUND('',#6551,.T.);
#4057=FACE_OUTER_BOUND('',#6552,.T.);
#4058=FACE_OUTER_BOUND('',#6553,.T.);
#4059=FACE_OUTER_BOUND('',#6554,.T.);
#4060=FACE_OUTER_BOUND('',#6555,.T.);
#4061=FACE_OUTER_BOUND('',#6556,.T.);
#4062=FACE_OUTER_BOUND('',#6557,.T.);
#4063=FACE_OUTER_BOUND('',#6558,.T.);
#4064=FACE_OUTER_BOUND('',#6559,.T.);
#4065=FACE_OUTER_BOUND('',#6560,.T.);
#4066=FACE_OUTER_BOUND('',#6561,.T.);
#4067=FACE_OUTER_BOUND('',#6562,.T.);
#4068=FACE_OUTER_BOUND('',#6563,.T.);
#4069=FACE_OUTER_BOUND('',#6564,.T.);
#4070=FACE_OUTER_BOUND('',#6565,.T.);
#4071=FACE_OUTER_BOUND('',#6566,.T.);
#4072=FACE_OUTER_BOUND('',#6567,.T.);
#4073=FACE_OUTER_BOUND('',#6568,.T.);
#4074=FACE_OUTER_BOUND('',#6569,.T.);
#4075=FACE_OUTER_BOUND('',#6570,.T.);
#4076=FACE_OUTER_BOUND('',#6571,.T.);
#4077=FACE_OUTER_BOUND('',#6572,.T.);
#4078=FACE_OUTER_BOUND('',#6573,.T.);
#4079=FACE_OUTER_BOUND('',#6574,.T.);
#4080=FACE_OUTER_BOUND('',#6575,.T.);
#4081=FACE_OUTER_BOUND('',#6576,.T.);
#4082=FACE_OUTER_BOUND('',#6577,.T.);
#4083=FACE_OUTER_BOUND('',#6578,.T.);
#4084=FACE_OUTER_BOUND('',#6579,.T.);
#4085=FACE_OUTER_BOUND('',#6580,.T.);
#4086=FACE_OUTER_BOUND('',#6581,.T.);
#4087=FACE_OUTER_BOUND('',#6582,.T.);
#4088=FACE_OUTER_BOUND('',#6583,.T.);
#4089=FACE_OUTER_BOUND('',#6584,.T.);
#4090=FACE_OUTER_BOUND('',#6585,.T.);
#4091=FACE_OUTER_BOUND('',#6586,.T.);
#4092=FACE_OUTER_BOUND('',#6587,.T.);
#4093=FACE_OUTER_BOUND('',#6588,.T.);
#4094=FACE_OUTER_BOUND('',#6589,.T.);
#4095=FACE_OUTER_BOUND('',#6590,.T.);
#4096=FACE_OUTER_BOUND('',#6591,.T.);
#4097=FACE_OUTER_BOUND('',#6592,.T.);
#4098=FACE_OUTER_BOUND('',#6593,.T.);
#4099=FACE_OUTER_BOUND('',#6594,.T.);
#4100=FACE_OUTER_BOUND('',#6595,.T.);
#4101=FACE_OUTER_BOUND('',#6596,.T.);
#4102=FACE_OUTER_BOUND('',#6597,.T.);
#4103=FACE_OUTER_BOUND('',#6598,.T.);
#4104=FACE_OUTER_BOUND('',#6599,.T.);
#4105=FACE_OUTER_BOUND('',#6600,.T.);
#4106=FACE_OUTER_BOUND('',#6601,.T.);
#4107=FACE_OUTER_BOUND('',#6602,.T.);
#4108=FACE_OUTER_BOUND('',#6603,.T.);
#4109=FACE_OUTER_BOUND('',#6604,.T.);
#4110=FACE_OUTER_BOUND('',#6605,.T.);
#4111=FACE_OUTER_BOUND('',#6606,.T.);
#4112=FACE_OUTER_BOUND('',#6607,.T.);
#4113=FACE_OUTER_BOUND('',#6608,.T.);
#4114=FACE_OUTER_BOUND('',#6609,.T.);
#4115=FACE_OUTER_BOUND('',#6610,.T.);
#4116=FACE_OUTER_BOUND('',#6611,.T.);
#4117=FACE_OUTER_BOUND('',#6612,.T.);
#4118=FACE_OUTER_BOUND('',#6613,.T.);
#4119=FACE_OUTER_BOUND('',#6614,.T.);
#4120=FACE_OUTER_BOUND('',#6615,.T.);
#4121=FACE_OUTER_BOUND('',#6616,.T.);
#4122=FACE_OUTER_BOUND('',#6617,.T.);
#4123=FACE_OUTER_BOUND('',#6618,.T.);
#4124=FACE_OUTER_BOUND('',#6619,.T.);
#4125=FACE_OUTER_BOUND('',#6620,.T.);
#4126=FACE_OUTER_BOUND('',#6621,.T.);
#4127=FACE_OUTER_BOUND('',#6622,.T.);
#4128=FACE_OUTER_BOUND('',#6623,.T.);
#4129=FACE_OUTER_BOUND('',#6624,.T.);
#4130=FACE_OUTER_BOUND('',#6625,.T.);
#4131=FACE_OUTER_BOUND('',#6626,.T.);
#4132=FACE_OUTER_BOUND('',#6627,.T.);
#4133=FACE_OUTER_BOUND('',#6628,.T.);
#4134=FACE_OUTER_BOUND('',#6629,.T.);
#4135=FACE_OUTER_BOUND('',#6630,.T.);
#4136=FACE_OUTER_BOUND('',#6631,.T.);
#4137=FACE_OUTER_BOUND('',#6632,.T.);
#4138=FACE_OUTER_BOUND('',#6633,.T.);
#4139=FACE_OUTER_BOUND('',#6634,.T.);
#4140=FACE_OUTER_BOUND('',#6635,.T.);
#4141=FACE_OUTER_BOUND('',#6636,.T.);
#4142=FACE_OUTER_BOUND('',#6637,.T.);
#4143=FACE_OUTER_BOUND('',#6638,.T.);
#4144=FACE_OUTER_BOUND('',#6639,.T.);
#4145=FACE_OUTER_BOUND('',#6640,.T.);
#4146=FACE_OUTER_BOUND('',#6641,.T.);
#4147=FACE_OUTER_BOUND('',#6642,.T.);
#4148=FACE_OUTER_BOUND('',#6643,.T.);
#4149=FACE_OUTER_BOUND('',#6644,.T.);
#4150=FACE_OUTER_BOUND('',#6645,.T.);
#4151=FACE_OUTER_BOUND('',#6646,.T.);
#4152=FACE_OUTER_BOUND('',#6647,.T.);
#4153=FACE_OUTER_BOUND('',#6648,.T.);
#4154=FACE_OUTER_BOUND('',#6649,.T.);
#4155=FACE_OUTER_BOUND('',#6650,.T.);
#4156=FACE_OUTER_BOUND('',#6651,.T.);
#4157=FACE_OUTER_BOUND('',#6652,.T.);
#4158=FACE_OUTER_BOUND('',#6653,.T.);
#4159=FACE_OUTER_BOUND('',#6654,.T.);
#4160=FACE_OUTER_BOUND('',#6655,.T.);
#4161=FACE_OUTER_BOUND('',#6656,.T.);
#4162=FACE_OUTER_BOUND('',#6657,.T.);
#4163=FACE_OUTER_BOUND('',#6658,.T.);
#4164=FACE_OUTER_BOUND('',#6659,.T.);
#4165=FACE_OUTER_BOUND('',#6660,.T.);
#4166=FACE_OUTER_BOUND('',#6661,.T.);
#4167=FACE_OUTER_BOUND('',#6662,.T.);
#4168=FACE_OUTER_BOUND('',#6663,.T.);
#4169=FACE_OUTER_BOUND('',#6664,.T.);
#4170=FACE_OUTER_BOUND('',#6665,.T.);
#4171=FACE_OUTER_BOUND('',#6666,.T.);
#4172=FACE_OUTER_BOUND('',#6667,.T.);
#4173=FACE_OUTER_BOUND('',#6668,.T.);
#4174=FACE_OUTER_BOUND('',#6669,.T.);
#4175=FACE_OUTER_BOUND('',#6670,.T.);
#4176=FACE_OUTER_BOUND('',#6671,.T.);
#4177=FACE_OUTER_BOUND('',#6672,.T.);
#4178=FACE_OUTER_BOUND('',#6673,.T.);
#4179=FACE_OUTER_BOUND('',#6674,.T.);
#4180=FACE_OUTER_BOUND('',#6675,.T.);
#4181=FACE_OUTER_BOUND('',#6676,.T.);
#4182=FACE_OUTER_BOUND('',#6677,.T.);
#4183=FACE_OUTER_BOUND('',#6678,.T.);
#4184=FACE_OUTER_BOUND('',#6679,.T.);
#4185=FACE_OUTER_BOUND('',#6680,.T.);
#4186=FACE_OUTER_BOUND('',#6681,.T.);
#4187=FACE_OUTER_BOUND('',#6682,.T.);
#4188=FACE_OUTER_BOUND('',#6683,.T.);
#4189=FACE_OUTER_BOUND('',#6684,.T.);
#4190=FACE_OUTER_BOUND('',#6685,.T.);
#4191=FACE_OUTER_BOUND('',#6686,.T.);
#4192=FACE_OUTER_BOUND('',#6687,.T.);
#4193=FACE_OUTER_BOUND('',#6688,.T.);
#4194=FACE_OUTER_BOUND('',#6689,.T.);
#4195=FACE_OUTER_BOUND('',#6690,.T.);
#4196=FACE_OUTER_BOUND('',#6691,.T.);
#4197=FACE_OUTER_BOUND('',#6692,.T.);
#4198=FACE_OUTER_BOUND('',#6693,.T.);
#4199=FACE_OUTER_BOUND('',#6694,.T.);
#4200=FACE_OUTER_BOUND('',#6695,.T.);
#4201=FACE_OUTER_BOUND('',#6696,.T.);
#4202=FACE_OUTER_BOUND('',#6697,.T.);
#4203=FACE_OUTER_BOUND('',#6698,.T.);
#4204=FACE_OUTER_BOUND('',#6699,.T.);
#4205=FACE_OUTER_BOUND('',#6700,.T.);
#4206=FACE_OUTER_BOUND('',#6701,.T.);
#4207=FACE_OUTER_BOUND('',#6702,.T.);
#4208=FACE_OUTER_BOUND('',#6703,.T.);
#4209=FACE_OUTER_BOUND('',#6704,.T.);
#4210=FACE_OUTER_BOUND('',#6705,.T.);
#4211=FACE_OUTER_BOUND('',#6706,.T.);
#4212=FACE_OUTER_BOUND('',#6707,.T.);
#4213=FACE_OUTER_BOUND('',#6708,.T.);
#4214=FACE_OUTER_BOUND('',#6709,.T.);
#4215=FACE_OUTER_BOUND('',#6710,.T.);
#4216=FACE_OUTER_BOUND('',#6711,.T.);
#4217=FACE_OUTER_BOUND('',#6712,.T.);
#4218=FACE_OUTER_BOUND('',#6713,.T.);
#4219=FACE_OUTER_BOUND('',#6714,.T.);
#4220=FACE_OUTER_BOUND('',#6715,.T.);
#4221=FACE_OUTER_BOUND('',#6716,.T.);
#4222=FACE_OUTER_BOUND('',#6717,.T.);
#4223=FACE_OUTER_BOUND('',#6718,.T.);
#4224=FACE_OUTER_BOUND('',#6719,.T.);
#4225=FACE_OUTER_BOUND('',#6720,.T.);
#4226=FACE_OUTER_BOUND('',#6721,.T.);
#4227=FACE_OUTER_BOUND('',#6722,.T.);
#4228=FACE_OUTER_BOUND('',#6723,.T.);
#4229=FACE_OUTER_BOUND('',#6724,.T.);
#4230=FACE_OUTER_BOUND('',#6725,.T.);
#4231=FACE_OUTER_BOUND('',#6726,.T.);
#4232=FACE_OUTER_BOUND('',#6727,.T.);
#4233=FACE_OUTER_BOUND('',#6728,.T.);
#4234=FACE_OUTER_BOUND('',#6729,.T.);
#4235=FACE_OUTER_BOUND('',#6730,.T.);
#4236=FACE_OUTER_BOUND('',#6731,.T.);
#4237=FACE_OUTER_BOUND('',#6732,.T.);
#4238=FACE_OUTER_BOUND('',#6733,.T.);
#4239=FACE_OUTER_BOUND('',#6734,.T.);
#4240=FACE_OUTER_BOUND('',#6735,.T.);
#4241=FACE_OUTER_BOUND('',#6736,.T.);
#4242=FACE_OUTER_BOUND('',#6737,.T.);
#4243=FACE_OUTER_BOUND('',#6738,.T.);
#4244=FACE_OUTER_BOUND('',#6739,.T.);
#4245=EDGE_LOOP('',(#26477,#26478,#26479,#26480));
#4246=EDGE_LOOP('',(#26481,#26482,#26483,#26484));
#4247=EDGE_LOOP('',(#26485,#26486,#26487,#26488));
#4248=EDGE_LOOP('',(#26489,#26490,#26491,#26492));
#4249=EDGE_LOOP('',(#26493,#26494,#26495,#26496));
#4250=EDGE_LOOP('',(#26497,#26498,#26499,#26500));
#4251=EDGE_LOOP('',(#26501,#26502,#26503,#26504));
#4252=EDGE_LOOP('',(#26505,#26506,#26507,#26508));
#4253=EDGE_LOOP('',(#26509,#26510,#26511,#26512));
#4254=EDGE_LOOP('',(#26513,#26514,#26515,#26516));
#4255=EDGE_LOOP('',(#26517,#26518,#26519,#26520));
#4256=EDGE_LOOP('',(#26521,#26522,#26523,#26524));
#4257=EDGE_LOOP('',(#26525,#26526,#26527,#26528));
#4258=EDGE_LOOP('',(#26529,#26530,#26531,#26532));
#4259=EDGE_LOOP('',(#26533,#26534,#26535,#26536));
#4260=EDGE_LOOP('',(#26537,#26538,#26539,#26540));
#4261=EDGE_LOOP('',(#26541,#26542,#26543,#26544));
#4262=EDGE_LOOP('',(#26545,#26546,#26547,#26548));
#4263=EDGE_LOOP('',(#26549,#26550,#26551,#26552));
#4264=EDGE_LOOP('',(#26553,#26554,#26555,#26556));
#4265=EDGE_LOOP('',(#26557,#26558,#26559,#26560));
#4266=EDGE_LOOP('',(#26561,#26562,#26563,#26564));
#4267=EDGE_LOOP('',(#26565,#26566,#26567,#26568));
#4268=EDGE_LOOP('',(#26569,#26570,#26571,#26572));
#4269=EDGE_LOOP('',(#26573,#26574,#26575,#26576));
#4270=EDGE_LOOP('',(#26577,#26578,#26579,#26580));
#4271=EDGE_LOOP('',(#26581,#26582,#26583,#26584));
#4272=EDGE_LOOP('',(#26585,#26586,#26587,#26588));
#4273=EDGE_LOOP('',(#26589,#26590,#26591,#26592));
#4274=EDGE_LOOP('',(#26593,#26594,#26595,#26596));
#4275=EDGE_LOOP('',(#26597,#26598,#26599,#26600));
#4276=EDGE_LOOP('',(#26601,#26602,#26603,#26604));
#4277=EDGE_LOOP('',(#26605,#26606,#26607,#26608));
#4278=EDGE_LOOP('',(#26609,#26610,#26611,#26612));
#4279=EDGE_LOOP('',(#26613,#26614,#26615,#26616));
#4280=EDGE_LOOP('',(#26617,#26618,#26619,#26620));
#4281=EDGE_LOOP('',(#26621,#26622,#26623,#26624));
#4282=EDGE_LOOP('',(#26625,#26626,#26627,#26628));
#4283=EDGE_LOOP('',(#26629,#26630,#26631,#26632));
#4284=EDGE_LOOP('',(#26633,#26634,#26635,#26636));
#4285=EDGE_LOOP('',(#26637,#26638,#26639,#26640));
#4286=EDGE_LOOP('',(#26641,#26642,#26643,#26644));
#4287=EDGE_LOOP('',(#26645,#26646,#26647,#26648));
#4288=EDGE_LOOP('',(#26649,#26650,#26651,#26652));
#4289=EDGE_LOOP('',(#26653,#26654,#26655,#26656));
#4290=EDGE_LOOP('',(#26657,#26658,#26659,#26660));
#4291=EDGE_LOOP('',(#26661,#26662,#26663,#26664));
#4292=EDGE_LOOP('',(#26665,#26666,#26667,#26668));
#4293=EDGE_LOOP('',(#26669,#26670,#26671,#26672));
#4294=EDGE_LOOP('',(#26673,#26674,#26675,#26676));
#4295=EDGE_LOOP('',(#26677,#26678,#26679,#26680));
#4296=EDGE_LOOP('',(#26681,#26682,#26683,#26684));
#4297=EDGE_LOOP('',(#26685,#26686,#26687,#26688));
#4298=EDGE_LOOP('',(#26689,#26690,#26691,#26692));
#4299=EDGE_LOOP('',(#26693,#26694,#26695,#26696));
#4300=EDGE_LOOP('',(#26697,#26698,#26699,#26700));
#4301=EDGE_LOOP('',(#26701,#26702,#26703,#26704));
#4302=EDGE_LOOP('',(#26705,#26706,#26707,#26708));
#4303=EDGE_LOOP('',(#26709,#26710,#26711,#26712));
#4304=EDGE_LOOP('',(#26713,#26714,#26715,#26716));
#4305=EDGE_LOOP('',(#26717,#26718,#26719,#26720));
#4306=EDGE_LOOP('',(#26721,#26722,#26723,#26724));
#4307=EDGE_LOOP('',(#26725,#26726,#26727,#26728));
#4308=EDGE_LOOP('',(#26729,#26730,#26731,#26732));
#4309=EDGE_LOOP('',(#26733,#26734,#26735,#26736));
#4310=EDGE_LOOP('',(#26737,#26738,#26739,#26740));
#4311=EDGE_LOOP('',(#26741,#26742,#26743,#26744));
#4312=EDGE_LOOP('',(#26745,#26746,#26747,#26748));
#4313=EDGE_LOOP('',(#26749,#26750,#26751,#26752));
#4314=EDGE_LOOP('',(#26753,#26754,#26755,#26756));
#4315=EDGE_LOOP('',(#26757,#26758,#26759,#26760));
#4316=EDGE_LOOP('',(#26761,#26762,#26763,#26764));
#4317=EDGE_LOOP('',(#26765,#26766,#26767,#26768));
#4318=EDGE_LOOP('',(#26769,#26770,#26771,#26772));
#4319=EDGE_LOOP('',(#26773,#26774,#26775,#26776));
#4320=EDGE_LOOP('',(#26777,#26778,#26779,#26780));
#4321=EDGE_LOOP('',(#26781,#26782,#26783,#26784));
#4322=EDGE_LOOP('',(#26785,#26786,#26787,#26788));
#4323=EDGE_LOOP('',(#26789,#26790,#26791,#26792));
#4324=EDGE_LOOP('',(#26793,#26794,#26795,#26796));
#4325=EDGE_LOOP('',(#26797,#26798,#26799,#26800));
#4326=EDGE_LOOP('',(#26801,#26802,#26803,#26804));
#4327=EDGE_LOOP('',(#26805,#26806,#26807,#26808));
#4328=EDGE_LOOP('',(#26809,#26810,#26811,#26812));
#4329=EDGE_LOOP('',(#26813,#26814,#26815,#26816));
#4330=EDGE_LOOP('',(#26817,#26818,#26819,#26820));
#4331=EDGE_LOOP('',(#26821,#26822,#26823,#26824));
#4332=EDGE_LOOP('',(#26825,#26826,#26827,#26828));
#4333=EDGE_LOOP('',(#26829,#26830,#26831,#26832));
#4334=EDGE_LOOP('',(#26833,#26834,#26835,#26836));
#4335=EDGE_LOOP('',(#26837,#26838,#26839,#26840,#26841,#26842,#26843,#26844,
#26845,#26846,#26847,#26848,#26849,#26850,#26851,#26852,#26853,#26854,#26855,
#26856,#26857,#26858,#26859,#26860,#26861,#26862,#26863,#26864));
#4336=EDGE_LOOP('',(#26865,#26866,#26867,#26868,#26869,#26870,#26871,#26872));
#4337=EDGE_LOOP('',(#26873,#26874,#26875,#26876,#26877,#26878,#26879,#26880));
#4338=EDGE_LOOP('',(#26881,#26882,#26883,#26884,#26885,#26886,#26887,#26888));
#4339=EDGE_LOOP('',(#26889,#26890,#26891,#26892,#26893,#26894,#26895,#26896));
#4340=EDGE_LOOP('',(#26897,#26898,#26899,#26900,#26901,#26902,#26903,#26904,
#26905,#26906,#26907,#26908,#26909,#26910,#26911,#26912,#26913,#26914,#26915,
#26916,#26917,#26918,#26919,#26920,#26921,#26922,#26923,#26924));
#4341=EDGE_LOOP('',(#26925,#26926,#26927,#26928));
#4342=EDGE_LOOP('',(#26929,#26930,#26931,#26932));
#4343=EDGE_LOOP('',(#26933,#26934,#26935,#26936));
#4344=EDGE_LOOP('',(#26937,#26938,#26939,#26940));
#4345=EDGE_LOOP('',(#26941,#26942,#26943,#26944));
#4346=EDGE_LOOP('',(#26945,#26946,#26947,#26948));
#4347=EDGE_LOOP('',(#26949,#26950,#26951,#26952,#26953,#26954));
#4348=EDGE_LOOP('',(#26955,#26956,#26957,#26958,#26959,#26960,#26961,#26962));
#4349=EDGE_LOOP('',(#26963,#26964,#26965,#26966,#26967,#26968,#26969,#26970));
#4350=EDGE_LOOP('',(#26971,#26972,#26973,#26974,#26975,#26976));
#4351=EDGE_LOOP('',(#26977,#26978,#26979,#26980));
#4352=EDGE_LOOP('',(#26981,#26982,#26983,#26984));
#4353=EDGE_LOOP('',(#26985,#26986,#26987,#26988));
#4354=EDGE_LOOP('',(#26989,#26990,#26991,#26992));
#4355=EDGE_LOOP('',(#26993,#26994,#26995,#26996,#26997,#26998,#26999,#27000,
#27001,#27002));
#4356=EDGE_LOOP('',(#27003,#27004,#27005,#27006));
#4357=EDGE_LOOP('',(#27007,#27008,#27009,#27010));
#4358=EDGE_LOOP('',(#27011,#27012,#27013,#27014));
#4359=EDGE_LOOP('',(#27015,#27016,#27017,#27018));
#4360=EDGE_LOOP('',(#27019,#27020,#27021,#27022));
#4361=EDGE_LOOP('',(#27023,#27024,#27025,#27026));
#4362=EDGE_LOOP('',(#27027,#27028,#27029,#27030));
#4363=EDGE_LOOP('',(#27031,#27032,#27033,#27034));
#4364=EDGE_LOOP('',(#27035,#27036,#27037,#27038));
#4365=EDGE_LOOP('',(#27039,#27040,#27041,#27042));
#4366=EDGE_LOOP('',(#27043,#27044,#27045,#27046));
#4367=EDGE_LOOP('',(#27047,#27048,#27049,#27050));
#4368=EDGE_LOOP('',(#27051,#27052,#27053,#27054));
#4369=EDGE_LOOP('',(#27055,#27056,#27057,#27058));
#4370=EDGE_LOOP('',(#27059,#27060,#27061,#27062));
#4371=EDGE_LOOP('',(#27063,#27064,#27065,#27066));
#4372=EDGE_LOOP('',(#27067,#27068,#27069,#27070));
#4373=EDGE_LOOP('',(#27071,#27072,#27073,#27074));
#4374=EDGE_LOOP('',(#27075,#27076,#27077,#27078));
#4375=EDGE_LOOP('',(#27079,#27080,#27081,#27082));
#4376=EDGE_LOOP('',(#27083,#27084,#27085,#27086));
#4377=EDGE_LOOP('',(#27087,#27088,#27089,#27090));
#4378=EDGE_LOOP('',(#27091,#27092,#27093,#27094));
#4379=EDGE_LOOP('',(#27095,#27096,#27097,#27098));
#4380=EDGE_LOOP('',(#27099,#27100,#27101,#27102));
#4381=EDGE_LOOP('',(#27103,#27104,#27105,#27106));
#4382=EDGE_LOOP('',(#27107,#27108,#27109,#27110));
#4383=EDGE_LOOP('',(#27111,#27112,#27113,#27114));
#4384=EDGE_LOOP('',(#27115,#27116,#27117,#27118));
#4385=EDGE_LOOP('',(#27119,#27120,#27121,#27122));
#4386=EDGE_LOOP('',(#27123,#27124,#27125,#27126));
#4387=EDGE_LOOP('',(#27127,#27128,#27129,#27130));
#4388=EDGE_LOOP('',(#27131,#27132,#27133,#27134));
#4389=EDGE_LOOP('',(#27135,#27136,#27137,#27138));
#4390=EDGE_LOOP('',(#27139,#27140,#27141,#27142));
#4391=EDGE_LOOP('',(#27143,#27144,#27145,#27146));
#4392=EDGE_LOOP('',(#27147,#27148,#27149,#27150));
#4393=EDGE_LOOP('',(#27151,#27152,#27153,#27154));
#4394=EDGE_LOOP('',(#27155,#27156,#27157,#27158));
#4395=EDGE_LOOP('',(#27159,#27160,#27161,#27162));
#4396=EDGE_LOOP('',(#27163,#27164,#27165,#27166));
#4397=EDGE_LOOP('',(#27167,#27168,#27169,#27170));
#4398=EDGE_LOOP('',(#27171,#27172,#27173,#27174));
#4399=EDGE_LOOP('',(#27175,#27176,#27177,#27178));
#4400=EDGE_LOOP('',(#27179,#27180,#27181,#27182));
#4401=EDGE_LOOP('',(#27183,#27184,#27185,#27186));
#4402=EDGE_LOOP('',(#27187,#27188,#27189,#27190));
#4403=EDGE_LOOP('',(#27191,#27192,#27193,#27194));
#4404=EDGE_LOOP('',(#27195,#27196,#27197,#27198,#27199,#27200,#27201,#27202,
#27203,#27204));
#4405=EDGE_LOOP('',(#27205,#27206,#27207,#27208));
#4406=EDGE_LOOP('',(#27209,#27210,#27211,#27212));
#4407=EDGE_LOOP('',(#27213,#27214,#27215,#27216));
#4408=EDGE_LOOP('',(#27217,#27218,#27219,#27220));
#4409=EDGE_LOOP('',(#27221,#27222,#27223,#27224));
#4410=EDGE_LOOP('',(#27225,#27226,#27227,#27228));
#4411=EDGE_LOOP('',(#27229,#27230,#27231,#27232));
#4412=EDGE_LOOP('',(#27233,#27234,#27235,#27236));
#4413=EDGE_LOOP('',(#27237,#27238,#27239,#27240));
#4414=EDGE_LOOP('',(#27241,#27242,#27243,#27244));
#4415=EDGE_LOOP('',(#27245,#27246,#27247,#27248));
#4416=EDGE_LOOP('',(#27249,#27250,#27251,#27252));
#4417=EDGE_LOOP('',(#27253,#27254,#27255,#27256));
#4418=EDGE_LOOP('',(#27257,#27258,#27259,#27260));
#4419=EDGE_LOOP('',(#27261,#27262,#27263,#27264));
#4420=EDGE_LOOP('',(#27265,#27266,#27267,#27268));
#4421=EDGE_LOOP('',(#27269,#27270,#27271,#27272));
#4422=EDGE_LOOP('',(#27273,#27274,#27275,#27276));
#4423=EDGE_LOOP('',(#27277,#27278,#27279,#27280));
#4424=EDGE_LOOP('',(#27281,#27282,#27283,#27284));
#4425=EDGE_LOOP('',(#27285,#27286,#27287,#27288));
#4426=EDGE_LOOP('',(#27289,#27290,#27291,#27292));
#4427=EDGE_LOOP('',(#27293,#27294,#27295,#27296));
#4428=EDGE_LOOP('',(#27297,#27298,#27299,#27300));
#4429=EDGE_LOOP('',(#27301,#27302,#27303,#27304));
#4430=EDGE_LOOP('',(#27305,#27306,#27307,#27308));
#4431=EDGE_LOOP('',(#27309,#27310,#27311,#27312));
#4432=EDGE_LOOP('',(#27313,#27314,#27315,#27316));
#4433=EDGE_LOOP('',(#27317,#27318,#27319,#27320));
#4434=EDGE_LOOP('',(#27321,#27322,#27323,#27324));
#4435=EDGE_LOOP('',(#27325,#27326,#27327,#27328));
#4436=EDGE_LOOP('',(#27329,#27330,#27331,#27332));
#4437=EDGE_LOOP('',(#27333,#27334,#27335,#27336));
#4438=EDGE_LOOP('',(#27337,#27338,#27339,#27340));
#4439=EDGE_LOOP('',(#27341,#27342,#27343,#27344));
#4440=EDGE_LOOP('',(#27345,#27346,#27347,#27348));
#4441=EDGE_LOOP('',(#27349,#27350,#27351,#27352));
#4442=EDGE_LOOP('',(#27353,#27354,#27355,#27356));
#4443=EDGE_LOOP('',(#27357,#27358,#27359,#27360));
#4444=EDGE_LOOP('',(#27361,#27362,#27363,#27364));
#4445=EDGE_LOOP('',(#27365,#27366,#27367,#27368));
#4446=EDGE_LOOP('',(#27369,#27370,#27371,#27372));
#4447=EDGE_LOOP('',(#27373,#27374,#27375,#27376));
#4448=EDGE_LOOP('',(#27377,#27378,#27379,#27380));
#4449=EDGE_LOOP('',(#27381,#27382,#27383,#27384));
#4450=EDGE_LOOP('',(#27385,#27386,#27387,#27388));
#4451=EDGE_LOOP('',(#27389,#27390,#27391,#27392));
#4452=EDGE_LOOP('',(#27393,#27394,#27395,#27396));
#4453=EDGE_LOOP('',(#27397,#27398,#27399,#27400));
#4454=EDGE_LOOP('',(#27401,#27402,#27403,#27404));
#4455=EDGE_LOOP('',(#27405,#27406,#27407,#27408));
#4456=EDGE_LOOP('',(#27409,#27410,#27411,#27412));
#4457=EDGE_LOOP('',(#27413,#27414,#27415,#27416));
#4458=EDGE_LOOP('',(#27417,#27418,#27419,#27420));
#4459=EDGE_LOOP('',(#27421,#27422,#27423,#27424));
#4460=EDGE_LOOP('',(#27425,#27426,#27427,#27428));
#4461=EDGE_LOOP('',(#27429,#27430,#27431,#27432));
#4462=EDGE_LOOP('',(#27433,#27434,#27435,#27436));
#4463=EDGE_LOOP('',(#27437,#27438,#27439,#27440));
#4464=EDGE_LOOP('',(#27441,#27442,#27443,#27444));
#4465=EDGE_LOOP('',(#27445,#27446,#27447,#27448));
#4466=EDGE_LOOP('',(#27449,#27450,#27451,#27452));
#4467=EDGE_LOOP('',(#27453,#27454,#27455,#27456));
#4468=EDGE_LOOP('',(#27457,#27458,#27459,#27460));
#4469=EDGE_LOOP('',(#27461,#27462,#27463,#27464));
#4470=EDGE_LOOP('',(#27465,#27466,#27467,#27468));
#4471=EDGE_LOOP('',(#27469,#27470,#27471,#27472));
#4472=EDGE_LOOP('',(#27473,#27474,#27475,#27476));
#4473=EDGE_LOOP('',(#27477,#27478,#27479,#27480));
#4474=EDGE_LOOP('',(#27481,#27482,#27483,#27484));
#4475=EDGE_LOOP('',(#27485,#27486,#27487,#27488));
#4476=EDGE_LOOP('',(#27489,#27490,#27491,#27492));
#4477=EDGE_LOOP('',(#27493,#27494,#27495,#27496));
#4478=EDGE_LOOP('',(#27497));
#4479=EDGE_LOOP('',(#27498,#27499,#27500,#27501,#27502,#27503,#27504,#27505,
#27506,#27507));
#4480=EDGE_LOOP('',(#27508,#27509,#27510,#27511,#27512,#27513,#27514,#27515,
#27516,#27517));
#4481=EDGE_LOOP('',(#27518,#27519,#27520,#27521,#27522,#27523,#27524,#27525));
#4482=EDGE_LOOP('',(#27526,#27527,#27528,#27529,#27530,#27531,#27532,#27533));
#4483=EDGE_LOOP('',(#27534,#27535,#27536,#27537,#27538,#27539,#27540,#27541));
#4484=EDGE_LOOP('',(#27542,#27543,#27544,#27545,#27546,#27547,#27548,#27549));
#4485=EDGE_LOOP('',(#27550,#27551,#27552,#27553,#27554,#27555,#27556,#27557));
#4486=EDGE_LOOP('',(#27558,#27559,#27560,#27561,#27562,#27563,#27564,#27565));
#4487=EDGE_LOOP('',(#27566,#27567,#27568,#27569,#27570,#27571,#27572,#27573));
#4488=EDGE_LOOP('',(#27574,#27575,#27576,#27577,#27578,#27579,#27580,#27581));
#4489=EDGE_LOOP('',(#27582,#27583,#27584,#27585,#27586,#27587,#27588,#27589));
#4490=EDGE_LOOP('',(#27590,#27591,#27592,#27593,#27594,#27595,#27596,#27597));
#4491=EDGE_LOOP('',(#27598,#27599,#27600,#27601,#27602,#27603,#27604,#27605));
#4492=EDGE_LOOP('',(#27606,#27607,#27608,#27609,#27610,#27611,#27612,#27613));
#4493=EDGE_LOOP('',(#27614,#27615,#27616,#27617,#27618,#27619,#27620,#27621));
#4494=EDGE_LOOP('',(#27622,#27623,#27624,#27625,#27626,#27627,#27628,#27629));
#4495=EDGE_LOOP('',(#27630,#27631,#27632,#27633,#27634,#27635,#27636,#27637));
#4496=EDGE_LOOP('',(#27638,#27639,#27640,#27641,#27642,#27643,#27644,#27645,
#27646,#27647));
#4497=EDGE_LOOP('',(#27648,#27649,#27650,#27651));
#4498=EDGE_LOOP('',(#27652,#27653,#27654,#27655));
#4499=EDGE_LOOP('',(#27656,#27657,#27658,#27659));
#4500=EDGE_LOOP('',(#27660,#27661,#27662,#27663));
#4501=EDGE_LOOP('',(#27664,#27665,#27666,#27667));
#4502=EDGE_LOOP('',(#27668,#27669,#27670,#27671,#27672,#27673,#27674,#27675,
#27676,#27677));
#4503=EDGE_LOOP('',(#27678));
#4504=EDGE_LOOP('',(#27679));
#4505=EDGE_LOOP('',(#27680));
#4506=EDGE_LOOP('',(#27681));
#4507=EDGE_LOOP('',(#27682));
#4508=EDGE_LOOP('',(#27683));
#4509=EDGE_LOOP('',(#27684,#27685,#27686,#27687));
#4510=EDGE_LOOP('',(#27688,#27689,#27690,#27691,#27692,#27693,#27694,#27695,
#27696,#27697,#27698,#27699));
#4511=EDGE_LOOP('',(#27700));
#4512=EDGE_LOOP('',(#27701));
#4513=EDGE_LOOP('',(#27702));
#4514=EDGE_LOOP('',(#27703,#27704,#27705,#27706,#27707,#27708,#27709,#27710,
#27711,#27712));
#4515=EDGE_LOOP('',(#27713));
#4516=EDGE_LOOP('',(#27714));
#4517=EDGE_LOOP('',(#27715));
#4518=EDGE_LOOP('',(#27716));
#4519=EDGE_LOOP('',(#27717));
#4520=EDGE_LOOP('',(#27718));
#4521=EDGE_LOOP('',(#27719,#27720,#27721,#27722));
#4522=EDGE_LOOP('',(#27723,#27724,#27725,#27726,#27727,#27728,#27729,#27730,
#27731,#27732,#27733,#27734));
#4523=EDGE_LOOP('',(#27735));
#4524=EDGE_LOOP('',(#27736));
#4525=EDGE_LOOP('',(#27737));
#4526=EDGE_LOOP('',(#27738,#27739,#27740,#27741,#27742));
#4527=EDGE_LOOP('',(#27743,#27744,#27745,#27746));
#4528=EDGE_LOOP('',(#27747,#27748,#27749,#27750,#27751));
#4529=EDGE_LOOP('',(#27752,#27753,#27754,#27755));
#4530=EDGE_LOOP('',(#27756,#27757,#27758,#27759,#27760));
#4531=EDGE_LOOP('',(#27761,#27762,#27763,#27764));
#4532=EDGE_LOOP('',(#27765,#27766,#27767,#27768,#27769));
#4533=EDGE_LOOP('',(#27770,#27771,#27772,#27773));
#4534=EDGE_LOOP('',(#27774,#27775,#27776,#27777,#27778,#27779));
#4535=EDGE_LOOP('',(#27780,#27781,#27782,#27783,#27784,#27785));
#4536=EDGE_LOOP('',(#27786,#27787,#27788,#27789));
#4537=EDGE_LOOP('',(#27790,#27791,#27792,#27793));
#4538=EDGE_LOOP('',(#27794,#27795,#27796,#27797));
#4539=EDGE_LOOP('',(#27798,#27799,#27800,#27801));
#4540=EDGE_LOOP('',(#27802,#27803,#27804,#27805));
#4541=EDGE_LOOP('',(#27806,#27807,#27808,#27809));
#4542=EDGE_LOOP('',(#27810,#27811,#27812,#27813));
#4543=EDGE_LOOP('',(#27814,#27815,#27816,#27817,#27818));
#4544=EDGE_LOOP('',(#27819,#27820,#27821,#27822,#27823));
#4545=EDGE_LOOP('',(#27824,#27825,#27826,#27827,#27828,#27829));
#4546=EDGE_LOOP('',(#27830,#27831,#27832,#27833,#27834,#27835));
#4547=EDGE_LOOP('',(#27836,#27837,#27838,#27839));
#4548=EDGE_LOOP('',(#27840,#27841,#27842,#27843));
#4549=EDGE_LOOP('',(#27844,#27845,#27846,#27847));
#4550=EDGE_LOOP('',(#27848,#27849,#27850,#27851));
#4551=EDGE_LOOP('',(#27852,#27853,#27854,#27855));
#4552=EDGE_LOOP('',(#27856,#27857,#27858,#27859));
#4553=EDGE_LOOP('',(#27860,#27861,#27862,#27863));
#4554=EDGE_LOOP('',(#27864,#27865,#27866,#27867,#27868));
#4555=EDGE_LOOP('',(#27869,#27870,#27871,#27872,#27873));
#4556=EDGE_LOOP('',(#27874,#27875,#27876,#27877));
#4557=EDGE_LOOP('',(#27878,#27879,#27880,#27881));
#4558=EDGE_LOOP('',(#27882,#27883,#27884,#27885,#27886,#27887));
#4559=EDGE_LOOP('',(#27888,#27889,#27890,#27891,#27892,#27893));
#4560=EDGE_LOOP('',(#27894,#27895,#27896,#27897,#27898,#27899,#27900,#27901,
#27902,#27903,#27904,#27905,#27906,#27907,#27908,#27909));
#4561=EDGE_LOOP('',(#27910,#27911,#27912,#27913,#27914,#27915,#27916,#27917,
#27918,#27919,#27920,#27921,#27922,#27923,#27924,#27925));
#4562=EDGE_LOOP('',(#27926,#27927,#27928,#27929));
#4563=EDGE_LOOP('',(#27930,#27931,#27932,#27933));
#4564=EDGE_LOOP('',(#27934,#27935,#27936,#27937));
#4565=EDGE_LOOP('',(#27938,#27939,#27940,#27941));
#4566=EDGE_LOOP('',(#27942,#27943,#27944,#27945));
#4567=EDGE_LOOP('',(#27946));
#4568=EDGE_LOOP('',(#27947,#27948,#27949,#27950));
#4569=EDGE_LOOP('',(#27951,#27952,#27953,#27954));
#4570=EDGE_LOOP('',(#27955,#27956,#27957,#27958));
#4571=EDGE_LOOP('',(#27959,#27960,#27961,#27962));
#4572=EDGE_LOOP('',(#27963,#27964,#27965,#27966));
#4573=EDGE_LOOP('',(#27967,#27968,#27969,#27970));
#4574=EDGE_LOOP('',(#27971,#27972,#27973,#27974));
#4575=EDGE_LOOP('',(#27975));
#4576=EDGE_LOOP('',(#27976,#27977,#27978,#27979));
#4577=EDGE_LOOP('',(#27980,#27981,#27982,#27983));
#4578=EDGE_LOOP('',(#27984,#27985,#27986,#27987,#27988,#27989));
#4579=EDGE_LOOP('',(#27990,#27991,#27992,#27993,#27994,#27995));
#4580=EDGE_LOOP('',(#27996,#27997,#27998,#27999,#28000,#28001,#28002,#28003,
#28004,#28005,#28006,#28007,#28008,#28009,#28010,#28011));
#4581=EDGE_LOOP('',(#28012,#28013,#28014,#28015,#28016,#28017,#28018,#28019,
#28020,#28021,#28022,#28023,#28024,#28025,#28026,#28027));
#4582=EDGE_LOOP('',(#28028,#28029,#28030,#28031));
#4583=EDGE_LOOP('',(#28032,#28033,#28034,#28035));
#4584=EDGE_LOOP('',(#28036,#28037,#28038,#28039));
#4585=EDGE_LOOP('',(#28040,#28041,#28042,#28043));
#4586=EDGE_LOOP('',(#28044,#28045,#28046,#28047));
#4587=EDGE_LOOP('',(#28048));
#4588=EDGE_LOOP('',(#28049,#28050,#28051,#28052));
#4589=EDGE_LOOP('',(#28053,#28054,#28055,#28056));
#4590=EDGE_LOOP('',(#28057,#28058,#28059,#28060));
#4591=EDGE_LOOP('',(#28061,#28062,#28063,#28064));
#4592=EDGE_LOOP('',(#28065,#28066,#28067,#28068));
#4593=EDGE_LOOP('',(#28069,#28070,#28071,#28072));
#4594=EDGE_LOOP('',(#28073,#28074,#28075,#28076));
#4595=EDGE_LOOP('',(#28077));
#4596=EDGE_LOOP('',(#28078,#28079,#28080,#28081));
#4597=EDGE_LOOP('',(#28082,#28083,#28084,#28085));
#4598=EDGE_LOOP('',(#28086,#28087,#28088,#28089,#28090,#28091));
#4599=EDGE_LOOP('',(#28092,#28093,#28094,#28095,#28096,#28097));
#4600=EDGE_LOOP('',(#28098,#28099,#28100,#28101,#28102,#28103,#28104,#28105,
#28106,#28107,#28108,#28109,#28110,#28111,#28112,#28113));
#4601=EDGE_LOOP('',(#28114,#28115,#28116,#28117,#28118,#28119,#28120,#28121,
#28122,#28123,#28124,#28125,#28126,#28127,#28128,#28129));
#4602=EDGE_LOOP('',(#28130,#28131,#28132,#28133));
#4603=EDGE_LOOP('',(#28134,#28135,#28136,#28137));
#4604=EDGE_LOOP('',(#28138,#28139,#28140,#28141));
#4605=EDGE_LOOP('',(#28142,#28143,#28144,#28145));
#4606=EDGE_LOOP('',(#28146,#28147,#28148,#28149));
#4607=EDGE_LOOP('',(#28150));
#4608=EDGE_LOOP('',(#28151,#28152,#28153,#28154));
#4609=EDGE_LOOP('',(#28155,#28156,#28157,#28158));
#4610=EDGE_LOOP('',(#28159,#28160,#28161,#28162));
#4611=EDGE_LOOP('',(#28163,#28164,#28165,#28166));
#4612=EDGE_LOOP('',(#28167,#28168,#28169,#28170));
#4613=EDGE_LOOP('',(#28171,#28172,#28173,#28174));
#4614=EDGE_LOOP('',(#28175,#28176,#28177,#28178));
#4615=EDGE_LOOP('',(#28179));
#4616=EDGE_LOOP('',(#28180,#28181,#28182,#28183));
#4617=EDGE_LOOP('',(#28184,#28185,#28186,#28187));
#4618=EDGE_LOOP('',(#28188,#28189,#28190,#28191,#28192,#28193));
#4619=EDGE_LOOP('',(#28194,#28195,#28196,#28197,#28198,#28199));
#4620=EDGE_LOOP('',(#28200,#28201,#28202,#28203,#28204,#28205,#28206,#28207,
#28208,#28209,#28210,#28211,#28212,#28213,#28214,#28215));
#4621=EDGE_LOOP('',(#28216,#28217,#28218,#28219,#28220,#28221,#28222,#28223,
#28224,#28225,#28226,#28227,#28228,#28229,#28230,#28231));
#4622=EDGE_LOOP('',(#28232,#28233,#28234,#28235));
#4623=EDGE_LOOP('',(#28236,#28237,#28238,#28239));
#4624=EDGE_LOOP('',(#28240,#28241,#28242,#28243));
#4625=EDGE_LOOP('',(#28244,#28245,#28246,#28247));
#4626=EDGE_LOOP('',(#28248,#28249,#28250,#28251));
#4627=EDGE_LOOP('',(#28252));
#4628=EDGE_LOOP('',(#28253,#28254,#28255,#28256));
#4629=EDGE_LOOP('',(#28257,#28258,#28259,#28260));
#4630=EDGE_LOOP('',(#28261,#28262,#28263,#28264));
#4631=EDGE_LOOP('',(#28265,#28266,#28267,#28268));
#4632=EDGE_LOOP('',(#28269,#28270,#28271,#28272));
#4633=EDGE_LOOP('',(#28273,#28274,#28275,#28276));
#4634=EDGE_LOOP('',(#28277,#28278,#28279,#28280));
#4635=EDGE_LOOP('',(#28281));
#4636=EDGE_LOOP('',(#28282));
#4637=EDGE_LOOP('',(#28283,#28284,#28285,#28286,#28287,#28288,#28289,#28290,
#28291,#28292));
#4638=EDGE_LOOP('',(#28293,#28294,#28295,#28296,#28297,#28298,#28299,#28300));
#4639=EDGE_LOOP('',(#28301,#28302,#28303,#28304,#28305,#28306,#28307,#28308));
#4640=EDGE_LOOP('',(#28309,#28310,#28311,#28312,#28313,#28314,#28315,#28316));
#4641=EDGE_LOOP('',(#28317,#28318,#28319,#28320,#28321,#28322,#28323,#28324));
#4642=EDGE_LOOP('',(#28325,#28326,#28327,#28328,#28329,#28330,#28331,#28332));
#4643=EDGE_LOOP('',(#28333,#28334,#28335,#28336,#28337,#28338,#28339,#28340,
#28341,#28342));
#4644=EDGE_LOOP('',(#28343,#28344,#28345,#28346,#28347,#28348,#28349,#28350));
#4645=EDGE_LOOP('',(#28351,#28352,#28353,#28354,#28355,#28356,#28357,#28358));
#4646=EDGE_LOOP('',(#28359,#28360,#28361,#28362,#28363,#28364,#28365,#28366));
#4647=EDGE_LOOP('',(#28367,#28368,#28369,#28370,#28371,#28372,#28373,#28374));
#4648=EDGE_LOOP('',(#28375,#28376,#28377,#28378,#28379,#28380,#28381,#28382));
#4649=EDGE_LOOP('',(#28383,#28384,#28385,#28386,#28387,#28388,#28389,#28390,
#28391,#28392));
#4650=EDGE_LOOP('',(#28393,#28394,#28395,#28396,#28397,#28398,#28399,#28400));
#4651=EDGE_LOOP('',(#28401,#28402,#28403,#28404,#28405,#28406,#28407,#28408));
#4652=EDGE_LOOP('',(#28409,#28410,#28411,#28412,#28413,#28414,#28415,#28416));
#4653=EDGE_LOOP('',(#28417,#28418,#28419,#28420,#28421,#28422,#28423,#28424));
#4654=EDGE_LOOP('',(#28425,#28426,#28427,#28428,#28429,#28430,#28431,#28432));
#4655=EDGE_LOOP('',(#28433,#28434,#28435,#28436));
#4656=EDGE_LOOP('',(#28437,#28438,#28439,#28440));
#4657=EDGE_LOOP('',(#28441,#28442,#28443,#28444));
#4658=EDGE_LOOP('',(#28445,#28446,#28447,#28448));
#4659=EDGE_LOOP('',(#28449,#28450,#28451,#28452));
#4660=EDGE_LOOP('',(#28453,#28454,#28455,#28456));
#4661=EDGE_LOOP('',(#28457,#28458,#28459,#28460));
#4662=EDGE_LOOP('',(#28461,#28462,#28463,#28464));
#4663=EDGE_LOOP('',(#28465,#28466,#28467,#28468));
#4664=EDGE_LOOP('',(#28469,#28470,#28471,#28472));
#4665=EDGE_LOOP('',(#28473,#28474,#28475,#28476));
#4666=EDGE_LOOP('',(#28477,#28478,#28479,#28480));
#4667=EDGE_LOOP('',(#28481,#28482,#28483,#28484));
#4668=EDGE_LOOP('',(#28485,#28486,#28487,#28488));
#4669=EDGE_LOOP('',(#28489,#28490,#28491,#28492));
#4670=EDGE_LOOP('',(#28493,#28494,#28495,#28496));
#4671=EDGE_LOOP('',(#28497,#28498,#28499,#28500));
#4672=EDGE_LOOP('',(#28501,#28502,#28503,#28504));
#4673=EDGE_LOOP('',(#28505,#28506,#28507,#28508));
#4674=EDGE_LOOP('',(#28509,#28510,#28511,#28512));
#4675=EDGE_LOOP('',(#28513,#28514,#28515,#28516));
#4676=EDGE_LOOP('',(#28517,#28518,#28519,#28520));
#4677=EDGE_LOOP('',(#28521,#28522,#28523,#28524));
#4678=EDGE_LOOP('',(#28525,#28526,#28527,#28528));
#4679=EDGE_LOOP('',(#28529,#28530,#28531,#28532));
#4680=EDGE_LOOP('',(#28533,#28534,#28535,#28536));
#4681=EDGE_LOOP('',(#28537,#28538,#28539,#28540));
#4682=EDGE_LOOP('',(#28541,#28542,#28543,#28544));
#4683=EDGE_LOOP('',(#28545,#28546,#28547,#28548));
#4684=EDGE_LOOP('',(#28549,#28550,#28551,#28552));
#4685=EDGE_LOOP('',(#28553,#28554,#28555,#28556));
#4686=EDGE_LOOP('',(#28557,#28558,#28559,#28560));
#4687=EDGE_LOOP('',(#28561,#28562,#28563,#28564));
#4688=EDGE_LOOP('',(#28565,#28566,#28567,#28568));
#4689=EDGE_LOOP('',(#28569,#28570,#28571,#28572));
#4690=EDGE_LOOP('',(#28573,#28574,#28575,#28576));
#4691=EDGE_LOOP('',(#28577,#28578,#28579,#28580));
#4692=EDGE_LOOP('',(#28581,#28582,#28583,#28584));
#4693=EDGE_LOOP('',(#28585,#28586,#28587,#28588));
#4694=EDGE_LOOP('',(#28589,#28590,#28591,#28592));
#4695=EDGE_LOOP('',(#28593,#28594,#28595,#28596));
#4696=EDGE_LOOP('',(#28597,#28598,#28599,#28600));
#4697=EDGE_LOOP('',(#28601,#28602,#28603,#28604));
#4698=EDGE_LOOP('',(#28605,#28606,#28607,#28608));
#4699=EDGE_LOOP('',(#28609,#28610,#28611,#28612));
#4700=EDGE_LOOP('',(#28613,#28614,#28615,#28616));
#4701=EDGE_LOOP('',(#28617,#28618,#28619,#28620));
#4702=EDGE_LOOP('',(#28621,#28622,#28623,#28624));
#4703=EDGE_LOOP('',(#28625,#28626,#28627,#28628));
#4704=EDGE_LOOP('',(#28629,#28630,#28631,#28632));
#4705=EDGE_LOOP('',(#28633,#28634,#28635,#28636));
#4706=EDGE_LOOP('',(#28637,#28638,#28639,#28640));
#4707=EDGE_LOOP('',(#28641,#28642,#28643,#28644));
#4708=EDGE_LOOP('',(#28645,#28646,#28647,#28648));
#4709=EDGE_LOOP('',(#28649,#28650,#28651,#28652));
#4710=EDGE_LOOP('',(#28653,#28654,#28655,#28656));
#4711=EDGE_LOOP('',(#28657,#28658,#28659,#28660));
#4712=EDGE_LOOP('',(#28661,#28662,#28663,#28664));
#4713=EDGE_LOOP('',(#28665,#28666,#28667,#28668));
#4714=EDGE_LOOP('',(#28669,#28670,#28671,#28672));
#4715=EDGE_LOOP('',(#28673,#28674,#28675,#28676));
#4716=EDGE_LOOP('',(#28677,#28678,#28679,#28680));
#4717=EDGE_LOOP('',(#28681,#28682,#28683,#28684));
#4718=EDGE_LOOP('',(#28685,#28686,#28687,#28688));
#4719=EDGE_LOOP('',(#28689,#28690,#28691,#28692));
#4720=EDGE_LOOP('',(#28693,#28694,#28695,#28696));
#4721=EDGE_LOOP('',(#28697,#28698,#28699,#28700));
#4722=EDGE_LOOP('',(#28701,#28702,#28703,#28704));
#4723=EDGE_LOOP('',(#28705,#28706,#28707,#28708));
#4724=EDGE_LOOP('',(#28709,#28710,#28711,#28712));
#4725=EDGE_LOOP('',(#28713,#28714,#28715,#28716));
#4726=EDGE_LOOP('',(#28717,#28718,#28719,#28720));
#4727=EDGE_LOOP('',(#28721,#28722,#28723,#28724));
#4728=EDGE_LOOP('',(#28725,#28726,#28727,#28728));
#4729=EDGE_LOOP('',(#28729,#28730,#28731,#28732));
#4730=EDGE_LOOP('',(#28733,#28734,#28735,#28736));
#4731=EDGE_LOOP('',(#28737,#28738,#28739,#28740));
#4732=EDGE_LOOP('',(#28741,#28742,#28743,#28744));
#4733=EDGE_LOOP('',(#28745,#28746,#28747,#28748));
#4734=EDGE_LOOP('',(#28749,#28750,#28751,#28752));
#4735=EDGE_LOOP('',(#28753,#28754,#28755,#28756));
#4736=EDGE_LOOP('',(#28757,#28758,#28759,#28760));
#4737=EDGE_LOOP('',(#28761,#28762,#28763,#28764));
#4738=EDGE_LOOP('',(#28765,#28766,#28767,#28768));
#4739=EDGE_LOOP('',(#28769,#28770,#28771,#28772));
#4740=EDGE_LOOP('',(#28773,#28774,#28775,#28776));
#4741=EDGE_LOOP('',(#28777,#28778,#28779,#28780));
#4742=EDGE_LOOP('',(#28781,#28782,#28783,#28784));
#4743=EDGE_LOOP('',(#28785,#28786,#28787,#28788));
#4744=EDGE_LOOP('',(#28789,#28790,#28791,#28792));
#4745=EDGE_LOOP('',(#28793,#28794,#28795,#28796));
#4746=EDGE_LOOP('',(#28797,#28798,#28799,#28800));
#4747=EDGE_LOOP('',(#28801,#28802,#28803,#28804));
#4748=EDGE_LOOP('',(#28805,#28806,#28807,#28808));
#4749=EDGE_LOOP('',(#28809,#28810,#28811,#28812));
#4750=EDGE_LOOP('',(#28813,#28814,#28815,#28816));
#4751=EDGE_LOOP('',(#28817,#28818,#28819,#28820));
#4752=EDGE_LOOP('',(#28821,#28822,#28823,#28824));
#4753=EDGE_LOOP('',(#28825,#28826,#28827,#28828));
#4754=EDGE_LOOP('',(#28829,#28830,#28831,#28832));
#4755=EDGE_LOOP('',(#28833,#28834,#28835,#28836));
#4756=EDGE_LOOP('',(#28837,#28838,#28839,#28840));
#4757=EDGE_LOOP('',(#28841,#28842,#28843,#28844));
#4758=EDGE_LOOP('',(#28845,#28846,#28847,#28848));
#4759=EDGE_LOOP('',(#28849,#28850,#28851,#28852));
#4760=EDGE_LOOP('',(#28853,#28854,#28855,#28856));
#4761=EDGE_LOOP('',(#28857,#28858,#28859,#28860));
#4762=EDGE_LOOP('',(#28861,#28862,#28863,#28864));
#4763=EDGE_LOOP('',(#28865,#28866,#28867,#28868));
#4764=EDGE_LOOP('',(#28869,#28870,#28871,#28872));
#4765=EDGE_LOOP('',(#28873,#28874,#28875,#28876));
#4766=EDGE_LOOP('',(#28877,#28878,#28879,#28880));
#4767=EDGE_LOOP('',(#28881,#28882,#28883,#28884));
#4768=EDGE_LOOP('',(#28885,#28886,#28887,#28888));
#4769=EDGE_LOOP('',(#28889,#28890,#28891,#28892));
#4770=EDGE_LOOP('',(#28893,#28894,#28895,#28896));
#4771=EDGE_LOOP('',(#28897,#28898,#28899,#28900));
#4772=EDGE_LOOP('',(#28901,#28902,#28903,#28904));
#4773=EDGE_LOOP('',(#28905,#28906,#28907,#28908));
#4774=EDGE_LOOP('',(#28909,#28910,#28911,#28912));
#4775=EDGE_LOOP('',(#28913,#28914,#28915,#28916));
#4776=EDGE_LOOP('',(#28917,#28918,#28919,#28920));
#4777=EDGE_LOOP('',(#28921,#28922,#28923,#28924));
#4778=EDGE_LOOP('',(#28925,#28926,#28927,#28928));
#4779=EDGE_LOOP('',(#28929,#28930,#28931,#28932));
#4780=EDGE_LOOP('',(#28933,#28934,#28935,#28936));
#4781=EDGE_LOOP('',(#28937,#28938,#28939,#28940));
#4782=EDGE_LOOP('',(#28941,#28942,#28943,#28944));
#4783=EDGE_LOOP('',(#28945,#28946,#28947,#28948));
#4784=EDGE_LOOP('',(#28949,#28950,#28951,#28952));
#4785=EDGE_LOOP('',(#28953,#28954,#28955,#28956));
#4786=EDGE_LOOP('',(#28957,#28958,#28959,#28960));
#4787=EDGE_LOOP('',(#28961,#28962,#28963,#28964));
#4788=EDGE_LOOP('',(#28965,#28966,#28967,#28968));
#4789=EDGE_LOOP('',(#28969,#28970,#28971,#28972));
#4790=EDGE_LOOP('',(#28973,#28974,#28975,#28976));
#4791=EDGE_LOOP('',(#28977,#28978,#28979,#28980));
#4792=EDGE_LOOP('',(#28981,#28982,#28983,#28984));
#4793=EDGE_LOOP('',(#28985,#28986,#28987,#28988));
#4794=EDGE_LOOP('',(#28989,#28990,#28991,#28992));
#4795=EDGE_LOOP('',(#28993,#28994,#28995,#28996));
#4796=EDGE_LOOP('',(#28997,#28998,#28999,#29000));
#4797=EDGE_LOOP('',(#29001,#29002,#29003,#29004));
#4798=EDGE_LOOP('',(#29005,#29006,#29007,#29008));
#4799=EDGE_LOOP('',(#29009,#29010,#29011,#29012));
#4800=EDGE_LOOP('',(#29013,#29014,#29015,#29016));
#4801=EDGE_LOOP('',(#29017,#29018,#29019,#29020));
#4802=EDGE_LOOP('',(#29021,#29022,#29023,#29024));
#4803=EDGE_LOOP('',(#29025,#29026,#29027,#29028));
#4804=EDGE_LOOP('',(#29029,#29030,#29031,#29032));
#4805=EDGE_LOOP('',(#29033,#29034,#29035,#29036));
#4806=EDGE_LOOP('',(#29037,#29038,#29039,#29040));
#4807=EDGE_LOOP('',(#29041,#29042,#29043,#29044));
#4808=EDGE_LOOP('',(#29045,#29046,#29047,#29048));
#4809=EDGE_LOOP('',(#29049,#29050,#29051,#29052));
#4810=EDGE_LOOP('',(#29053,#29054,#29055,#29056));
#4811=EDGE_LOOP('',(#29057,#29058,#29059,#29060));
#4812=EDGE_LOOP('',(#29061,#29062,#29063,#29064));
#4813=EDGE_LOOP('',(#29065,#29066,#29067,#29068));
#4814=EDGE_LOOP('',(#29069,#29070,#29071,#29072));
#4815=EDGE_LOOP('',(#29073,#29074,#29075,#29076));
#4816=EDGE_LOOP('',(#29077,#29078,#29079,#29080));
#4817=EDGE_LOOP('',(#29081,#29082,#29083,#29084));
#4818=EDGE_LOOP('',(#29085,#29086,#29087,#29088));
#4819=EDGE_LOOP('',(#29089,#29090,#29091,#29092));
#4820=EDGE_LOOP('',(#29093,#29094,#29095,#29096));
#4821=EDGE_LOOP('',(#29097,#29098,#29099,#29100));
#4822=EDGE_LOOP('',(#29101,#29102,#29103,#29104));
#4823=EDGE_LOOP('',(#29105,#29106,#29107,#29108));
#4824=EDGE_LOOP('',(#29109,#29110,#29111,#29112));
#4825=EDGE_LOOP('',(#29113,#29114,#29115,#29116));
#4826=EDGE_LOOP('',(#29117,#29118,#29119,#29120));
#4827=EDGE_LOOP('',(#29121,#29122,#29123,#29124));
#4828=EDGE_LOOP('',(#29125,#29126,#29127,#29128));
#4829=EDGE_LOOP('',(#29129,#29130,#29131,#29132));
#4830=EDGE_LOOP('',(#29133,#29134,#29135,#29136));
#4831=EDGE_LOOP('',(#29137,#29138,#29139,#29140));
#4832=EDGE_LOOP('',(#29141,#29142,#29143,#29144));
#4833=EDGE_LOOP('',(#29145,#29146,#29147,#29148));
#4834=EDGE_LOOP('',(#29149,#29150,#29151,#29152));
#4835=EDGE_LOOP('',(#29153,#29154,#29155,#29156));
#4836=EDGE_LOOP('',(#29157,#29158,#29159,#29160));
#4837=EDGE_LOOP('',(#29161,#29162,#29163,#29164));
#4838=EDGE_LOOP('',(#29165,#29166,#29167,#29168));
#4839=EDGE_LOOP('',(#29169,#29170,#29171,#29172));
#4840=EDGE_LOOP('',(#29173,#29174,#29175,#29176));
#4841=EDGE_LOOP('',(#29177,#29178,#29179,#29180));
#4842=EDGE_LOOP('',(#29181,#29182,#29183,#29184));
#4843=EDGE_LOOP('',(#29185,#29186,#29187,#29188));
#4844=EDGE_LOOP('',(#29189,#29190,#29191,#29192));
#4845=EDGE_LOOP('',(#29193,#29194,#29195,#29196));
#4846=EDGE_LOOP('',(#29197,#29198,#29199,#29200));
#4847=EDGE_LOOP('',(#29201,#29202,#29203,#29204));
#4848=EDGE_LOOP('',(#29205,#29206,#29207,#29208));
#4849=EDGE_LOOP('',(#29209,#29210,#29211,#29212));
#4850=EDGE_LOOP('',(#29213,#29214,#29215,#29216));
#4851=EDGE_LOOP('',(#29217,#29218,#29219,#29220));
#4852=EDGE_LOOP('',(#29221,#29222,#29223,#29224));
#4853=EDGE_LOOP('',(#29225,#29226,#29227,#29228));
#4854=EDGE_LOOP('',(#29229,#29230,#29231,#29232));
#4855=EDGE_LOOP('',(#29233,#29234,#29235,#29236));
#4856=EDGE_LOOP('',(#29237,#29238,#29239,#29240));
#4857=EDGE_LOOP('',(#29241,#29242,#29243,#29244));
#4858=EDGE_LOOP('',(#29245,#29246,#29247,#29248));
#4859=EDGE_LOOP('',(#29249,#29250,#29251,#29252));
#4860=EDGE_LOOP('',(#29253,#29254,#29255,#29256));
#4861=EDGE_LOOP('',(#29257,#29258,#29259,#29260));
#4862=EDGE_LOOP('',(#29261,#29262,#29263,#29264));
#4863=EDGE_LOOP('',(#29265,#29266,#29267,#29268));
#4864=EDGE_LOOP('',(#29269,#29270,#29271,#29272));
#4865=EDGE_LOOP('',(#29273,#29274,#29275,#29276));
#4866=EDGE_LOOP('',(#29277,#29278,#29279,#29280));
#4867=EDGE_LOOP('',(#29281,#29282,#29283,#29284));
#4868=EDGE_LOOP('',(#29285,#29286,#29287,#29288));
#4869=EDGE_LOOP('',(#29289,#29290,#29291,#29292));
#4870=EDGE_LOOP('',(#29293,#29294,#29295,#29296));
#4871=EDGE_LOOP('',(#29297,#29298,#29299,#29300));
#4872=EDGE_LOOP('',(#29301,#29302,#29303,#29304));
#4873=EDGE_LOOP('',(#29305,#29306,#29307,#29308));
#4874=EDGE_LOOP('',(#29309,#29310,#29311,#29312));
#4875=EDGE_LOOP('',(#29313,#29314,#29315,#29316));
#4876=EDGE_LOOP('',(#29317,#29318,#29319,#29320));
#4877=EDGE_LOOP('',(#29321,#29322,#29323,#29324));
#4878=EDGE_LOOP('',(#29325,#29326,#29327,#29328));
#4879=EDGE_LOOP('',(#29329,#29330,#29331,#29332));
#4880=EDGE_LOOP('',(#29333,#29334,#29335,#29336));
#4881=EDGE_LOOP('',(#29337,#29338,#29339,#29340));
#4882=EDGE_LOOP('',(#29341,#29342,#29343,#29344));
#4883=EDGE_LOOP('',(#29345,#29346,#29347,#29348));
#4884=EDGE_LOOP('',(#29349,#29350,#29351,#29352));
#4885=EDGE_LOOP('',(#29353,#29354,#29355,#29356));
#4886=EDGE_LOOP('',(#29357,#29358,#29359,#29360));
#4887=EDGE_LOOP('',(#29361,#29362,#29363,#29364));
#4888=EDGE_LOOP('',(#29365,#29366,#29367,#29368));
#4889=EDGE_LOOP('',(#29369,#29370,#29371,#29372));
#4890=EDGE_LOOP('',(#29373,#29374,#29375,#29376));
#4891=EDGE_LOOP('',(#29377,#29378,#29379,#29380));
#4892=EDGE_LOOP('',(#29381,#29382,#29383,#29384));
#4893=EDGE_LOOP('',(#29385,#29386,#29387,#29388));
#4894=EDGE_LOOP('',(#29389,#29390,#29391,#29392));
#4895=EDGE_LOOP('',(#29393,#29394,#29395,#29396));
#4896=EDGE_LOOP('',(#29397,#29398,#29399,#29400));
#4897=EDGE_LOOP('',(#29401,#29402,#29403,#29404));
#4898=EDGE_LOOP('',(#29405,#29406,#29407,#29408));
#4899=EDGE_LOOP('',(#29409,#29410,#29411,#29412));
#4900=EDGE_LOOP('',(#29413,#29414,#29415,#29416));
#4901=EDGE_LOOP('',(#29417,#29418,#29419,#29420));
#4902=EDGE_LOOP('',(#29421,#29422,#29423,#29424));
#4903=EDGE_LOOP('',(#29425,#29426,#29427,#29428));
#4904=EDGE_LOOP('',(#29429,#29430,#29431,#29432));
#4905=EDGE_LOOP('',(#29433,#29434,#29435,#29436));
#4906=EDGE_LOOP('',(#29437,#29438,#29439,#29440));
#4907=EDGE_LOOP('',(#29441,#29442,#29443,#29444));
#4908=EDGE_LOOP('',(#29445,#29446,#29447,#29448));
#4909=EDGE_LOOP('',(#29449,#29450,#29451,#29452));
#4910=EDGE_LOOP('',(#29453,#29454,#29455,#29456));
#4911=EDGE_LOOP('',(#29457,#29458,#29459,#29460));
#4912=EDGE_LOOP('',(#29461,#29462,#29463,#29464));
#4913=EDGE_LOOP('',(#29465,#29466,#29467,#29468));
#4914=EDGE_LOOP('',(#29469,#29470,#29471,#29472));
#4915=EDGE_LOOP('',(#29473,#29474,#29475,#29476));
#4916=EDGE_LOOP('',(#29477,#29478,#29479,#29480));
#4917=EDGE_LOOP('',(#29481,#29482,#29483,#29484));
#4918=EDGE_LOOP('',(#29485,#29486,#29487,#29488));
#4919=EDGE_LOOP('',(#29489,#29490,#29491,#29492));
#4920=EDGE_LOOP('',(#29493,#29494,#29495,#29496));
#4921=EDGE_LOOP('',(#29497,#29498,#29499,#29500));
#4922=EDGE_LOOP('',(#29501,#29502,#29503,#29504));
#4923=EDGE_LOOP('',(#29505,#29506,#29507,#29508));
#4924=EDGE_LOOP('',(#29509,#29510,#29511,#29512));
#4925=EDGE_LOOP('',(#29513,#29514,#29515,#29516));
#4926=EDGE_LOOP('',(#29517,#29518,#29519,#29520));
#4927=EDGE_LOOP('',(#29521,#29522,#29523,#29524));
#4928=EDGE_LOOP('',(#29525,#29526,#29527,#29528));
#4929=EDGE_LOOP('',(#29529,#29530,#29531,#29532));
#4930=EDGE_LOOP('',(#29533,#29534,#29535,#29536));
#4931=EDGE_LOOP('',(#29537,#29538,#29539,#29540));
#4932=EDGE_LOOP('',(#29541,#29542,#29543,#29544,#29545,#29546));
#4933=EDGE_LOOP('',(#29547,#29548,#29549,#29550,#29551,#29552));
#4934=EDGE_LOOP('',(#29553,#29554,#29555,#29556,#29557,#29558,#29559,#29560,
#29561,#29562,#29563,#29564,#29565,#29566,#29567,#29568));
#4935=EDGE_LOOP('',(#29569,#29570,#29571,#29572,#29573,#29574,#29575,#29576,
#29577,#29578,#29579,#29580,#29581,#29582,#29583,#29584));
#4936=EDGE_LOOP('',(#29585,#29586,#29587,#29588));
#4937=EDGE_LOOP('',(#29589,#29590,#29591,#29592));
#4938=EDGE_LOOP('',(#29593,#29594,#29595,#29596));
#4939=EDGE_LOOP('',(#29597,#29598,#29599,#29600));
#4940=EDGE_LOOP('',(#29601,#29602,#29603,#29604));
#4941=EDGE_LOOP('',(#29605));
#4942=EDGE_LOOP('',(#29606,#29607,#29608,#29609));
#4943=EDGE_LOOP('',(#29610,#29611,#29612,#29613));
#4944=EDGE_LOOP('',(#29614,#29615,#29616,#29617));
#4945=EDGE_LOOP('',(#29618,#29619,#29620,#29621));
#4946=EDGE_LOOP('',(#29622,#29623,#29624,#29625));
#4947=EDGE_LOOP('',(#29626,#29627,#29628,#29629));
#4948=EDGE_LOOP('',(#29630,#29631,#29632,#29633));
#4949=EDGE_LOOP('',(#29634));
#4950=EDGE_LOOP('',(#29635,#29636,#29637,#29638));
#4951=EDGE_LOOP('',(#29639,#29640,#29641,#29642));
#4952=EDGE_LOOP('',(#29643,#29644,#29645,#29646,#29647,#29648));
#4953=EDGE_LOOP('',(#29649,#29650,#29651,#29652,#29653,#29654));
#4954=EDGE_LOOP('',(#29655,#29656,#29657,#29658,#29659,#29660,#29661,#29662,
#29663,#29664,#29665,#29666,#29667,#29668,#29669,#29670));
#4955=EDGE_LOOP('',(#29671,#29672,#29673,#29674,#29675,#29676,#29677,#29678,
#29679,#29680,#29681,#29682,#29683,#29684,#29685,#29686));
#4956=EDGE_LOOP('',(#29687,#29688,#29689,#29690));
#4957=EDGE_LOOP('',(#29691,#29692,#29693,#29694));
#4958=EDGE_LOOP('',(#29695,#29696,#29697,#29698));
#4959=EDGE_LOOP('',(#29699,#29700,#29701,#29702));
#4960=EDGE_LOOP('',(#29703,#29704,#29705,#29706));
#4961=EDGE_LOOP('',(#29707));
#4962=EDGE_LOOP('',(#29708,#29709,#29710,#29711));
#4963=EDGE_LOOP('',(#29712,#29713,#29714,#29715));
#4964=EDGE_LOOP('',(#29716,#29717,#29718,#29719));
#4965=EDGE_LOOP('',(#29720,#29721,#29722,#29723));
#4966=EDGE_LOOP('',(#29724,#29725,#29726,#29727));
#4967=EDGE_LOOP('',(#29728,#29729,#29730,#29731));
#4968=EDGE_LOOP('',(#29732,#29733,#29734,#29735));
#4969=EDGE_LOOP('',(#29736));
#4970=EDGE_LOOP('',(#29737,#29738,#29739,#29740));
#4971=EDGE_LOOP('',(#29741,#29742,#29743,#29744));
#4972=EDGE_LOOP('',(#29745,#29746,#29747,#29748));
#4973=EDGE_LOOP('',(#29749,#29750,#29751,#29752));
#4974=EDGE_LOOP('',(#29753,#29754,#29755,#29756));
#4975=EDGE_LOOP('',(#29757,#29758,#29759,#29760));
#4976=EDGE_LOOP('',(#29761,#29762,#29763,#29764));
#4977=EDGE_LOOP('',(#29765,#29766,#29767,#29768));
#4978=EDGE_LOOP('',(#29769,#29770,#29771,#29772));
#4979=EDGE_LOOP('',(#29773,#29774,#29775,#29776));
#4980=EDGE_LOOP('',(#29777,#29778,#29779,#29780));
#4981=EDGE_LOOP('',(#29781,#29782,#29783,#29784));
#4982=EDGE_LOOP('',(#29785,#29786,#29787,#29788,#29789,#29790));
#4983=EDGE_LOOP('',(#29791,#29792,#29793,#29794,#29795,#29796));
#4984=EDGE_LOOP('',(#29797,#29798,#29799,#29800));
#4985=EDGE_LOOP('',(#29801,#29802,#29803,#29804));
#4986=EDGE_LOOP('',(#29805,#29806,#29807,#29808));
#4987=EDGE_LOOP('',(#29809,#29810,#29811,#29812));
#4988=EDGE_LOOP('',(#29813,#29814,#29815,#29816));
#4989=EDGE_LOOP('',(#29817,#29818,#29819,#29820));
#4990=EDGE_LOOP('',(#29821,#29822,#29823,#29824,#29825));
#4991=EDGE_LOOP('',(#29826,#29827,#29828,#29829,#29830));
#4992=EDGE_LOOP('',(#29831,#29832,#29833,#29834,#29835));
#4993=EDGE_LOOP('',(#29836,#29837,#29838,#29839));
#4994=EDGE_LOOP('',(#29840,#29841,#29842,#29843,#29844));
#4995=EDGE_LOOP('',(#29845,#29846,#29847,#29848,#29849,#29850,#29851,#29852,
#29853,#29854,#29855,#29856));
#4996=EDGE_LOOP('',(#29857,#29858,#29859,#29860));
#4997=EDGE_LOOP('',(#29861,#29862,#29863,#29864));
#4998=EDGE_LOOP('',(#29865,#29866,#29867,#29868));
#4999=EDGE_LOOP('',(#29869,#29870,#29871,#29872));
#5000=EDGE_LOOP('',(#29873,#29874,#29875,#29876,#29877,#29878));
#5001=EDGE_LOOP('',(#29879,#29880,#29881,#29882,#29883,#29884));
#5002=EDGE_LOOP('',(#29885,#29886,#29887,#29888));
#5003=EDGE_LOOP('',(#29889,#29890,#29891,#29892,#29893,#29894));
#5004=EDGE_LOOP('',(#29895,#29896,#29897,#29898));
#5005=EDGE_LOOP('',(#29899,#29900,#29901,#29902,#29903,#29904));
#5006=EDGE_LOOP('',(#29905,#29906,#29907,#29908));
#5007=EDGE_LOOP('',(#29909,#29910,#29911,#29912));
#5008=EDGE_LOOP('',(#29913,#29914,#29915,#29916,#29917,#29918));
#5009=EDGE_LOOP('',(#29919,#29920,#29921,#29922,#29923,#29924));
#5010=EDGE_LOOP('',(#29925,#29926,#29927,#29928));
#5011=EDGE_LOOP('',(#29929,#29930,#29931,#29932,#29933,#29934,#29935,#29936,
#29937,#29938,#29939,#29940));
#5012=EDGE_LOOP('',(#29941,#29942,#29943,#29944));
#5013=EDGE_LOOP('',(#29945,#29946,#29947,#29948));
#5014=EDGE_LOOP('',(#29949,#29950,#29951,#29952));
#5015=EDGE_LOOP('',(#29953,#29954,#29955,#29956,#29957,#29958,#29959,#29960));
#5016=EDGE_LOOP('',(#29961,#29962,#29963,#29964,#29965,#29966,#29967,#29968,
#29969,#29970,#29971,#29972));
#5017=EDGE_LOOP('',(#29973,#29974,#29975,#29976,#29977,#29978,#29979,#29980,
#29981,#29982,#29983,#29984));
#5018=EDGE_LOOP('',(#29985));
#5019=EDGE_LOOP('',(#29986));
#5020=EDGE_LOOP('',(#29987,#29988,#29989,#29990,#29991,#29992,#29993,#29994,
#29995,#29996,#29997,#29998));
#5021=EDGE_LOOP('',(#29999,#30000,#30001,#30002,#30003,#30004));
#5022=EDGE_LOOP('',(#30005,#30006,#30007,#30008));
#5023=EDGE_LOOP('',(#30009,#30010,#30011,#30012,#30013,#30014));
#5024=EDGE_LOOP('',(#30015,#30016,#30017,#30018));
#5025=EDGE_LOOP('',(#30019,#30020,#30021,#30022,#30023,#30024));
#5026=EDGE_LOOP('',(#30025,#30026,#30027,#30028));
#5027=EDGE_LOOP('',(#30029,#30030,#30031,#30032,#30033,#30034));
#5028=EDGE_LOOP('',(#30035,#30036,#30037,#30038));
#5029=EDGE_LOOP('',(#30039,#30040,#30041,#30042));
#5030=EDGE_LOOP('',(#30043,#30044,#30045,#30046));
#5031=EDGE_LOOP('',(#30047,#30048,#30049,#30050));
#5032=EDGE_LOOP('',(#30051,#30052,#30053,#30054,#30055,#30056));
#5033=EDGE_LOOP('',(#30057));
#5034=EDGE_LOOP('',(#30058,#30059,#30060,#30061));
#5035=EDGE_LOOP('',(#30062,#30063,#30064,#30065));
#5036=EDGE_LOOP('',(#30066,#30067,#30068,#30069,#30070,#30071));
#5037=EDGE_LOOP('',(#30072));
#5038=EDGE_LOOP('',(#30073,#30074,#30075,#30076));
#5039=EDGE_LOOP('',(#30077,#30078,#30079,#30080));
#5040=EDGE_LOOP('',(#30081,#30082,#30083,#30084));
#5041=EDGE_LOOP('',(#30085,#30086,#30087,#30088));
#5042=EDGE_LOOP('',(#30089,#30090,#30091,#30092));
#5043=EDGE_LOOP('',(#30093,#30094,#30095,#30096));
#5044=EDGE_LOOP('',(#30097,#30098,#30099,#30100));
#5045=EDGE_LOOP('',(#30101,#30102,#30103,#30104));
#5046=EDGE_LOOP('',(#30105,#30106,#30107,#30108));
#5047=EDGE_LOOP('',(#30109,#30110,#30111,#30112));
#5048=EDGE_LOOP('',(#30113,#30114,#30115,#30116));
#5049=EDGE_LOOP('',(#30117,#30118,#30119,#30120));
#5050=EDGE_LOOP('',(#30121,#30122,#30123,#30124));
#5051=EDGE_LOOP('',(#30125,#30126,#30127,#30128));
#5052=EDGE_LOOP('',(#30129,#30130,#30131,#30132));
#5053=EDGE_LOOP('',(#30133,#30134,#30135,#30136));
#5054=EDGE_LOOP('',(#30137,#30138,#30139,#30140));
#5055=EDGE_LOOP('',(#30141,#30142,#30143,#30144));
#5056=EDGE_LOOP('',(#30145,#30146,#30147,#30148));
#5057=EDGE_LOOP('',(#30149,#30150,#30151,#30152));
#5058=EDGE_LOOP('',(#30153,#30154,#30155,#30156));
#5059=EDGE_LOOP('',(#30157,#30158,#30159,#30160));
#5060=EDGE_LOOP('',(#30161,#30162,#30163,#30164));
#5061=EDGE_LOOP('',(#30165,#30166,#30167,#30168));
#5062=EDGE_LOOP('',(#30169,#30170,#30171,#30172));
#5063=EDGE_LOOP('',(#30173,#30174,#30175,#30176));
#5064=EDGE_LOOP('',(#30177,#30178,#30179,#30180));
#5065=EDGE_LOOP('',(#30181,#30182,#30183,#30184));
#5066=EDGE_LOOP('',(#30185,#30186,#30187,#30188));
#5067=EDGE_LOOP('',(#30189,#30190,#30191,#30192));
#5068=EDGE_LOOP('',(#30193,#30194,#30195,#30196));
#5069=EDGE_LOOP('',(#30197,#30198,#30199,#30200));
#5070=EDGE_LOOP('',(#30201,#30202,#30203,#30204));
#5071=EDGE_LOOP('',(#30205,#30206,#30207,#30208));
#5072=EDGE_LOOP('',(#30209,#30210,#30211,#30212));
#5073=EDGE_LOOP('',(#30213,#30214,#30215,#30216));
#5074=EDGE_LOOP('',(#30217,#30218,#30219,#30220));
#5075=EDGE_LOOP('',(#30221,#30222,#30223,#30224));
#5076=EDGE_LOOP('',(#30225,#30226,#30227,#30228));
#5077=EDGE_LOOP('',(#30229,#30230,#30231,#30232));
#5078=EDGE_LOOP('',(#30233,#30234,#30235,#30236));
#5079=EDGE_LOOP('',(#30237,#30238,#30239,#30240));
#5080=EDGE_LOOP('',(#30241,#30242,#30243,#30244));
#5081=EDGE_LOOP('',(#30245,#30246,#30247,#30248));
#5082=EDGE_LOOP('',(#30249,#30250,#30251,#30252));
#5083=EDGE_LOOP('',(#30253,#30254,#30255,#30256));
#5084=EDGE_LOOP('',(#30257,#30258,#30259,#30260));
#5085=EDGE_LOOP('',(#30261,#30262,#30263,#30264));
#5086=EDGE_LOOP('',(#30265,#30266,#30267,#30268));
#5087=EDGE_LOOP('',(#30269,#30270,#30271,#30272));
#5088=EDGE_LOOP('',(#30273,#30274,#30275,#30276));
#5089=EDGE_LOOP('',(#30277,#30278,#30279,#30280,#30281,#30282));
#5090=EDGE_LOOP('',(#30283));
#5091=EDGE_LOOP('',(#30284,#30285,#30286,#30287));
#5092=EDGE_LOOP('',(#30288,#30289,#30290,#30291,#30292,#30293));
#5093=EDGE_LOOP('',(#30294));
#5094=EDGE_LOOP('',(#30295,#30296,#30297,#30298));
#5095=EDGE_LOOP('',(#30299,#30300,#30301,#30302));
#5096=EDGE_LOOP('',(#30303,#30304,#30305,#30306));
#5097=EDGE_LOOP('',(#30307,#30308,#30309,#30310));
#5098=EDGE_LOOP('',(#30311,#30312,#30313,#30314));
#5099=EDGE_LOOP('',(#30315,#30316,#30317,#30318));
#5100=EDGE_LOOP('',(#30319,#30320,#30321,#30322));
#5101=EDGE_LOOP('',(#30323,#30324,#30325,#30326));
#5102=EDGE_LOOP('',(#30327,#30328,#30329,#30330));
#5103=EDGE_LOOP('',(#30331,#30332,#30333,#30334));
#5104=EDGE_LOOP('',(#30335,#30336,#30337,#30338));
#5105=EDGE_LOOP('',(#30339,#30340,#30341,#30342,#30343,#30344));
#5106=EDGE_LOOP('',(#30345));
#5107=EDGE_LOOP('',(#30346,#30347,#30348,#30349,#30350,#30351));
#5108=EDGE_LOOP('',(#30352));
#5109=EDGE_LOOP('',(#30353,#30354,#30355,#30356));
#5110=EDGE_LOOP('',(#30357,#30358,#30359,#30360));
#5111=EDGE_LOOP('',(#30361,#30362,#30363,#30364));
#5112=EDGE_LOOP('',(#30365,#30366,#30367,#30368));
#5113=EDGE_LOOP('',(#30369,#30370,#30371,#30372));
#5114=EDGE_LOOP('',(#30373,#30374,#30375,#30376));
#5115=EDGE_LOOP('',(#30377,#30378,#30379,#30380));
#5116=EDGE_LOOP('',(#30381,#30382,#30383,#30384));
#5117=EDGE_LOOP('',(#30385,#30386,#30387,#30388));
#5118=EDGE_LOOP('',(#30389,#30390,#30391,#30392));
#5119=EDGE_LOOP('',(#30393,#30394,#30395,#30396));
#5120=EDGE_LOOP('',(#30397,#30398,#30399,#30400,#30401,#30402));
#5121=EDGE_LOOP('',(#30403));
#5122=EDGE_LOOP('',(#30404,#30405,#30406,#30407,#30408,#30409));
#5123=EDGE_LOOP('',(#30410));
#5124=EDGE_LOOP('',(#30411,#30412,#30413,#30414));
#5125=EDGE_LOOP('',(#30415,#30416,#30417,#30418));
#5126=EDGE_LOOP('',(#30419,#30420,#30421,#30422));
#5127=EDGE_LOOP('',(#30423,#30424,#30425,#30426));
#5128=EDGE_LOOP('',(#30427,#30428,#30429,#30430));
#5129=EDGE_LOOP('',(#30431,#30432,#30433,#30434));
#5130=EDGE_LOOP('',(#30435,#30436,#30437,#30438));
#5131=EDGE_LOOP('',(#30439,#30440,#30441,#30442));
#5132=EDGE_LOOP('',(#30443,#30444,#30445,#30446));
#5133=EDGE_LOOP('',(#30447,#30448,#30449,#30450));
#5134=EDGE_LOOP('',(#30451,#30452,#30453,#30454));
#5135=EDGE_LOOP('',(#30455,#30456,#30457,#30458,#30459,#30460));
#5136=EDGE_LOOP('',(#30461,#30462,#30463,#30464,#30465,#30466));
#5137=EDGE_LOOP('',(#30467,#30468,#30469,#30470));
#5138=EDGE_LOOP('',(#30471,#30472,#30473,#30474));
#5139=EDGE_LOOP('',(#30475,#30476,#30477,#30478,#30479,#30480));
#5140=EDGE_LOOP('',(#30481,#30482,#30483,#30484,#30485,#30486));
#5141=EDGE_LOOP('',(#30487,#30488,#30489,#30490));
#5142=EDGE_LOOP('',(#30491,#30492,#30493,#30494,#30495,#30496,#30497,#30498));
#5143=EDGE_LOOP('',(#30499,#30500,#30501,#30502,#30503,#30504,#30505,#30506));
#5144=EDGE_LOOP('',(#30507,#30508,#30509,#30510));
#5145=EDGE_LOOP('',(#30511,#30512,#30513,#30514,#30515,#30516,#30517,#30518,
#30519,#30520));
#5146=EDGE_LOOP('',(#30521,#30522,#30523,#30524));
#5147=EDGE_LOOP('',(#30525,#30526,#30527,#30528));
#5148=EDGE_LOOP('',(#30529,#30530,#30531,#30532));
#5149=EDGE_LOOP('',(#30533,#30534,#30535,#30536));
#5150=EDGE_LOOP('',(#30537,#30538,#30539,#30540));
#5151=EDGE_LOOP('',(#30541,#30542,#30543,#30544));
#5152=EDGE_LOOP('',(#30545,#30546,#30547,#30548,#30549,#30550,#30551,#30552,
#30553,#30554,#30555,#30556,#30557,#30558,#30559,#30560,#30561,#30562,#30563));
#5153=EDGE_LOOP('',(#30564,#30565,#30566,#30567));
#5154=EDGE_LOOP('',(#30568,#30569,#30570,#30571,#30572,#30573,#30574,#30575,
#30576,#30577,#30578,#30579,#30580,#30581,#30582,#30583,#30584,#30585,#30586));
#5155=EDGE_LOOP('',(#30587,#30588,#30589,#30590));
#5156=EDGE_LOOP('',(#30591,#30592,#30593,#30594));
#5157=EDGE_LOOP('',(#30595,#30596,#30597,#30598));
#5158=EDGE_LOOP('',(#30599,#30600,#30601,#30602));
#5159=EDGE_LOOP('',(#30603,#30604,#30605,#30606,#30607,#30608,#30609,#30610,
#30611,#30612,#30613,#30614));
#5160=EDGE_LOOP('',(#30615,#30616,#30617,#30618));
#5161=EDGE_LOOP('',(#30619,#30620,#30621,#30622));
#5162=EDGE_LOOP('',(#30623,#30624,#30625,#30626));
#5163=EDGE_LOOP('',(#30627,#30628,#30629,#30630));
#5164=EDGE_LOOP('',(#30631,#30632,#30633,#30634,#30635,#30636,#30637,#30638,
#30639,#30640,#30641,#30642));
#5165=EDGE_LOOP('',(#30643,#30644,#30645,#30646));
#5166=EDGE_LOOP('',(#30647,#30648,#30649,#30650,#30651,#30652,#30653,#30654));
#5167=EDGE_LOOP('',(#30655));
#5168=EDGE_LOOP('',(#30656,#30657,#30658,#30659,#30660,#30661,#30662,#30663));
#5169=EDGE_LOOP('',(#30664));
#5170=EDGE_LOOP('',(#30665,#30666,#30667,#30668));
#5171=EDGE_LOOP('',(#30669,#30670,#30671,#30672,#30673,#30674,#30675,#30676));
#5172=EDGE_LOOP('',(#30677));
#5173=EDGE_LOOP('',(#30678,#30679,#30680,#30681,#30682,#30683,#30684,#30685));
#5174=EDGE_LOOP('',(#30686));
#5175=EDGE_LOOP('',(#30687,#30688,#30689,#30690));
#5176=EDGE_LOOP('',(#30691,#30692,#30693,#30694));
#5177=EDGE_LOOP('',(#30695,#30696,#30697,#30698));
#5178=EDGE_LOOP('',(#30699,#30700,#30701,#30702));
#5179=EDGE_LOOP('',(#30703,#30704,#30705,#30706));
#5180=EDGE_LOOP('',(#30707,#30708,#30709,#30710));
#5181=EDGE_LOOP('',(#30711,#30712,#30713,#30714));
#5182=EDGE_LOOP('',(#30715,#30716,#30717,#30718));
#5183=EDGE_LOOP('',(#30719,#30720,#30721,#30722));
#5184=EDGE_LOOP('',(#30723,#30724,#30725,#30726));
#5185=EDGE_LOOP('',(#30727,#30728,#30729,#30730));
#5186=EDGE_LOOP('',(#30731,#30732,#30733,#30734));
#5187=EDGE_LOOP('',(#30735,#30736,#30737,#30738));
#5188=EDGE_LOOP('',(#30739,#30740,#30741,#30742));
#5189=EDGE_LOOP('',(#30743,#30744,#30745,#30746));
#5190=EDGE_LOOP('',(#30747,#30748,#30749,#30750));
#5191=EDGE_LOOP('',(#30751,#30752,#30753,#30754));
#5192=EDGE_LOOP('',(#30755,#30756,#30757,#30758));
#5193=EDGE_LOOP('',(#30759,#30760,#30761,#30762));
#5194=EDGE_LOOP('',(#30763,#30764,#30765,#30766));
#5195=EDGE_LOOP('',(#30767,#30768,#30769,#30770));
#5196=EDGE_LOOP('',(#30771,#30772,#30773,#30774));
#5197=EDGE_LOOP('',(#30775,#30776,#30777,#30778));
#5198=EDGE_LOOP('',(#30779,#30780,#30781,#30782));
#5199=EDGE_LOOP('',(#30783,#30784,#30785,#30786));
#5200=EDGE_LOOP('',(#30787,#30788,#30789,#30790));
#5201=EDGE_LOOP('',(#30791,#30792,#30793,#30794));
#5202=EDGE_LOOP('',(#30795,#30796,#30797,#30798,#30799,#30800,#30801,#30802,
#30803,#30804,#30805,#30806));
#5203=EDGE_LOOP('',(#30807));
#5204=EDGE_LOOP('',(#30808,#30809,#30810,#30811,#30812,#30813,#30814,#30815,
#30816,#30817,#30818,#30819));
#5205=EDGE_LOOP('',(#30820));
#5206=EDGE_LOOP('',(#30821,#30822,#30823,#30824));
#5207=EDGE_LOOP('',(#30825,#30826,#30827,#30828));
#5208=EDGE_LOOP('',(#30829,#30830,#30831,#30832));
#5209=EDGE_LOOP('',(#30833,#30834,#30835,#30836));
#5210=EDGE_LOOP('',(#30837,#30838,#30839,#30840));
#5211=EDGE_LOOP('',(#30841,#30842,#30843,#30844));
#5212=EDGE_LOOP('',(#30845,#30846,#30847,#30848));
#5213=EDGE_LOOP('',(#30849,#30850,#30851,#30852));
#5214=EDGE_LOOP('',(#30853,#30854,#30855,#30856));
#5215=EDGE_LOOP('',(#30857,#30858,#30859,#30860));
#5216=EDGE_LOOP('',(#30861,#30862,#30863,#30864));
#5217=EDGE_LOOP('',(#30865,#30866,#30867,#30868));
#5218=EDGE_LOOP('',(#30869,#30870,#30871,#30872));
#5219=EDGE_LOOP('',(#30873,#30874,#30875,#30876));
#5220=EDGE_LOOP('',(#30877,#30878,#30879,#30880));
#5221=EDGE_LOOP('',(#30881,#30882,#30883,#30884));
#5222=EDGE_LOOP('',(#30885,#30886,#30887,#30888));
#5223=EDGE_LOOP('',(#30889,#30890,#30891,#30892));
#5224=EDGE_LOOP('',(#30893,#30894,#30895,#30896));
#5225=EDGE_LOOP('',(#30897,#30898,#30899,#30900));
#5226=EDGE_LOOP('',(#30901,#30902,#30903,#30904,#30905,#30906,#30907,#30908,
#30909,#30910));
#5227=EDGE_LOOP('',(#30911,#30912,#30913,#30914));
#5228=EDGE_LOOP('',(#30915,#30916,#30917,#30918,#30919,#30920,#30921,#30922,
#30923,#30924));
#5229=EDGE_LOOP('',(#30925,#30926,#30927,#30928));
#5230=EDGE_LOOP('',(#30929,#30930,#30931,#30932));
#5231=EDGE_LOOP('',(#30933,#30934,#30935,#30936));
#5232=EDGE_LOOP('',(#30937,#30938,#30939,#30940));
#5233=EDGE_LOOP('',(#30941,#30942,#30943,#30944));
#5234=EDGE_LOOP('',(#30945,#30946,#30947,#30948));
#5235=EDGE_LOOP('',(#30949,#30950,#30951,#30952));
#5236=EDGE_LOOP('',(#30953,#30954,#30955,#30956));
#5237=EDGE_LOOP('',(#30957,#30958,#30959,#30960));
#5238=EDGE_LOOP('',(#30961,#30962,#30963,#30964));
#5239=EDGE_LOOP('',(#30965,#30966,#30967,#30968));
#5240=EDGE_LOOP('',(#30969,#30970,#30971,#30972));
#5241=EDGE_LOOP('',(#30973,#30974,#30975,#30976));
#5242=EDGE_LOOP('',(#30977,#30978,#30979,#30980));
#5243=EDGE_LOOP('',(#30981,#30982,#30983,#30984));
#5244=EDGE_LOOP('',(#30985,#30986,#30987,#30988,#30989,#30990,#30991,#30992,
#30993,#30994));
#5245=EDGE_LOOP('',(#30995,#30996,#30997,#30998));
#5246=EDGE_LOOP('',(#30999,#31000,#31001,#31002,#31003,#31004,#31005,#31006,
#31007,#31008));
#5247=EDGE_LOOP('',(#31009,#31010,#31011,#31012));
#5248=EDGE_LOOP('',(#31013,#31014,#31015,#31016));
#5249=EDGE_LOOP('',(#31017,#31018,#31019,#31020));
#5250=EDGE_LOOP('',(#31021));
#5251=EDGE_LOOP('',(#31022,#31023,#31024,#31025,#31026,#31027));
#5252=EDGE_LOOP('',(#31028,#31029,#31030,#31031,#31032,#31033));
#5253=EDGE_LOOP('',(#31034,#31035,#31036,#31037,#31038,#31039));
#5254=EDGE_LOOP('',(#31040,#31041,#31042,#31043,#31044,#31045));
#5255=EDGE_LOOP('',(#31046,#31047,#31048,#31049,#31050,#31051));
#5256=EDGE_LOOP('',(#31052,#31053,#31054,#31055,#31056,#31057));
#5257=EDGE_LOOP('',(#31058,#31059,#31060,#31061,#31062,#31063));
#5258=EDGE_LOOP('',(#31064,#31065,#31066,#31067,#31068,#31069));
#5259=EDGE_LOOP('',(#31070,#31071,#31072,#31073,#31074,#31075));
#5260=EDGE_LOOP('',(#31076,#31077,#31078,#31079,#31080,#31081));
#5261=EDGE_LOOP('',(#31082,#31083,#31084,#31085,#31086,#31087));
#5262=EDGE_LOOP('',(#31088,#31089,#31090,#31091,#31092,#31093));
#5263=EDGE_LOOP('',(#31094,#31095,#31096,#31097,#31098,#31099));
#5264=EDGE_LOOP('',(#31100,#31101,#31102,#31103,#31104,#31105));
#5265=EDGE_LOOP('',(#31106,#31107,#31108,#31109,#31110,#31111));
#5266=EDGE_LOOP('',(#31112,#31113,#31114,#31115,#31116,#31117));
#5267=EDGE_LOOP('',(#31118,#31119,#31120,#31121,#31122,#31123));
#5268=EDGE_LOOP('',(#31124,#31125,#31126,#31127,#31128,#31129));
#5269=EDGE_LOOP('',(#31130,#31131,#31132,#31133,#31134,#31135));
#5270=EDGE_LOOP('',(#31136,#31137,#31138,#31139,#31140,#31141));
#5271=EDGE_LOOP('',(#31142,#31143,#31144,#31145,#31146,#31147));
#5272=EDGE_LOOP('',(#31148,#31149,#31150,#31151,#31152,#31153));
#5273=EDGE_LOOP('',(#31154,#31155,#31156,#31157,#31158,#31159));
#5274=EDGE_LOOP('',(#31160,#31161,#31162,#31163,#31164,#31165));
#5275=EDGE_LOOP('',(#31166,#31167,#31168,#31169,#31170,#31171));
#5276=EDGE_LOOP('',(#31172,#31173,#31174,#31175,#31176,#31177));
#5277=EDGE_LOOP('',(#31178,#31179,#31180,#31181,#31182,#31183));
#5278=EDGE_LOOP('',(#31184,#31185,#31186,#31187,#31188,#31189));
#5279=EDGE_LOOP('',(#31190,#31191,#31192,#31193,#31194,#31195));
#5280=EDGE_LOOP('',(#31196,#31197,#31198,#31199,#31200,#31201));
#5281=EDGE_LOOP('',(#31202,#31203,#31204,#31205,#31206,#31207));
#5282=EDGE_LOOP('',(#31208,#31209,#31210,#31211,#31212,#31213));
#5283=EDGE_LOOP('',(#31214,#31215,#31216,#31217,#31218,#31219));
#5284=EDGE_LOOP('',(#31220,#31221,#31222,#31223,#31224,#31225));
#5285=EDGE_LOOP('',(#31226,#31227,#31228,#31229,#31230,#31231));
#5286=EDGE_LOOP('',(#31232,#31233,#31234,#31235,#31236,#31237));
#5287=EDGE_LOOP('',(#31238,#31239,#31240,#31241,#31242,#31243));
#5288=EDGE_LOOP('',(#31244,#31245,#31246,#31247,#31248,#31249));
#5289=EDGE_LOOP('',(#31250,#31251,#31252,#31253,#31254,#31255));
#5290=EDGE_LOOP('',(#31256,#31257,#31258,#31259,#31260,#31261));
#5291=EDGE_LOOP('',(#31262,#31263,#31264,#31265,#31266,#31267));
#5292=EDGE_LOOP('',(#31268,#31269,#31270,#31271,#31272,#31273));
#5293=EDGE_LOOP('',(#31274,#31275,#31276,#31277,#31278,#31279));
#5294=EDGE_LOOP('',(#31280,#31281,#31282,#31283,#31284,#31285));
#5295=EDGE_LOOP('',(#31286,#31287,#31288,#31289,#31290,#31291));
#5296=EDGE_LOOP('',(#31292,#31293,#31294,#31295,#31296,#31297));
#5297=EDGE_LOOP('',(#31298,#31299,#31300,#31301,#31302,#31303));
#5298=EDGE_LOOP('',(#31304,#31305,#31306,#31307,#31308,#31309));
#5299=EDGE_LOOP('',(#31310,#31311,#31312,#31313,#31314,#31315));
#5300=EDGE_LOOP('',(#31316,#31317,#31318,#31319,#31320,#31321));
#5301=EDGE_LOOP('',(#31322,#31323,#31324,#31325,#31326,#31327));
#5302=EDGE_LOOP('',(#31328,#31329,#31330,#31331,#31332,#31333));
#5303=EDGE_LOOP('',(#31334,#31335,#31336,#31337,#31338,#31339));
#5304=EDGE_LOOP('',(#31340,#31341,#31342,#31343,#31344,#31345));
#5305=EDGE_LOOP('',(#31346,#31347,#31348,#31349,#31350,#31351));
#5306=EDGE_LOOP('',(#31352,#31353,#31354,#31355,#31356,#31357));
#5307=EDGE_LOOP('',(#31358,#31359,#31360,#31361,#31362,#31363));
#5308=EDGE_LOOP('',(#31364,#31365,#31366,#31367,#31368,#31369));
#5309=EDGE_LOOP('',(#31370,#31371,#31372,#31373,#31374,#31375));
#5310=EDGE_LOOP('',(#31376,#31377,#31378,#31379,#31380,#31381));
#5311=EDGE_LOOP('',(#31382,#31383,#31384,#31385,#31386,#31387));
#5312=EDGE_LOOP('',(#31388,#31389,#31390,#31391,#31392,#31393));
#5313=EDGE_LOOP('',(#31394,#31395,#31396,#31397,#31398,#31399));
#5314=EDGE_LOOP('',(#31400,#31401,#31402,#31403,#31404,#31405));
#5315=EDGE_LOOP('',(#31406,#31407,#31408,#31409,#31410,#31411));
#5316=EDGE_LOOP('',(#31412,#31413,#31414,#31415,#31416,#31417));
#5317=EDGE_LOOP('',(#31418,#31419,#31420,#31421,#31422,#31423));
#5318=EDGE_LOOP('',(#31424,#31425,#31426,#31427,#31428,#31429));
#5319=EDGE_LOOP('',(#31430,#31431,#31432,#31433,#31434,#31435));
#5320=EDGE_LOOP('',(#31436,#31437,#31438,#31439,#31440,#31441));
#5321=EDGE_LOOP('',(#31442,#31443,#31444,#31445,#31446,#31447));
#5322=EDGE_LOOP('',(#31448,#31449,#31450,#31451,#31452,#31453));
#5323=EDGE_LOOP('',(#31454,#31455,#31456,#31457,#31458,#31459));
#5324=EDGE_LOOP('',(#31460,#31461,#31462,#31463,#31464,#31465));
#5325=EDGE_LOOP('',(#31466,#31467,#31468,#31469,#31470,#31471));
#5326=EDGE_LOOP('',(#31472,#31473,#31474,#31475,#31476,#31477));
#5327=EDGE_LOOP('',(#31478,#31479,#31480,#31481,#31482,#31483));
#5328=EDGE_LOOP('',(#31484,#31485,#31486,#31487,#31488,#31489));
#5329=EDGE_LOOP('',(#31490,#31491,#31492,#31493,#31494,#31495));
#5330=EDGE_LOOP('',(#31496,#31497,#31498,#31499,#31500,#31501));
#5331=EDGE_LOOP('',(#31502,#31503,#31504,#31505,#31506,#31507));
#5332=EDGE_LOOP('',(#31508,#31509,#31510,#31511,#31512,#31513));
#5333=EDGE_LOOP('',(#31514,#31515,#31516,#31517,#31518,#31519));
#5334=EDGE_LOOP('',(#31520,#31521,#31522,#31523,#31524,#31525));
#5335=EDGE_LOOP('',(#31526,#31527,#31528,#31529,#31530,#31531));
#5336=EDGE_LOOP('',(#31532,#31533,#31534,#31535,#31536,#31537));
#5337=EDGE_LOOP('',(#31538,#31539,#31540,#31541,#31542,#31543));
#5338=EDGE_LOOP('',(#31544,#31545,#31546,#31547,#31548,#31549));
#5339=EDGE_LOOP('',(#31550,#31551,#31552,#31553,#31554,#31555));
#5340=EDGE_LOOP('',(#31556,#31557,#31558,#31559,#31560,#31561));
#5341=EDGE_LOOP('',(#31562,#31563,#31564,#31565,#31566,#31567));
#5342=EDGE_LOOP('',(#31568,#31569,#31570,#31571,#31572,#31573));
#5343=EDGE_LOOP('',(#31574,#31575,#31576,#31577,#31578,#31579));
#5344=EDGE_LOOP('',(#31580,#31581,#31582,#31583,#31584,#31585));
#5345=EDGE_LOOP('',(#31586,#31587,#31588,#31589,#31590,#31591));
#5346=EDGE_LOOP('',(#31592,#31593,#31594,#31595,#31596,#31597));
#5347=EDGE_LOOP('',(#31598,#31599,#31600,#31601,#31602,#31603));
#5348=EDGE_LOOP('',(#31604,#31605,#31606,#31607,#31608,#31609));
#5349=EDGE_LOOP('',(#31610,#31611,#31612,#31613,#31614,#31615));
#5350=EDGE_LOOP('',(#31616,#31617,#31618,#31619,#31620,#31621));
#5351=EDGE_LOOP('',(#31622,#31623,#31624,#31625,#31626,#31627));
#5352=EDGE_LOOP('',(#31628,#31629,#31630,#31631,#31632,#31633));
#5353=EDGE_LOOP('',(#31634,#31635,#31636,#31637,#31638,#31639));
#5354=EDGE_LOOP('',(#31640,#31641,#31642,#31643,#31644,#31645));
#5355=EDGE_LOOP('',(#31646,#31647,#31648,#31649,#31650,#31651));
#5356=EDGE_LOOP('',(#31652,#31653,#31654,#31655,#31656,#31657));
#5357=EDGE_LOOP('',(#31658,#31659,#31660,#31661,#31662,#31663));
#5358=EDGE_LOOP('',(#31664,#31665,#31666,#31667,#31668,#31669));
#5359=EDGE_LOOP('',(#31670,#31671,#31672,#31673,#31674,#31675));
#5360=EDGE_LOOP('',(#31676,#31677,#31678,#31679,#31680,#31681));
#5361=EDGE_LOOP('',(#31682,#31683,#31684,#31685,#31686,#31687));
#5362=EDGE_LOOP('',(#31688,#31689,#31690,#31691,#31692,#31693));
#5363=EDGE_LOOP('',(#31694,#31695,#31696,#31697,#31698,#31699));
#5364=EDGE_LOOP('',(#31700,#31701,#31702,#31703,#31704,#31705));
#5365=EDGE_LOOP('',(#31706,#31707,#31708,#31709,#31710,#31711));
#5366=EDGE_LOOP('',(#31712,#31713,#31714,#31715,#31716,#31717));
#5367=EDGE_LOOP('',(#31718,#31719,#31720,#31721,#31722,#31723));
#5368=EDGE_LOOP('',(#31724,#31725,#31726,#31727,#31728,#31729));
#5369=EDGE_LOOP('',(#31730,#31731,#31732,#31733,#31734,#31735));
#5370=EDGE_LOOP('',(#31736,#31737,#31738,#31739,#31740,#31741));
#5371=EDGE_LOOP('',(#31742,#31743,#31744,#31745,#31746,#31747));
#5372=EDGE_LOOP('',(#31748,#31749,#31750,#31751,#31752,#31753));
#5373=EDGE_LOOP('',(#31754,#31755,#31756,#31757,#31758,#31759));
#5374=EDGE_LOOP('',(#31760,#31761,#31762,#31763,#31764,#31765));
#5375=EDGE_LOOP('',(#31766,#31767,#31768,#31769,#31770,#31771));
#5376=EDGE_LOOP('',(#31772,#31773,#31774,#31775,#31776,#31777));
#5377=EDGE_LOOP('',(#31778,#31779,#31780,#31781,#31782,#31783));
#5378=EDGE_LOOP('',(#31784,#31785,#31786,#31787,#31788,#31789));
#5379=EDGE_LOOP('',(#31790,#31791,#31792,#31793,#31794,#31795));
#5380=EDGE_LOOP('',(#31796,#31797,#31798,#31799,#31800,#31801));
#5381=EDGE_LOOP('',(#31802,#31803,#31804,#31805,#31806,#31807));
#5382=EDGE_LOOP('',(#31808,#31809,#31810,#31811,#31812,#31813));
#5383=EDGE_LOOP('',(#31814,#31815,#31816,#31817,#31818,#31819));
#5384=EDGE_LOOP('',(#31820,#31821,#31822,#31823,#31824,#31825));
#5385=EDGE_LOOP('',(#31826,#31827,#31828,#31829,#31830,#31831));
#5386=EDGE_LOOP('',(#31832,#31833,#31834,#31835,#31836,#31837));
#5387=EDGE_LOOP('',(#31838,#31839,#31840,#31841,#31842,#31843));
#5388=EDGE_LOOP('',(#31844,#31845,#31846,#31847,#31848,#31849));
#5389=EDGE_LOOP('',(#31850,#31851,#31852,#31853,#31854,#31855));
#5390=EDGE_LOOP('',(#31856,#31857,#31858,#31859,#31860,#31861));
#5391=EDGE_LOOP('',(#31862,#31863,#31864,#31865,#31866,#31867));
#5392=EDGE_LOOP('',(#31868,#31869,#31870,#31871,#31872,#31873));
#5393=EDGE_LOOP('',(#31874,#31875,#31876,#31877,#31878,#31879));
#5394=EDGE_LOOP('',(#31880,#31881,#31882,#31883,#31884,#31885));
#5395=EDGE_LOOP('',(#31886,#31887,#31888,#31889,#31890,#31891));
#5396=EDGE_LOOP('',(#31892,#31893,#31894,#31895,#31896,#31897));
#5397=EDGE_LOOP('',(#31898,#31899,#31900,#31901,#31902,#31903));
#5398=EDGE_LOOP('',(#31904,#31905,#31906,#31907,#31908,#31909));
#5399=EDGE_LOOP('',(#31910,#31911,#31912,#31913,#31914,#31915));
#5400=EDGE_LOOP('',(#31916,#31917,#31918,#31919,#31920,#31921));
#5401=EDGE_LOOP('',(#31922,#31923,#31924,#31925,#31926,#31927));
#5402=EDGE_LOOP('',(#31928,#31929,#31930,#31931,#31932,#31933));
#5403=EDGE_LOOP('',(#31934,#31935,#31936,#31937,#31938,#31939));
#5404=EDGE_LOOP('',(#31940,#31941,#31942,#31943,#31944,#31945));
#5405=EDGE_LOOP('',(#31946,#31947,#31948,#31949,#31950,#31951));
#5406=EDGE_LOOP('',(#31952,#31953,#31954,#31955,#31956,#31957));
#5407=EDGE_LOOP('',(#31958,#31959,#31960,#31961,#31962,#31963));
#5408=EDGE_LOOP('',(#31964,#31965,#31966,#31967,#31968,#31969));
#5409=EDGE_LOOP('',(#31970,#31971,#31972,#31973,#31974,#31975));
#5410=EDGE_LOOP('',(#31976,#31977,#31978,#31979,#31980,#31981));
#5411=EDGE_LOOP('',(#31982,#31983,#31984,#31985,#31986,#31987));
#5412=EDGE_LOOP('',(#31988,#31989,#31990,#31991,#31992,#31993));
#5413=EDGE_LOOP('',(#31994,#31995,#31996,#31997,#31998,#31999));
#5414=EDGE_LOOP('',(#32000,#32001,#32002,#32003,#32004,#32005));
#5415=EDGE_LOOP('',(#32006,#32007,#32008,#32009,#32010,#32011));
#5416=EDGE_LOOP('',(#32012,#32013,#32014,#32015,#32016,#32017));
#5417=EDGE_LOOP('',(#32018,#32019,#32020,#32021,#32022,#32023));
#5418=EDGE_LOOP('',(#32024,#32025,#32026,#32027,#32028,#32029));
#5419=EDGE_LOOP('',(#32030,#32031,#32032,#32033,#32034,#32035));
#5420=EDGE_LOOP('',(#32036,#32037,#32038,#32039,#32040,#32041));
#5421=EDGE_LOOP('',(#32042,#32043,#32044,#32045,#32046,#32047));
#5422=EDGE_LOOP('',(#32048,#32049,#32050,#32051,#32052,#32053));
#5423=EDGE_LOOP('',(#32054,#32055,#32056,#32057,#32058,#32059));
#5424=EDGE_LOOP('',(#32060,#32061,#32062,#32063,#32064,#32065));
#5425=EDGE_LOOP('',(#32066,#32067,#32068,#32069,#32070,#32071));
#5426=EDGE_LOOP('',(#32072,#32073,#32074,#32075,#32076,#32077));
#5427=EDGE_LOOP('',(#32078,#32079,#32080,#32081,#32082,#32083));
#5428=EDGE_LOOP('',(#32084,#32085,#32086,#32087,#32088,#32089));
#5429=EDGE_LOOP('',(#32090,#32091,#32092,#32093,#32094,#32095));
#5430=EDGE_LOOP('',(#32096,#32097,#32098,#32099,#32100,#32101));
#5431=EDGE_LOOP('',(#32102,#32103,#32104,#32105,#32106,#32107));
#5432=EDGE_LOOP('',(#32108,#32109,#32110,#32111,#32112,#32113));
#5433=EDGE_LOOP('',(#32114,#32115,#32116,#32117,#32118,#32119));
#5434=EDGE_LOOP('',(#32120,#32121,#32122,#32123,#32124,#32125));
#5435=EDGE_LOOP('',(#32126,#32127,#32128,#32129,#32130,#32131));
#5436=EDGE_LOOP('',(#32132,#32133,#32134,#32135,#32136,#32137));
#5437=EDGE_LOOP('',(#32138));
#5438=EDGE_LOOP('',(#32139,#32140,#32141,#32142,#32143,#32144));
#5439=EDGE_LOOP('',(#32145,#32146,#32147,#32148,#32149,#32150));
#5440=EDGE_LOOP('',(#32151,#32152,#32153,#32154,#32155,#32156));
#5441=EDGE_LOOP('',(#32157,#32158,#32159,#32160,#32161,#32162));
#5442=EDGE_LOOP('',(#32163,#32164,#32165,#32166,#32167,#32168));
#5443=EDGE_LOOP('',(#32169,#32170,#32171,#32172,#32173,#32174));
#5444=EDGE_LOOP('',(#32175,#32176,#32177,#32178,#32179,#32180));
#5445=EDGE_LOOP('',(#32181,#32182,#32183,#32184,#32185,#32186));
#5446=EDGE_LOOP('',(#32187,#32188,#32189,#32190,#32191,#32192));
#5447=EDGE_LOOP('',(#32193,#32194,#32195,#32196,#32197,#32198));
#5448=EDGE_LOOP('',(#32199,#32200,#32201,#32202,#32203,#32204));
#5449=EDGE_LOOP('',(#32205,#32206,#32207,#32208,#32209,#32210));
#5450=EDGE_LOOP('',(#32211,#32212,#32213,#32214,#32215,#32216));
#5451=EDGE_LOOP('',(#32217,#32218,#32219,#32220,#32221,#32222));
#5452=EDGE_LOOP('',(#32223,#32224,#32225,#32226,#32227,#32228));
#5453=EDGE_LOOP('',(#32229,#32230,#32231,#32232,#32233,#32234));
#5454=EDGE_LOOP('',(#32235,#32236,#32237,#32238,#32239,#32240));
#5455=EDGE_LOOP('',(#32241,#32242,#32243,#32244,#32245,#32246));
#5456=EDGE_LOOP('',(#32247,#32248,#32249,#32250,#32251,#32252));
#5457=EDGE_LOOP('',(#32253,#32254,#32255,#32256,#32257,#32258));
#5458=EDGE_LOOP('',(#32259,#32260,#32261,#32262,#32263,#32264));
#5459=EDGE_LOOP('',(#32265,#32266,#32267,#32268,#32269,#32270));
#5460=EDGE_LOOP('',(#32271,#32272,#32273,#32274,#32275,#32276));
#5461=EDGE_LOOP('',(#32277,#32278,#32279,#32280,#32281,#32282));
#5462=EDGE_LOOP('',(#32283,#32284,#32285,#32286,#32287,#32288));
#5463=EDGE_LOOP('',(#32289,#32290,#32291,#32292,#32293,#32294));
#5464=EDGE_LOOP('',(#32295,#32296,#32297,#32298,#32299,#32300));
#5465=EDGE_LOOP('',(#32301,#32302,#32303,#32304,#32305,#32306));
#5466=EDGE_LOOP('',(#32307,#32308,#32309,#32310,#32311,#32312));
#5467=EDGE_LOOP('',(#32313,#32314,#32315,#32316,#32317,#32318));
#5468=EDGE_LOOP('',(#32319,#32320,#32321,#32322,#32323,#32324));
#5469=EDGE_LOOP('',(#32325,#32326,#32327,#32328,#32329,#32330));
#5470=EDGE_LOOP('',(#32331,#32332,#32333,#32334,#32335,#32336));
#5471=EDGE_LOOP('',(#32337,#32338,#32339,#32340,#32341,#32342));
#5472=EDGE_LOOP('',(#32343,#32344,#32345,#32346,#32347,#32348));
#5473=EDGE_LOOP('',(#32349,#32350,#32351,#32352,#32353,#32354));
#5474=EDGE_LOOP('',(#32355,#32356,#32357,#32358,#32359,#32360));
#5475=EDGE_LOOP('',(#32361,#32362,#32363,#32364,#32365,#32366));
#5476=EDGE_LOOP('',(#32367,#32368,#32369,#32370,#32371,#32372));
#5477=EDGE_LOOP('',(#32373,#32374,#32375,#32376,#32377,#32378));
#5478=EDGE_LOOP('',(#32379,#32380,#32381,#32382,#32383,#32384));
#5479=EDGE_LOOP('',(#32385,#32386,#32387,#32388,#32389,#32390));
#5480=EDGE_LOOP('',(#32391,#32392,#32393,#32394,#32395,#32396));
#5481=EDGE_LOOP('',(#32397,#32398,#32399,#32400,#32401,#32402));
#5482=EDGE_LOOP('',(#32403,#32404,#32405,#32406,#32407,#32408));
#5483=EDGE_LOOP('',(#32409,#32410,#32411,#32412,#32413,#32414));
#5484=EDGE_LOOP('',(#32415,#32416,#32417,#32418,#32419,#32420));
#5485=EDGE_LOOP('',(#32421,#32422,#32423,#32424,#32425,#32426));
#5486=EDGE_LOOP('',(#32427,#32428,#32429,#32430,#32431,#32432));
#5487=EDGE_LOOP('',(#32433,#32434,#32435,#32436,#32437,#32438));
#5488=EDGE_LOOP('',(#32439,#32440,#32441,#32442,#32443,#32444));
#5489=EDGE_LOOP('',(#32445,#32446,#32447,#32448,#32449,#32450));
#5490=EDGE_LOOP('',(#32451,#32452,#32453,#32454,#32455,#32456));
#5491=EDGE_LOOP('',(#32457,#32458,#32459,#32460,#32461,#32462));
#5492=EDGE_LOOP('',(#32463,#32464,#32465,#32466,#32467,#32468));
#5493=EDGE_LOOP('',(#32469,#32470,#32471,#32472,#32473,#32474));
#5494=EDGE_LOOP('',(#32475,#32476,#32477,#32478,#32479,#32480));
#5495=EDGE_LOOP('',(#32481,#32482,#32483,#32484,#32485,#32486));
#5496=EDGE_LOOP('',(#32487,#32488,#32489,#32490,#32491,#32492));
#5497=EDGE_LOOP('',(#32493,#32494,#32495,#32496,#32497,#32498));
#5498=EDGE_LOOP('',(#32499,#32500,#32501,#32502,#32503,#32504));
#5499=EDGE_LOOP('',(#32505,#32506,#32507,#32508,#32509,#32510));
#5500=EDGE_LOOP('',(#32511,#32512,#32513,#32514,#32515,#32516));
#5501=EDGE_LOOP('',(#32517,#32518,#32519,#32520,#32521,#32522));
#5502=EDGE_LOOP('',(#32523,#32524,#32525,#32526,#32527,#32528));
#5503=EDGE_LOOP('',(#32529,#32530,#32531,#32532,#32533,#32534));
#5504=EDGE_LOOP('',(#32535,#32536,#32537,#32538,#32539,#32540));
#5505=EDGE_LOOP('',(#32541,#32542,#32543,#32544,#32545,#32546));
#5506=EDGE_LOOP('',(#32547,#32548,#32549,#32550,#32551,#32552));
#5507=EDGE_LOOP('',(#32553,#32554,#32555,#32556,#32557,#32558));
#5508=EDGE_LOOP('',(#32559,#32560,#32561,#32562,#32563,#32564));
#5509=EDGE_LOOP('',(#32565,#32566,#32567,#32568,#32569,#32570));
#5510=EDGE_LOOP('',(#32571,#32572,#32573,#32574,#32575,#32576));
#5511=EDGE_LOOP('',(#32577,#32578,#32579,#32580,#32581,#32582));
#5512=EDGE_LOOP('',(#32583,#32584,#32585,#32586,#32587,#32588));
#5513=EDGE_LOOP('',(#32589,#32590,#32591,#32592,#32593,#32594));
#5514=EDGE_LOOP('',(#32595,#32596,#32597,#32598,#32599,#32600));
#5515=EDGE_LOOP('',(#32601,#32602,#32603,#32604,#32605,#32606));
#5516=EDGE_LOOP('',(#32607,#32608,#32609,#32610,#32611,#32612));
#5517=EDGE_LOOP('',(#32613,#32614,#32615,#32616,#32617,#32618));
#5518=EDGE_LOOP('',(#32619,#32620,#32621,#32622,#32623,#32624));
#5519=EDGE_LOOP('',(#32625,#32626,#32627,#32628,#32629,#32630));
#5520=EDGE_LOOP('',(#32631,#32632,#32633,#32634,#32635,#32636));
#5521=EDGE_LOOP('',(#32637,#32638,#32639,#32640,#32641,#32642));
#5522=EDGE_LOOP('',(#32643,#32644,#32645,#32646,#32647,#32648));
#5523=EDGE_LOOP('',(#32649,#32650,#32651,#32652,#32653,#32654));
#5524=EDGE_LOOP('',(#32655,#32656,#32657,#32658,#32659,#32660));
#5525=EDGE_LOOP('',(#32661,#32662,#32663,#32664,#32665,#32666));
#5526=EDGE_LOOP('',(#32667,#32668,#32669,#32670,#32671,#32672));
#5527=EDGE_LOOP('',(#32673,#32674,#32675,#32676,#32677,#32678));
#5528=EDGE_LOOP('',(#32679,#32680,#32681,#32682,#32683,#32684));
#5529=EDGE_LOOP('',(#32685,#32686,#32687,#32688,#32689,#32690));
#5530=EDGE_LOOP('',(#32691,#32692,#32693,#32694,#32695,#32696));
#5531=EDGE_LOOP('',(#32697,#32698,#32699,#32700,#32701,#32702));
#5532=EDGE_LOOP('',(#32703,#32704,#32705,#32706,#32707,#32708));
#5533=EDGE_LOOP('',(#32709,#32710,#32711,#32712,#32713,#32714));
#5534=EDGE_LOOP('',(#32715,#32716,#32717,#32718,#32719,#32720));
#5535=EDGE_LOOP('',(#32721,#32722,#32723,#32724,#32725,#32726));
#5536=EDGE_LOOP('',(#32727,#32728,#32729,#32730,#32731,#32732));
#5537=EDGE_LOOP('',(#32733,#32734,#32735,#32736,#32737,#32738));
#5538=EDGE_LOOP('',(#32739,#32740,#32741,#32742,#32743,#32744));
#5539=EDGE_LOOP('',(#32745,#32746,#32747,#32748,#32749,#32750));
#5540=EDGE_LOOP('',(#32751,#32752,#32753,#32754,#32755,#32756));
#5541=EDGE_LOOP('',(#32757,#32758,#32759,#32760,#32761,#32762));
#5542=EDGE_LOOP('',(#32763,#32764,#32765,#32766,#32767,#32768));
#5543=EDGE_LOOP('',(#32769,#32770,#32771,#32772,#32773,#32774));
#5544=EDGE_LOOP('',(#32775,#32776,#32777,#32778,#32779,#32780));
#5545=EDGE_LOOP('',(#32781,#32782,#32783,#32784,#32785,#32786));
#5546=EDGE_LOOP('',(#32787,#32788,#32789,#32790,#32791,#32792));
#5547=EDGE_LOOP('',(#32793,#32794,#32795,#32796,#32797,#32798));
#5548=EDGE_LOOP('',(#32799,#32800,#32801,#32802,#32803,#32804));
#5549=EDGE_LOOP('',(#32805,#32806,#32807,#32808,#32809,#32810));
#5550=EDGE_LOOP('',(#32811,#32812,#32813,#32814,#32815,#32816));
#5551=EDGE_LOOP('',(#32817,#32818,#32819,#32820,#32821,#32822));
#5552=EDGE_LOOP('',(#32823,#32824,#32825,#32826,#32827,#32828));
#5553=EDGE_LOOP('',(#32829,#32830,#32831,#32832,#32833,#32834));
#5554=EDGE_LOOP('',(#32835,#32836,#32837,#32838,#32839,#32840));
#5555=EDGE_LOOP('',(#32841,#32842,#32843,#32844,#32845,#32846));
#5556=EDGE_LOOP('',(#32847,#32848,#32849,#32850,#32851,#32852));
#5557=EDGE_LOOP('',(#32853,#32854,#32855,#32856,#32857,#32858));
#5558=EDGE_LOOP('',(#32859,#32860,#32861,#32862,#32863,#32864));
#5559=EDGE_LOOP('',(#32865,#32866,#32867,#32868,#32869,#32870));
#5560=EDGE_LOOP('',(#32871,#32872,#32873,#32874,#32875,#32876));
#5561=EDGE_LOOP('',(#32877,#32878,#32879,#32880,#32881,#32882));
#5562=EDGE_LOOP('',(#32883,#32884,#32885,#32886,#32887,#32888));
#5563=EDGE_LOOP('',(#32889,#32890,#32891,#32892,#32893,#32894));
#5564=EDGE_LOOP('',(#32895,#32896,#32897,#32898,#32899,#32900));
#5565=EDGE_LOOP('',(#32901,#32902,#32903,#32904,#32905,#32906));
#5566=EDGE_LOOP('',(#32907,#32908,#32909,#32910,#32911,#32912));
#5567=EDGE_LOOP('',(#32913,#32914,#32915,#32916,#32917,#32918));
#5568=EDGE_LOOP('',(#32919,#32920,#32921,#32922,#32923,#32924));
#5569=EDGE_LOOP('',(#32925,#32926,#32927,#32928,#32929,#32930));
#5570=EDGE_LOOP('',(#32931,#32932,#32933,#32934,#32935,#32936));
#5571=EDGE_LOOP('',(#32937,#32938,#32939,#32940,#32941,#32942));
#5572=EDGE_LOOP('',(#32943,#32944,#32945,#32946,#32947,#32948));
#5573=EDGE_LOOP('',(#32949,#32950,#32951,#32952,#32953,#32954));
#5574=EDGE_LOOP('',(#32955,#32956,#32957,#32958,#32959,#32960));
#5575=EDGE_LOOP('',(#32961,#32962,#32963,#32964,#32965,#32966));
#5576=EDGE_LOOP('',(#32967,#32968,#32969,#32970,#32971,#32972));
#5577=EDGE_LOOP('',(#32973,#32974,#32975,#32976,#32977,#32978));
#5578=EDGE_LOOP('',(#32979,#32980,#32981,#32982,#32983,#32984));
#5579=EDGE_LOOP('',(#32985,#32986,#32987,#32988,#32989,#32990));
#5580=EDGE_LOOP('',(#32991,#32992,#32993,#32994,#32995,#32996));
#5581=EDGE_LOOP('',(#32997,#32998,#32999,#33000,#33001,#33002));
#5582=EDGE_LOOP('',(#33003,#33004,#33005,#33006,#33007,#33008));
#5583=EDGE_LOOP('',(#33009,#33010,#33011,#33012,#33013,#33014));
#5584=EDGE_LOOP('',(#33015,#33016,#33017,#33018,#33019,#33020));
#5585=EDGE_LOOP('',(#33021,#33022,#33023,#33024,#33025,#33026));
#5586=EDGE_LOOP('',(#33027,#33028,#33029,#33030,#33031,#33032));
#5587=EDGE_LOOP('',(#33033,#33034,#33035,#33036,#33037,#33038));
#5588=EDGE_LOOP('',(#33039,#33040,#33041,#33042,#33043,#33044));
#5589=EDGE_LOOP('',(#33045,#33046,#33047,#33048,#33049,#33050));
#5590=EDGE_LOOP('',(#33051,#33052,#33053,#33054,#33055,#33056));
#5591=EDGE_LOOP('',(#33057,#33058,#33059,#33060,#33061,#33062));
#5592=EDGE_LOOP('',(#33063,#33064,#33065,#33066,#33067,#33068));
#5593=EDGE_LOOP('',(#33069,#33070,#33071,#33072,#33073,#33074));
#5594=EDGE_LOOP('',(#33075,#33076,#33077,#33078,#33079,#33080));
#5595=EDGE_LOOP('',(#33081,#33082,#33083,#33084,#33085,#33086));
#5596=EDGE_LOOP('',(#33087,#33088,#33089,#33090,#33091,#33092));
#5597=EDGE_LOOP('',(#33093,#33094,#33095,#33096,#33097,#33098));
#5598=EDGE_LOOP('',(#33099,#33100,#33101,#33102,#33103,#33104));
#5599=EDGE_LOOP('',(#33105,#33106,#33107,#33108,#33109,#33110));
#5600=EDGE_LOOP('',(#33111,#33112,#33113,#33114,#33115,#33116));
#5601=EDGE_LOOP('',(#33117,#33118,#33119,#33120,#33121,#33122));
#5602=EDGE_LOOP('',(#33123,#33124,#33125,#33126,#33127,#33128));
#5603=EDGE_LOOP('',(#33129,#33130,#33131,#33132,#33133,#33134));
#5604=EDGE_LOOP('',(#33135,#33136,#33137,#33138,#33139,#33140));
#5605=EDGE_LOOP('',(#33141,#33142,#33143,#33144,#33145,#33146));
#5606=EDGE_LOOP('',(#33147,#33148,#33149,#33150,#33151,#33152));
#5607=EDGE_LOOP('',(#33153,#33154,#33155,#33156,#33157,#33158));
#5608=EDGE_LOOP('',(#33159,#33160,#33161,#33162,#33163,#33164));
#5609=EDGE_LOOP('',(#33165,#33166,#33167,#33168,#33169,#33170));
#5610=EDGE_LOOP('',(#33171,#33172,#33173,#33174,#33175,#33176));
#5611=EDGE_LOOP('',(#33177,#33178,#33179,#33180,#33181,#33182));
#5612=EDGE_LOOP('',(#33183,#33184,#33185,#33186,#33187,#33188));
#5613=EDGE_LOOP('',(#33189,#33190,#33191,#33192,#33193,#33194));
#5614=EDGE_LOOP('',(#33195,#33196,#33197,#33198,#33199,#33200));
#5615=EDGE_LOOP('',(#33201,#33202,#33203,#33204,#33205,#33206));
#5616=EDGE_LOOP('',(#33207,#33208,#33209,#33210,#33211,#33212));
#5617=EDGE_LOOP('',(#33213,#33214,#33215,#33216,#33217,#33218));
#5618=EDGE_LOOP('',(#33219,#33220,#33221,#33222,#33223,#33224));
#5619=EDGE_LOOP('',(#33225,#33226,#33227,#33228,#33229,#33230));
#5620=EDGE_LOOP('',(#33231,#33232,#33233,#33234,#33235,#33236));
#5621=EDGE_LOOP('',(#33237,#33238,#33239,#33240,#33241,#33242));
#5622=EDGE_LOOP('',(#33243,#33244,#33245,#33246,#33247,#33248));
#5623=EDGE_LOOP('',(#33249,#33250,#33251,#33252,#33253,#33254));
#5624=EDGE_LOOP('',(#33255,#33256,#33257,#33258));
#5625=EDGE_LOOP('',(#33259,#33260,#33261,#33262));
#5626=EDGE_LOOP('',(#33263,#33264,#33265,#33266));
#5627=EDGE_LOOP('',(#33267,#33268,#33269,#33270));
#5628=EDGE_LOOP('',(#33271,#33272,#33273,#33274));
#5629=EDGE_LOOP('',(#33275,#33276,#33277,#33278));
#5630=EDGE_LOOP('',(#33279,#33280,#33281,#33282));
#5631=EDGE_LOOP('',(#33283,#33284,#33285,#33286));
#5632=EDGE_LOOP('',(#33287,#33288,#33289,#33290));
#5633=EDGE_LOOP('',(#33291,#33292,#33293,#33294));
#5634=EDGE_LOOP('',(#33295,#33296,#33297,#33298));
#5635=EDGE_LOOP('',(#33299,#33300,#33301,#33302));
#5636=EDGE_LOOP('',(#33303,#33304,#33305,#33306));
#5637=EDGE_LOOP('',(#33307,#33308,#33309,#33310));
#5638=EDGE_LOOP('',(#33311,#33312,#33313,#33314));
#5639=EDGE_LOOP('',(#33315,#33316,#33317,#33318));
#5640=EDGE_LOOP('',(#33319,#33320,#33321,#33322));
#5641=EDGE_LOOP('',(#33323,#33324,#33325,#33326));
#5642=EDGE_LOOP('',(#33327,#33328,#33329,#33330));
#5643=EDGE_LOOP('',(#33331,#33332,#33333,#33334));
#5644=EDGE_LOOP('',(#33335,#33336,#33337,#33338));
#5645=EDGE_LOOP('',(#33339,#33340,#33341,#33342));
#5646=EDGE_LOOP('',(#33343,#33344,#33345,#33346));
#5647=EDGE_LOOP('',(#33347,#33348,#33349,#33350));
#5648=EDGE_LOOP('',(#33351,#33352,#33353,#33354));
#5649=EDGE_LOOP('',(#33355,#33356,#33357,#33358));
#5650=EDGE_LOOP('',(#33359,#33360,#33361,#33362));
#5651=EDGE_LOOP('',(#33363,#33364,#33365,#33366));
#5652=EDGE_LOOP('',(#33367,#33368,#33369,#33370));
#5653=EDGE_LOOP('',(#33371,#33372,#33373,#33374));
#5654=EDGE_LOOP('',(#33375,#33376,#33377,#33378));
#5655=EDGE_LOOP('',(#33379,#33380,#33381,#33382));
#5656=EDGE_LOOP('',(#33383,#33384,#33385,#33386));
#5657=EDGE_LOOP('',(#33387,#33388,#33389,#33390));
#5658=EDGE_LOOP('',(#33391,#33392,#33393,#33394));
#5659=EDGE_LOOP('',(#33395,#33396,#33397,#33398));
#5660=EDGE_LOOP('',(#33399,#33400,#33401,#33402));
#5661=EDGE_LOOP('',(#33403,#33404,#33405,#33406));
#5662=EDGE_LOOP('',(#33407,#33408,#33409,#33410));
#5663=EDGE_LOOP('',(#33411,#33412,#33413,#33414));
#5664=EDGE_LOOP('',(#33415,#33416,#33417,#33418));
#5665=EDGE_LOOP('',(#33419,#33420,#33421,#33422));
#5666=EDGE_LOOP('',(#33423,#33424,#33425,#33426));
#5667=EDGE_LOOP('',(#33427,#33428,#33429,#33430));
#5668=EDGE_LOOP('',(#33431,#33432,#33433,#33434));
#5669=EDGE_LOOP('',(#33435,#33436,#33437,#33438));
#5670=EDGE_LOOP('',(#33439,#33440,#33441,#33442));
#5671=EDGE_LOOP('',(#33443,#33444,#33445,#33446));
#5672=EDGE_LOOP('',(#33447,#33448,#33449,#33450));
#5673=EDGE_LOOP('',(#33451,#33452,#33453,#33454));
#5674=EDGE_LOOP('',(#33455,#33456,#33457,#33458));
#5675=EDGE_LOOP('',(#33459,#33460,#33461,#33462));
#5676=EDGE_LOOP('',(#33463,#33464,#33465,#33466));
#5677=EDGE_LOOP('',(#33467,#33468,#33469,#33470));
#5678=EDGE_LOOP('',(#33471,#33472,#33473,#33474));
#5679=EDGE_LOOP('',(#33475,#33476,#33477,#33478));
#5680=EDGE_LOOP('',(#33479,#33480,#33481,#33482));
#5681=EDGE_LOOP('',(#33483,#33484,#33485,#33486));
#5682=EDGE_LOOP('',(#33487,#33488,#33489,#33490));
#5683=EDGE_LOOP('',(#33491,#33492,#33493,#33494));
#5684=EDGE_LOOP('',(#33495,#33496,#33497,#33498));
#5685=EDGE_LOOP('',(#33499,#33500,#33501,#33502));
#5686=EDGE_LOOP('',(#33503,#33504,#33505,#33506));
#5687=EDGE_LOOP('',(#33507,#33508,#33509,#33510));
#5688=EDGE_LOOP('',(#33511,#33512,#33513,#33514));
#5689=EDGE_LOOP('',(#33515,#33516,#33517,#33518));
#5690=EDGE_LOOP('',(#33519,#33520,#33521,#33522));
#5691=EDGE_LOOP('',(#33523,#33524,#33525,#33526));
#5692=EDGE_LOOP('',(#33527,#33528,#33529,#33530));
#5693=EDGE_LOOP('',(#33531,#33532,#33533,#33534));
#5694=EDGE_LOOP('',(#33535,#33536,#33537,#33538));
#5695=EDGE_LOOP('',(#33539,#33540,#33541,#33542));
#5696=EDGE_LOOP('',(#33543,#33544,#33545,#33546));
#5697=EDGE_LOOP('',(#33547,#33548,#33549,#33550));
#5698=EDGE_LOOP('',(#33551,#33552,#33553,#33554));
#5699=EDGE_LOOP('',(#33555,#33556,#33557,#33558));
#5700=EDGE_LOOP('',(#33559,#33560,#33561,#33562));
#5701=EDGE_LOOP('',(#33563,#33564,#33565,#33566));
#5702=EDGE_LOOP('',(#33567,#33568,#33569,#33570));
#5703=EDGE_LOOP('',(#33571,#33572,#33573,#33574));
#5704=EDGE_LOOP('',(#33575,#33576,#33577,#33578));
#5705=EDGE_LOOP('',(#33579,#33580,#33581,#33582));
#5706=EDGE_LOOP('',(#33583,#33584,#33585,#33586));
#5707=EDGE_LOOP('',(#33587,#33588,#33589,#33590));
#5708=EDGE_LOOP('',(#33591,#33592,#33593,#33594));
#5709=EDGE_LOOP('',(#33595,#33596,#33597,#33598));
#5710=EDGE_LOOP('',(#33599,#33600,#33601,#33602));
#5711=EDGE_LOOP('',(#33603,#33604,#33605,#33606));
#5712=EDGE_LOOP('',(#33607,#33608,#33609,#33610));
#5713=EDGE_LOOP('',(#33611,#33612,#33613,#33614));
#5714=EDGE_LOOP('',(#33615,#33616,#33617,#33618));
#5715=EDGE_LOOP('',(#33619,#33620,#33621,#33622));
#5716=EDGE_LOOP('',(#33623,#33624,#33625,#33626));
#5717=EDGE_LOOP('',(#33627,#33628,#33629,#33630));
#5718=EDGE_LOOP('',(#33631,#33632,#33633,#33634));
#5719=EDGE_LOOP('',(#33635,#33636,#33637,#33638));
#5720=EDGE_LOOP('',(#33639,#33640,#33641,#33642));
#5721=EDGE_LOOP('',(#33643,#33644,#33645,#33646));
#5722=EDGE_LOOP('',(#33647,#33648,#33649,#33650));
#5723=EDGE_LOOP('',(#33651,#33652,#33653,#33654));
#5724=EDGE_LOOP('',(#33655,#33656,#33657,#33658));
#5725=EDGE_LOOP('',(#33659,#33660,#33661,#33662));
#5726=EDGE_LOOP('',(#33663,#33664,#33665,#33666));
#5727=EDGE_LOOP('',(#33667,#33668,#33669,#33670));
#5728=EDGE_LOOP('',(#33671,#33672,#33673,#33674));
#5729=EDGE_LOOP('',(#33675,#33676,#33677,#33678));
#5730=EDGE_LOOP('',(#33679,#33680,#33681,#33682));
#5731=EDGE_LOOP('',(#33683,#33684,#33685,#33686));
#5732=EDGE_LOOP('',(#33687,#33688,#33689,#33690));
#5733=EDGE_LOOP('',(#33691,#33692,#33693,#33694));
#5734=EDGE_LOOP('',(#33695,#33696,#33697,#33698));
#5735=EDGE_LOOP('',(#33699,#33700,#33701,#33702));
#5736=EDGE_LOOP('',(#33703,#33704,#33705,#33706));
#5737=EDGE_LOOP('',(#33707,#33708,#33709,#33710));
#5738=EDGE_LOOP('',(#33711,#33712,#33713,#33714));
#5739=EDGE_LOOP('',(#33715,#33716,#33717,#33718));
#5740=EDGE_LOOP('',(#33719,#33720,#33721,#33722));
#5741=EDGE_LOOP('',(#33723,#33724,#33725,#33726));
#5742=EDGE_LOOP('',(#33727,#33728,#33729,#33730));
#5743=EDGE_LOOP('',(#33731,#33732,#33733,#33734));
#5744=EDGE_LOOP('',(#33735,#33736,#33737,#33738));
#5745=EDGE_LOOP('',(#33739,#33740,#33741,#33742));
#5746=EDGE_LOOP('',(#33743,#33744,#33745,#33746));
#5747=EDGE_LOOP('',(#33747,#33748,#33749,#33750));
#5748=EDGE_LOOP('',(#33751,#33752,#33753,#33754));
#5749=EDGE_LOOP('',(#33755,#33756,#33757,#33758));
#5750=EDGE_LOOP('',(#33759,#33760,#33761,#33762));
#5751=EDGE_LOOP('',(#33763,#33764,#33765,#33766));
#5752=EDGE_LOOP('',(#33767,#33768,#33769,#33770));
#5753=EDGE_LOOP('',(#33771,#33772,#33773,#33774));
#5754=EDGE_LOOP('',(#33775,#33776,#33777,#33778));
#5755=EDGE_LOOP('',(#33779,#33780,#33781,#33782));
#5756=EDGE_LOOP('',(#33783,#33784,#33785,#33786));
#5757=EDGE_LOOP('',(#33787,#33788,#33789,#33790));
#5758=EDGE_LOOP('',(#33791,#33792,#33793,#33794));
#5759=EDGE_LOOP('',(#33795,#33796,#33797,#33798));
#5760=EDGE_LOOP('',(#33799,#33800,#33801,#33802));
#5761=EDGE_LOOP('',(#33803,#33804,#33805,#33806));
#5762=EDGE_LOOP('',(#33807,#33808,#33809,#33810));
#5763=EDGE_LOOP('',(#33811,#33812,#33813,#33814));
#5764=EDGE_LOOP('',(#33815,#33816,#33817,#33818));
#5765=EDGE_LOOP('',(#33819,#33820,#33821,#33822));
#5766=EDGE_LOOP('',(#33823,#33824,#33825,#33826));
#5767=EDGE_LOOP('',(#33827,#33828,#33829,#33830));
#5768=EDGE_LOOP('',(#33831,#33832,#33833,#33834));
#5769=EDGE_LOOP('',(#33835,#33836,#33837,#33838));
#5770=EDGE_LOOP('',(#33839,#33840,#33841,#33842));
#5771=EDGE_LOOP('',(#33843,#33844,#33845,#33846));
#5772=EDGE_LOOP('',(#33847,#33848,#33849,#33850));
#5773=EDGE_LOOP('',(#33851,#33852,#33853,#33854));
#5774=EDGE_LOOP('',(#33855,#33856,#33857,#33858));
#5775=EDGE_LOOP('',(#33859,#33860,#33861,#33862));
#5776=EDGE_LOOP('',(#33863,#33864,#33865,#33866));
#5777=EDGE_LOOP('',(#33867,#33868,#33869,#33870));
#5778=EDGE_LOOP('',(#33871,#33872,#33873,#33874));
#5779=EDGE_LOOP('',(#33875,#33876,#33877,#33878));
#5780=EDGE_LOOP('',(#33879,#33880,#33881,#33882));
#5781=EDGE_LOOP('',(#33883,#33884,#33885,#33886));
#5782=EDGE_LOOP('',(#33887,#33888,#33889,#33890));
#5783=EDGE_LOOP('',(#33891,#33892,#33893,#33894));
#5784=EDGE_LOOP('',(#33895,#33896,#33897,#33898));
#5785=EDGE_LOOP('',(#33899,#33900,#33901,#33902));
#5786=EDGE_LOOP('',(#33903,#33904,#33905,#33906));
#5787=EDGE_LOOP('',(#33907,#33908,#33909,#33910));
#5788=EDGE_LOOP('',(#33911,#33912,#33913,#33914));
#5789=EDGE_LOOP('',(#33915,#33916,#33917,#33918));
#5790=EDGE_LOOP('',(#33919,#33920,#33921,#33922));
#5791=EDGE_LOOP('',(#33923,#33924,#33925,#33926));
#5792=EDGE_LOOP('',(#33927,#33928,#33929,#33930));
#5793=EDGE_LOOP('',(#33931,#33932,#33933,#33934));
#5794=EDGE_LOOP('',(#33935,#33936,#33937,#33938));
#5795=EDGE_LOOP('',(#33939,#33940,#33941,#33942));
#5796=EDGE_LOOP('',(#33943,#33944,#33945,#33946));
#5797=EDGE_LOOP('',(#33947,#33948,#33949,#33950));
#5798=EDGE_LOOP('',(#33951,#33952,#33953,#33954));
#5799=EDGE_LOOP('',(#33955,#33956,#33957,#33958));
#5800=EDGE_LOOP('',(#33959,#33960,#33961,#33962));
#5801=EDGE_LOOP('',(#33963,#33964,#33965,#33966));
#5802=EDGE_LOOP('',(#33967,#33968,#33969,#33970));
#5803=EDGE_LOOP('',(#33971,#33972,#33973,#33974));
#5804=EDGE_LOOP('',(#33975,#33976,#33977,#33978));
#5805=EDGE_LOOP('',(#33979,#33980,#33981,#33982));
#5806=EDGE_LOOP('',(#33983,#33984,#33985,#33986));
#5807=EDGE_LOOP('',(#33987,#33988,#33989,#33990));
#5808=EDGE_LOOP('',(#33991,#33992,#33993,#33994));
#5809=EDGE_LOOP('',(#33995,#33996,#33997,#33998));
#5810=EDGE_LOOP('',(#33999,#34000,#34001,#34002));
#5811=EDGE_LOOP('',(#34003,#34004,#34005,#34006));
#5812=EDGE_LOOP('',(#34007,#34008,#34009,#34010));
#5813=EDGE_LOOP('',(#34011,#34012,#34013,#34014));
#5814=EDGE_LOOP('',(#34015,#34016,#34017,#34018));
#5815=EDGE_LOOP('',(#34019,#34020,#34021,#34022));
#5816=EDGE_LOOP('',(#34023,#34024,#34025,#34026));
#5817=EDGE_LOOP('',(#34027,#34028,#34029,#34030));
#5818=EDGE_LOOP('',(#34031,#34032,#34033,#34034));
#5819=EDGE_LOOP('',(#34035,#34036,#34037,#34038));
#5820=EDGE_LOOP('',(#34039,#34040,#34041,#34042));
#5821=EDGE_LOOP('',(#34043,#34044,#34045,#34046));
#5822=EDGE_LOOP('',(#34047,#34048,#34049,#34050));
#5823=EDGE_LOOP('',(#34051,#34052,#34053,#34054));
#5824=EDGE_LOOP('',(#34055,#34056,#34057,#34058));
#5825=EDGE_LOOP('',(#34059,#34060,#34061,#34062));
#5826=EDGE_LOOP('',(#34063,#34064,#34065,#34066));
#5827=EDGE_LOOP('',(#34067,#34068,#34069,#34070));
#5828=EDGE_LOOP('',(#34071,#34072,#34073,#34074));
#5829=EDGE_LOOP('',(#34075,#34076,#34077,#34078));
#5830=EDGE_LOOP('',(#34079,#34080,#34081,#34082));
#5831=EDGE_LOOP('',(#34083,#34084,#34085,#34086));
#5832=EDGE_LOOP('',(#34087,#34088,#34089,#34090));
#5833=EDGE_LOOP('',(#34091,#34092,#34093,#34094));
#5834=EDGE_LOOP('',(#34095,#34096,#34097,#34098));
#5835=EDGE_LOOP('',(#34099,#34100,#34101,#34102));
#5836=EDGE_LOOP('',(#34103,#34104,#34105,#34106));
#5837=EDGE_LOOP('',(#34107,#34108,#34109,#34110));
#5838=EDGE_LOOP('',(#34111,#34112,#34113,#34114));
#5839=EDGE_LOOP('',(#34115,#34116,#34117,#34118));
#5840=EDGE_LOOP('',(#34119,#34120,#34121,#34122));
#5841=EDGE_LOOP('',(#34123,#34124,#34125,#34126));
#5842=EDGE_LOOP('',(#34127,#34128,#34129,#34130));
#5843=EDGE_LOOP('',(#34131,#34132,#34133,#34134));
#5844=EDGE_LOOP('',(#34135,#34136,#34137,#34138));
#5845=EDGE_LOOP('',(#34139,#34140,#34141,#34142));
#5846=EDGE_LOOP('',(#34143,#34144,#34145,#34146));
#5847=EDGE_LOOP('',(#34147,#34148,#34149,#34150));
#5848=EDGE_LOOP('',(#34151,#34152,#34153,#34154));
#5849=EDGE_LOOP('',(#34155,#34156,#34157,#34158));
#5850=EDGE_LOOP('',(#34159,#34160,#34161,#34162));
#5851=EDGE_LOOP('',(#34163,#34164,#34165,#34166));
#5852=EDGE_LOOP('',(#34167,#34168,#34169,#34170));
#5853=EDGE_LOOP('',(#34171,#34172,#34173,#34174));
#5854=EDGE_LOOP('',(#34175,#34176,#34177,#34178));
#5855=EDGE_LOOP('',(#34179,#34180,#34181,#34182));
#5856=EDGE_LOOP('',(#34183,#34184,#34185,#34186));
#5857=EDGE_LOOP('',(#34187,#34188,#34189,#34190));
#5858=EDGE_LOOP('',(#34191,#34192,#34193,#34194));
#5859=EDGE_LOOP('',(#34195,#34196,#34197,#34198));
#5860=EDGE_LOOP('',(#34199,#34200,#34201,#34202));
#5861=EDGE_LOOP('',(#34203,#34204,#34205,#34206));
#5862=EDGE_LOOP('',(#34207,#34208,#34209,#34210));
#5863=EDGE_LOOP('',(#34211,#34212,#34213,#34214));
#5864=EDGE_LOOP('',(#34215,#34216,#34217,#34218));
#5865=EDGE_LOOP('',(#34219,#34220,#34221,#34222));
#5866=EDGE_LOOP('',(#34223,#34224,#34225,#34226));
#5867=EDGE_LOOP('',(#34227,#34228,#34229,#34230));
#5868=EDGE_LOOP('',(#34231,#34232,#34233,#34234));
#5869=EDGE_LOOP('',(#34235,#34236,#34237,#34238));
#5870=EDGE_LOOP('',(#34239,#34240,#34241,#34242));
#5871=EDGE_LOOP('',(#34243,#34244,#34245,#34246));
#5872=EDGE_LOOP('',(#34247,#34248,#34249,#34250));
#5873=EDGE_LOOP('',(#34251,#34252,#34253,#34254));
#5874=EDGE_LOOP('',(#34255,#34256,#34257,#34258));
#5875=EDGE_LOOP('',(#34259,#34260,#34261,#34262));
#5876=EDGE_LOOP('',(#34263,#34264,#34265,#34266));
#5877=EDGE_LOOP('',(#34267,#34268,#34269,#34270));
#5878=EDGE_LOOP('',(#34271,#34272,#34273,#34274));
#5879=EDGE_LOOP('',(#34275,#34276,#34277,#34278));
#5880=EDGE_LOOP('',(#34279,#34280,#34281,#34282));
#5881=EDGE_LOOP('',(#34283,#34284,#34285,#34286));
#5882=EDGE_LOOP('',(#34287,#34288,#34289,#34290));
#5883=EDGE_LOOP('',(#34291,#34292,#34293,#34294));
#5884=EDGE_LOOP('',(#34295,#34296,#34297,#34298));
#5885=EDGE_LOOP('',(#34299,#34300,#34301,#34302));
#5886=EDGE_LOOP('',(#34303,#34304,#34305,#34306));
#5887=EDGE_LOOP('',(#34307,#34308,#34309,#34310));
#5888=EDGE_LOOP('',(#34311,#34312,#34313,#34314));
#5889=EDGE_LOOP('',(#34315,#34316,#34317,#34318));
#5890=EDGE_LOOP('',(#34319,#34320,#34321,#34322));
#5891=EDGE_LOOP('',(#34323,#34324,#34325,#34326));
#5892=EDGE_LOOP('',(#34327,#34328,#34329,#34330));
#5893=EDGE_LOOP('',(#34331,#34332,#34333,#34334));
#5894=EDGE_LOOP('',(#34335,#34336,#34337,#34338));
#5895=EDGE_LOOP('',(#34339,#34340,#34341,#34342));
#5896=EDGE_LOOP('',(#34343,#34344,#34345,#34346));
#5897=EDGE_LOOP('',(#34347,#34348,#34349,#34350));
#5898=EDGE_LOOP('',(#34351,#34352,#34353,#34354));
#5899=EDGE_LOOP('',(#34355,#34356,#34357,#34358));
#5900=EDGE_LOOP('',(#34359,#34360,#34361,#34362));
#5901=EDGE_LOOP('',(#34363,#34364,#34365,#34366));
#5902=EDGE_LOOP('',(#34367,#34368,#34369,#34370));
#5903=EDGE_LOOP('',(#34371,#34372,#34373,#34374));
#5904=EDGE_LOOP('',(#34375,#34376,#34377,#34378));
#5905=EDGE_LOOP('',(#34379,#34380,#34381,#34382));
#5906=EDGE_LOOP('',(#34383,#34384,#34385,#34386));
#5907=EDGE_LOOP('',(#34387,#34388,#34389,#34390));
#5908=EDGE_LOOP('',(#34391,#34392,#34393,#34394));
#5909=EDGE_LOOP('',(#34395,#34396,#34397,#34398));
#5910=EDGE_LOOP('',(#34399,#34400,#34401,#34402));
#5911=EDGE_LOOP('',(#34403,#34404,#34405,#34406));
#5912=EDGE_LOOP('',(#34407,#34408,#34409,#34410));
#5913=EDGE_LOOP('',(#34411,#34412,#34413,#34414));
#5914=EDGE_LOOP('',(#34415,#34416,#34417,#34418));
#5915=EDGE_LOOP('',(#34419,#34420,#34421,#34422));
#5916=EDGE_LOOP('',(#34423,#34424,#34425,#34426));
#5917=EDGE_LOOP('',(#34427,#34428,#34429,#34430));
#5918=EDGE_LOOP('',(#34431,#34432,#34433,#34434));
#5919=EDGE_LOOP('',(#34435,#34436,#34437,#34438));
#5920=EDGE_LOOP('',(#34439,#34440,#34441,#34442));
#5921=EDGE_LOOP('',(#34443,#34444,#34445,#34446));
#5922=EDGE_LOOP('',(#34447,#34448,#34449,#34450));
#5923=EDGE_LOOP('',(#34451,#34452,#34453,#34454));
#5924=EDGE_LOOP('',(#34455,#34456,#34457,#34458));
#5925=EDGE_LOOP('',(#34459,#34460,#34461,#34462));
#5926=EDGE_LOOP('',(#34463,#34464,#34465,#34466));
#5927=EDGE_LOOP('',(#34467,#34468,#34469,#34470));
#5928=EDGE_LOOP('',(#34471,#34472,#34473,#34474));
#5929=EDGE_LOOP('',(#34475,#34476,#34477,#34478));
#5930=EDGE_LOOP('',(#34479,#34480,#34481,#34482));
#5931=EDGE_LOOP('',(#34483,#34484,#34485,#34486));
#5932=EDGE_LOOP('',(#34487,#34488,#34489,#34490));
#5933=EDGE_LOOP('',(#34491,#34492,#34493,#34494));
#5934=EDGE_LOOP('',(#34495,#34496,#34497,#34498));
#5935=EDGE_LOOP('',(#34499,#34500,#34501,#34502));
#5936=EDGE_LOOP('',(#34503,#34504,#34505,#34506));
#5937=EDGE_LOOP('',(#34507,#34508,#34509,#34510));
#5938=EDGE_LOOP('',(#34511,#34512,#34513,#34514));
#5939=EDGE_LOOP('',(#34515,#34516,#34517,#34518));
#5940=EDGE_LOOP('',(#34519,#34520,#34521,#34522));
#5941=EDGE_LOOP('',(#34523,#34524,#34525,#34526));
#5942=EDGE_LOOP('',(#34527,#34528,#34529,#34530));
#5943=EDGE_LOOP('',(#34531,#34532,#34533,#34534));
#5944=EDGE_LOOP('',(#34535,#34536,#34537,#34538));
#5945=EDGE_LOOP('',(#34539,#34540,#34541,#34542));
#5946=EDGE_LOOP('',(#34543,#34544,#34545,#34546));
#5947=EDGE_LOOP('',(#34547,#34548,#34549,#34550));
#5948=EDGE_LOOP('',(#34551,#34552,#34553,#34554));
#5949=EDGE_LOOP('',(#34555,#34556,#34557,#34558));
#5950=EDGE_LOOP('',(#34559,#34560,#34561,#34562));
#5951=EDGE_LOOP('',(#34563,#34564,#34565,#34566));
#5952=EDGE_LOOP('',(#34567,#34568,#34569,#34570));
#5953=EDGE_LOOP('',(#34571,#34572,#34573,#34574));
#5954=EDGE_LOOP('',(#34575,#34576,#34577,#34578));
#5955=EDGE_LOOP('',(#34579,#34580,#34581,#34582));
#5956=EDGE_LOOP('',(#34583,#34584,#34585,#34586));
#5957=EDGE_LOOP('',(#34587,#34588,#34589,#34590));
#5958=EDGE_LOOP('',(#34591,#34592,#34593,#34594));
#5959=EDGE_LOOP('',(#34595,#34596,#34597,#34598));
#5960=EDGE_LOOP('',(#34599,#34600,#34601,#34602));
#5961=EDGE_LOOP('',(#34603,#34604,#34605,#34606));
#5962=EDGE_LOOP('',(#34607,#34608,#34609,#34610));
#5963=EDGE_LOOP('',(#34611,#34612,#34613,#34614));
#5964=EDGE_LOOP('',(#34615,#34616,#34617,#34618));
#5965=EDGE_LOOP('',(#34619,#34620,#34621,#34622));
#5966=EDGE_LOOP('',(#34623,#34624,#34625,#34626));
#5967=EDGE_LOOP('',(#34627,#34628,#34629,#34630));
#5968=EDGE_LOOP('',(#34631,#34632,#34633,#34634));
#5969=EDGE_LOOP('',(#34635,#34636,#34637,#34638));
#5970=EDGE_LOOP('',(#34639,#34640,#34641,#34642));
#5971=EDGE_LOOP('',(#34643,#34644,#34645,#34646));
#5972=EDGE_LOOP('',(#34647,#34648,#34649,#34650));
#5973=EDGE_LOOP('',(#34651,#34652,#34653,#34654));
#5974=EDGE_LOOP('',(#34655,#34656,#34657,#34658));
#5975=EDGE_LOOP('',(#34659,#34660,#34661,#34662));
#5976=EDGE_LOOP('',(#34663,#34664,#34665,#34666));
#5977=EDGE_LOOP('',(#34667,#34668,#34669,#34670));
#5978=EDGE_LOOP('',(#34671,#34672,#34673,#34674));
#5979=EDGE_LOOP('',(#34675,#34676,#34677,#34678));
#5980=EDGE_LOOP('',(#34679,#34680,#34681,#34682));
#5981=EDGE_LOOP('',(#34683,#34684,#34685,#34686));
#5982=EDGE_LOOP('',(#34687,#34688,#34689,#34690));
#5983=EDGE_LOOP('',(#34691,#34692,#34693,#34694));
#5984=EDGE_LOOP('',(#34695,#34696,#34697,#34698));
#5985=EDGE_LOOP('',(#34699,#34700,#34701,#34702));
#5986=EDGE_LOOP('',(#34703,#34704,#34705,#34706));
#5987=EDGE_LOOP('',(#34707,#34708,#34709,#34710));
#5988=EDGE_LOOP('',(#34711,#34712,#34713,#34714));
#5989=EDGE_LOOP('',(#34715,#34716,#34717,#34718));
#5990=EDGE_LOOP('',(#34719,#34720,#34721,#34722));
#5991=EDGE_LOOP('',(#34723,#34724,#34725,#34726));
#5992=EDGE_LOOP('',(#34727,#34728,#34729,#34730));
#5993=EDGE_LOOP('',(#34731,#34732,#34733,#34734));
#5994=EDGE_LOOP('',(#34735,#34736,#34737,#34738));
#5995=EDGE_LOOP('',(#34739,#34740,#34741,#34742));
#5996=EDGE_LOOP('',(#34743,#34744,#34745,#34746));
#5997=EDGE_LOOP('',(#34747,#34748,#34749,#34750));
#5998=EDGE_LOOP('',(#34751,#34752,#34753,#34754));
#5999=EDGE_LOOP('',(#34755,#34756,#34757,#34758));
#6000=EDGE_LOOP('',(#34759,#34760,#34761,#34762));
#6001=EDGE_LOOP('',(#34763,#34764,#34765,#34766));
#6002=EDGE_LOOP('',(#34767,#34768,#34769,#34770));
#6003=EDGE_LOOP('',(#34771,#34772,#34773,#34774));
#6004=EDGE_LOOP('',(#34775,#34776,#34777,#34778));
#6005=EDGE_LOOP('',(#34779,#34780,#34781,#34782));
#6006=EDGE_LOOP('',(#34783,#34784,#34785,#34786));
#6007=EDGE_LOOP('',(#34787,#34788,#34789,#34790));
#6008=EDGE_LOOP('',(#34791,#34792,#34793,#34794));
#6009=EDGE_LOOP('',(#34795,#34796,#34797,#34798));
#6010=EDGE_LOOP('',(#34799,#34800,#34801,#34802));
#6011=EDGE_LOOP('',(#34803,#34804,#34805,#34806));
#6012=EDGE_LOOP('',(#34807,#34808,#34809,#34810));
#6013=EDGE_LOOP('',(#34811,#34812,#34813,#34814));
#6014=EDGE_LOOP('',(#34815,#34816,#34817,#34818));
#6015=EDGE_LOOP('',(#34819,#34820,#34821,#34822));
#6016=EDGE_LOOP('',(#34823,#34824,#34825,#34826));
#6017=EDGE_LOOP('',(#34827,#34828,#34829,#34830));
#6018=EDGE_LOOP('',(#34831,#34832,#34833,#34834));
#6019=EDGE_LOOP('',(#34835,#34836,#34837,#34838));
#6020=EDGE_LOOP('',(#34839,#34840,#34841,#34842));
#6021=EDGE_LOOP('',(#34843,#34844,#34845,#34846));
#6022=EDGE_LOOP('',(#34847,#34848,#34849,#34850));
#6023=EDGE_LOOP('',(#34851,#34852,#34853,#34854));
#6024=EDGE_LOOP('',(#34855,#34856,#34857,#34858));
#6025=EDGE_LOOP('',(#34859,#34860,#34861,#34862));
#6026=EDGE_LOOP('',(#34863,#34864,#34865,#34866));
#6027=EDGE_LOOP('',(#34867,#34868,#34869,#34870));
#6028=EDGE_LOOP('',(#34871,#34872,#34873,#34874));
#6029=EDGE_LOOP('',(#34875,#34876,#34877,#34878));
#6030=EDGE_LOOP('',(#34879,#34880,#34881,#34882));
#6031=EDGE_LOOP('',(#34883,#34884,#34885,#34886));
#6032=EDGE_LOOP('',(#34887,#34888,#34889,#34890));
#6033=EDGE_LOOP('',(#34891,#34892,#34893,#34894));
#6034=EDGE_LOOP('',(#34895,#34896,#34897,#34898));
#6035=EDGE_LOOP('',(#34899,#34900,#34901,#34902));
#6036=EDGE_LOOP('',(#34903,#34904,#34905,#34906));
#6037=EDGE_LOOP('',(#34907,#34908,#34909,#34910));
#6038=EDGE_LOOP('',(#34911,#34912,#34913,#34914));
#6039=EDGE_LOOP('',(#34915,#34916,#34917,#34918));
#6040=EDGE_LOOP('',(#34919,#34920,#34921,#34922));
#6041=EDGE_LOOP('',(#34923,#34924,#34925,#34926));
#6042=EDGE_LOOP('',(#34927,#34928,#34929,#34930));
#6043=EDGE_LOOP('',(#34931,#34932,#34933,#34934));
#6044=EDGE_LOOP('',(#34935,#34936,#34937,#34938));
#6045=EDGE_LOOP('',(#34939,#34940,#34941,#34942));
#6046=EDGE_LOOP('',(#34943,#34944,#34945,#34946));
#6047=EDGE_LOOP('',(#34947,#34948,#34949,#34950));
#6048=EDGE_LOOP('',(#34951,#34952,#34953,#34954));
#6049=EDGE_LOOP('',(#34955,#34956,#34957,#34958));
#6050=EDGE_LOOP('',(#34959,#34960,#34961,#34962));
#6051=EDGE_LOOP('',(#34963,#34964,#34965,#34966));
#6052=EDGE_LOOP('',(#34967,#34968,#34969,#34970));
#6053=EDGE_LOOP('',(#34971,#34972,#34973,#34974));
#6054=EDGE_LOOP('',(#34975,#34976,#34977,#34978));
#6055=EDGE_LOOP('',(#34979,#34980,#34981,#34982));
#6056=EDGE_LOOP('',(#34983,#34984,#34985,#34986));
#6057=EDGE_LOOP('',(#34987,#34988,#34989,#34990));
#6058=EDGE_LOOP('',(#34991,#34992,#34993,#34994));
#6059=EDGE_LOOP('',(#34995,#34996,#34997,#34998));
#6060=EDGE_LOOP('',(#34999,#35000,#35001,#35002));
#6061=EDGE_LOOP('',(#35003,#35004,#35005,#35006));
#6062=EDGE_LOOP('',(#35007,#35008,#35009,#35010));
#6063=EDGE_LOOP('',(#35011,#35012,#35013,#35014));
#6064=EDGE_LOOP('',(#35015,#35016,#35017,#35018));
#6065=EDGE_LOOP('',(#35019,#35020,#35021,#35022));
#6066=EDGE_LOOP('',(#35023,#35024,#35025,#35026));
#6067=EDGE_LOOP('',(#35027,#35028,#35029,#35030));
#6068=EDGE_LOOP('',(#35031,#35032,#35033,#35034));
#6069=EDGE_LOOP('',(#35035,#35036,#35037,#35038));
#6070=EDGE_LOOP('',(#35039,#35040,#35041,#35042));
#6071=EDGE_LOOP('',(#35043,#35044,#35045,#35046));
#6072=EDGE_LOOP('',(#35047,#35048,#35049,#35050));
#6073=EDGE_LOOP('',(#35051,#35052,#35053,#35054));
#6074=EDGE_LOOP('',(#35055,#35056,#35057,#35058));
#6075=EDGE_LOOP('',(#35059,#35060,#35061,#35062));
#6076=EDGE_LOOP('',(#35063,#35064,#35065,#35066));
#6077=EDGE_LOOP('',(#35067,#35068,#35069,#35070));
#6078=EDGE_LOOP('',(#35071,#35072,#35073,#35074));
#6079=EDGE_LOOP('',(#35075,#35076,#35077,#35078));
#6080=EDGE_LOOP('',(#35079,#35080,#35081,#35082));
#6081=EDGE_LOOP('',(#35083,#35084,#35085,#35086));
#6082=EDGE_LOOP('',(#35087,#35088,#35089,#35090));
#6083=EDGE_LOOP('',(#35091,#35092,#35093,#35094));
#6084=EDGE_LOOP('',(#35095,#35096,#35097,#35098));
#6085=EDGE_LOOP('',(#35099,#35100,#35101,#35102));
#6086=EDGE_LOOP('',(#35103,#35104,#35105,#35106));
#6087=EDGE_LOOP('',(#35107,#35108,#35109,#35110));
#6088=EDGE_LOOP('',(#35111,#35112,#35113,#35114));
#6089=EDGE_LOOP('',(#35115,#35116,#35117,#35118));
#6090=EDGE_LOOP('',(#35119,#35120,#35121,#35122));
#6091=EDGE_LOOP('',(#35123,#35124,#35125,#35126));
#6092=EDGE_LOOP('',(#35127,#35128,#35129,#35130));
#6093=EDGE_LOOP('',(#35131,#35132,#35133,#35134));
#6094=EDGE_LOOP('',(#35135,#35136,#35137,#35138));
#6095=EDGE_LOOP('',(#35139,#35140,#35141,#35142));
#6096=EDGE_LOOP('',(#35143,#35144,#35145,#35146));
#6097=EDGE_LOOP('',(#35147,#35148,#35149,#35150));
#6098=EDGE_LOOP('',(#35151,#35152,#35153,#35154));
#6099=EDGE_LOOP('',(#35155,#35156,#35157,#35158));
#6100=EDGE_LOOP('',(#35159,#35160,#35161,#35162));
#6101=EDGE_LOOP('',(#35163,#35164,#35165,#35166));
#6102=EDGE_LOOP('',(#35167,#35168,#35169,#35170));
#6103=EDGE_LOOP('',(#35171,#35172,#35173,#35174));
#6104=EDGE_LOOP('',(#35175,#35176,#35177,#35178));
#6105=EDGE_LOOP('',(#35179,#35180,#35181,#35182));
#6106=EDGE_LOOP('',(#35183,#35184,#35185,#35186));
#6107=EDGE_LOOP('',(#35187,#35188,#35189,#35190));
#6108=EDGE_LOOP('',(#35191,#35192,#35193,#35194));
#6109=EDGE_LOOP('',(#35195,#35196,#35197,#35198));
#6110=EDGE_LOOP('',(#35199,#35200,#35201,#35202));
#6111=EDGE_LOOP('',(#35203,#35204,#35205,#35206));
#6112=EDGE_LOOP('',(#35207,#35208,#35209,#35210));
#6113=EDGE_LOOP('',(#35211,#35212,#35213,#35214));
#6114=EDGE_LOOP('',(#35215,#35216,#35217,#35218));
#6115=EDGE_LOOP('',(#35219,#35220,#35221,#35222));
#6116=EDGE_LOOP('',(#35223,#35224,#35225,#35226));
#6117=EDGE_LOOP('',(#35227,#35228,#35229,#35230));
#6118=EDGE_LOOP('',(#35231,#35232,#35233,#35234));
#6119=EDGE_LOOP('',(#35235,#35236,#35237,#35238));
#6120=EDGE_LOOP('',(#35239,#35240,#35241,#35242));
#6121=EDGE_LOOP('',(#35243,#35244,#35245,#35246));
#6122=EDGE_LOOP('',(#35247,#35248,#35249,#35250));
#6123=EDGE_LOOP('',(#35251,#35252,#35253,#35254));
#6124=EDGE_LOOP('',(#35255,#35256,#35257,#35258));
#6125=EDGE_LOOP('',(#35259,#35260,#35261,#35262));
#6126=EDGE_LOOP('',(#35263,#35264,#35265,#35266));
#6127=EDGE_LOOP('',(#35267,#35268,#35269,#35270));
#6128=EDGE_LOOP('',(#35271,#35272,#35273,#35274));
#6129=EDGE_LOOP('',(#35275,#35276,#35277,#35278));
#6130=EDGE_LOOP('',(#35279,#35280,#35281,#35282));
#6131=EDGE_LOOP('',(#35283,#35284,#35285,#35286));
#6132=EDGE_LOOP('',(#35287,#35288,#35289,#35290));
#6133=EDGE_LOOP('',(#35291,#35292,#35293,#35294));
#6134=EDGE_LOOP('',(#35295,#35296,#35297,#35298));
#6135=EDGE_LOOP('',(#35299,#35300,#35301,#35302));
#6136=EDGE_LOOP('',(#35303,#35304,#35305,#35306));
#6137=EDGE_LOOP('',(#35307,#35308,#35309,#35310));
#6138=EDGE_LOOP('',(#35311,#35312,#35313,#35314));
#6139=EDGE_LOOP('',(#35315,#35316,#35317,#35318));
#6140=EDGE_LOOP('',(#35319,#35320,#35321,#35322));
#6141=EDGE_LOOP('',(#35323,#35324,#35325,#35326));
#6142=EDGE_LOOP('',(#35327,#35328,#35329,#35330));
#6143=EDGE_LOOP('',(#35331,#35332,#35333,#35334));
#6144=EDGE_LOOP('',(#35335,#35336,#35337,#35338));
#6145=EDGE_LOOP('',(#35339,#35340,#35341,#35342));
#6146=EDGE_LOOP('',(#35343,#35344,#35345,#35346));
#6147=EDGE_LOOP('',(#35347,#35348,#35349,#35350));
#6148=EDGE_LOOP('',(#35351,#35352,#35353,#35354));
#6149=EDGE_LOOP('',(#35355,#35356,#35357,#35358));
#6150=EDGE_LOOP('',(#35359,#35360,#35361,#35362));
#6151=EDGE_LOOP('',(#35363,#35364,#35365,#35366));
#6152=EDGE_LOOP('',(#35367,#35368,#35369,#35370));
#6153=EDGE_LOOP('',(#35371,#35372,#35373,#35374));
#6154=EDGE_LOOP('',(#35375,#35376,#35377,#35378));
#6155=EDGE_LOOP('',(#35379,#35380,#35381,#35382));
#6156=EDGE_LOOP('',(#35383,#35384,#35385,#35386));
#6157=EDGE_LOOP('',(#35387,#35388,#35389,#35390));
#6158=EDGE_LOOP('',(#35391,#35392,#35393,#35394));
#6159=EDGE_LOOP('',(#35395,#35396,#35397,#35398));
#6160=EDGE_LOOP('',(#35399,#35400,#35401,#35402));
#6161=EDGE_LOOP('',(#35403,#35404,#35405,#35406));
#6162=EDGE_LOOP('',(#35407,#35408,#35409,#35410));
#6163=EDGE_LOOP('',(#35411,#35412,#35413,#35414));
#6164=EDGE_LOOP('',(#35415,#35416,#35417,#35418));
#6165=EDGE_LOOP('',(#35419,#35420,#35421,#35422));
#6166=EDGE_LOOP('',(#35423,#35424,#35425,#35426));
#6167=EDGE_LOOP('',(#35427,#35428,#35429,#35430));
#6168=EDGE_LOOP('',(#35431,#35432,#35433,#35434));
#6169=EDGE_LOOP('',(#35435,#35436,#35437,#35438));
#6170=EDGE_LOOP('',(#35439,#35440,#35441,#35442));
#6171=EDGE_LOOP('',(#35443,#35444,#35445,#35446));
#6172=EDGE_LOOP('',(#35447,#35448,#35449,#35450));
#6173=EDGE_LOOP('',(#35451,#35452,#35453,#35454));
#6174=EDGE_LOOP('',(#35455,#35456,#35457,#35458));
#6175=EDGE_LOOP('',(#35459,#35460,#35461,#35462));
#6176=EDGE_LOOP('',(#35463,#35464,#35465,#35466));
#6177=EDGE_LOOP('',(#35467,#35468,#35469,#35470));
#6178=EDGE_LOOP('',(#35471,#35472,#35473,#35474));
#6179=EDGE_LOOP('',(#35475,#35476,#35477,#35478));
#6180=EDGE_LOOP('',(#35479,#35480,#35481,#35482));
#6181=EDGE_LOOP('',(#35483,#35484,#35485,#35486));
#6182=EDGE_LOOP('',(#35487,#35488,#35489,#35490));
#6183=EDGE_LOOP('',(#35491,#35492,#35493,#35494));
#6184=EDGE_LOOP('',(#35495,#35496,#35497,#35498));
#6185=EDGE_LOOP('',(#35499,#35500,#35501,#35502));
#6186=EDGE_LOOP('',(#35503,#35504,#35505,#35506));
#6187=EDGE_LOOP('',(#35507,#35508,#35509,#35510));
#6188=EDGE_LOOP('',(#35511,#35512,#35513,#35514));
#6189=EDGE_LOOP('',(#35515,#35516,#35517,#35518));
#6190=EDGE_LOOP('',(#35519,#35520,#35521,#35522));
#6191=EDGE_LOOP('',(#35523,#35524,#35525,#35526));
#6192=EDGE_LOOP('',(#35527,#35528,#35529,#35530));
#6193=EDGE_LOOP('',(#35531,#35532,#35533,#35534));
#6194=EDGE_LOOP('',(#35535,#35536,#35537,#35538));
#6195=EDGE_LOOP('',(#35539,#35540,#35541,#35542));
#6196=EDGE_LOOP('',(#35543,#35544,#35545,#35546));
#6197=EDGE_LOOP('',(#35547,#35548,#35549,#35550));
#6198=EDGE_LOOP('',(#35551,#35552,#35553,#35554));
#6199=EDGE_LOOP('',(#35555,#35556,#35557,#35558));
#6200=EDGE_LOOP('',(#35559,#35560,#35561,#35562));
#6201=EDGE_LOOP('',(#35563,#35564,#35565,#35566));
#6202=EDGE_LOOP('',(#35567,#35568,#35569,#35570));
#6203=EDGE_LOOP('',(#35571,#35572,#35573,#35574));
#6204=EDGE_LOOP('',(#35575,#35576,#35577,#35578));
#6205=EDGE_LOOP('',(#35579,#35580,#35581,#35582));
#6206=EDGE_LOOP('',(#35583,#35584,#35585,#35586));
#6207=EDGE_LOOP('',(#35587,#35588,#35589,#35590));
#6208=EDGE_LOOP('',(#35591,#35592,#35593,#35594));
#6209=EDGE_LOOP('',(#35595,#35596,#35597,#35598));
#6210=EDGE_LOOP('',(#35599,#35600,#35601,#35602));
#6211=EDGE_LOOP('',(#35603,#35604,#35605,#35606));
#6212=EDGE_LOOP('',(#35607,#35608,#35609,#35610));
#6213=EDGE_LOOP('',(#35611,#35612,#35613,#35614));
#6214=EDGE_LOOP('',(#35615,#35616,#35617,#35618));
#6215=EDGE_LOOP('',(#35619,#35620,#35621,#35622));
#6216=EDGE_LOOP('',(#35623,#35624,#35625,#35626));
#6217=EDGE_LOOP('',(#35627,#35628,#35629,#35630));
#6218=EDGE_LOOP('',(#35631,#35632,#35633,#35634));
#6219=EDGE_LOOP('',(#35635,#35636,#35637,#35638));
#6220=EDGE_LOOP('',(#35639,#35640,#35641,#35642));
#6221=EDGE_LOOP('',(#35643,#35644,#35645,#35646));
#6222=EDGE_LOOP('',(#35647,#35648,#35649,#35650));
#6223=EDGE_LOOP('',(#35651,#35652,#35653,#35654));
#6224=EDGE_LOOP('',(#35655,#35656,#35657,#35658));
#6225=EDGE_LOOP('',(#35659,#35660,#35661,#35662));
#6226=EDGE_LOOP('',(#35663,#35664,#35665,#35666));
#6227=EDGE_LOOP('',(#35667,#35668,#35669,#35670));
#6228=EDGE_LOOP('',(#35671,#35672,#35673,#35674));
#6229=EDGE_LOOP('',(#35675,#35676,#35677,#35678));
#6230=EDGE_LOOP('',(#35679,#35680,#35681,#35682));
#6231=EDGE_LOOP('',(#35683,#35684,#35685,#35686));
#6232=EDGE_LOOP('',(#35687,#35688,#35689,#35690));
#6233=EDGE_LOOP('',(#35691,#35692,#35693,#35694));
#6234=EDGE_LOOP('',(#35695,#35696,#35697,#35698));
#6235=EDGE_LOOP('',(#35699,#35700,#35701,#35702));
#6236=EDGE_LOOP('',(#35703,#35704,#35705,#35706));
#6237=EDGE_LOOP('',(#35707,#35708,#35709,#35710));
#6238=EDGE_LOOP('',(#35711,#35712,#35713,#35714));
#6239=EDGE_LOOP('',(#35715,#35716,#35717,#35718));
#6240=EDGE_LOOP('',(#35719,#35720,#35721,#35722));
#6241=EDGE_LOOP('',(#35723,#35724,#35725,#35726));
#6242=EDGE_LOOP('',(#35727,#35728,#35729,#35730));
#6243=EDGE_LOOP('',(#35731,#35732,#35733,#35734));
#6244=EDGE_LOOP('',(#35735,#35736,#35737,#35738));
#6245=EDGE_LOOP('',(#35739,#35740,#35741,#35742));
#6246=EDGE_LOOP('',(#35743,#35744,#35745,#35746));
#6247=EDGE_LOOP('',(#35747,#35748,#35749,#35750));
#6248=EDGE_LOOP('',(#35751,#35752,#35753,#35754));
#6249=EDGE_LOOP('',(#35755,#35756,#35757,#35758));
#6250=EDGE_LOOP('',(#35759,#35760,#35761,#35762));
#6251=EDGE_LOOP('',(#35763,#35764,#35765,#35766));
#6252=EDGE_LOOP('',(#35767,#35768,#35769,#35770));
#6253=EDGE_LOOP('',(#35771,#35772,#35773,#35774));
#6254=EDGE_LOOP('',(#35775,#35776,#35777,#35778));
#6255=EDGE_LOOP('',(#35779,#35780,#35781,#35782));
#6256=EDGE_LOOP('',(#35783,#35784,#35785,#35786));
#6257=EDGE_LOOP('',(#35787,#35788,#35789,#35790));
#6258=EDGE_LOOP('',(#35791,#35792,#35793,#35794));
#6259=EDGE_LOOP('',(#35795,#35796,#35797,#35798));
#6260=EDGE_LOOP('',(#35799,#35800,#35801,#35802));
#6261=EDGE_LOOP('',(#35803,#35804,#35805,#35806));
#6262=EDGE_LOOP('',(#35807,#35808,#35809,#35810));
#6263=EDGE_LOOP('',(#35811,#35812,#35813,#35814));
#6264=EDGE_LOOP('',(#35815,#35816,#35817,#35818));
#6265=EDGE_LOOP('',(#35819,#35820,#35821,#35822));
#6266=EDGE_LOOP('',(#35823,#35824,#35825,#35826));
#6267=EDGE_LOOP('',(#35827,#35828,#35829,#35830));
#6268=EDGE_LOOP('',(#35831,#35832,#35833,#35834));
#6269=EDGE_LOOP('',(#35835,#35836,#35837,#35838));
#6270=EDGE_LOOP('',(#35839,#35840,#35841,#35842));
#6271=EDGE_LOOP('',(#35843,#35844,#35845,#35846));
#6272=EDGE_LOOP('',(#35847,#35848,#35849,#35850));
#6273=EDGE_LOOP('',(#35851,#35852,#35853,#35854));
#6274=EDGE_LOOP('',(#35855,#35856,#35857,#35858));
#6275=EDGE_LOOP('',(#35859,#35860,#35861,#35862));
#6276=EDGE_LOOP('',(#35863,#35864,#35865,#35866));
#6277=EDGE_LOOP('',(#35867,#35868,#35869,#35870));
#6278=EDGE_LOOP('',(#35871,#35872,#35873,#35874));
#6279=EDGE_LOOP('',(#35875,#35876,#35877,#35878));
#6280=EDGE_LOOP('',(#35879,#35880,#35881,#35882));
#6281=EDGE_LOOP('',(#35883,#35884,#35885,#35886));
#6282=EDGE_LOOP('',(#35887,#35888,#35889,#35890));
#6283=EDGE_LOOP('',(#35891,#35892,#35893,#35894));
#6284=EDGE_LOOP('',(#35895,#35896,#35897,#35898));
#6285=EDGE_LOOP('',(#35899,#35900,#35901,#35902));
#6286=EDGE_LOOP('',(#35903,#35904,#35905,#35906));
#6287=EDGE_LOOP('',(#35907,#35908,#35909,#35910));
#6288=EDGE_LOOP('',(#35911,#35912,#35913,#35914));
#6289=EDGE_LOOP('',(#35915,#35916,#35917,#35918));
#6290=EDGE_LOOP('',(#35919,#35920,#35921,#35922));
#6291=EDGE_LOOP('',(#35923,#35924,#35925,#35926));
#6292=EDGE_LOOP('',(#35927,#35928,#35929,#35930));
#6293=EDGE_LOOP('',(#35931,#35932,#35933,#35934));
#6294=EDGE_LOOP('',(#35935,#35936,#35937,#35938));
#6295=EDGE_LOOP('',(#35939,#35940,#35941,#35942));
#6296=EDGE_LOOP('',(#35943,#35944,#35945,#35946));
#6297=EDGE_LOOP('',(#35947,#35948,#35949,#35950));
#6298=EDGE_LOOP('',(#35951,#35952,#35953,#35954));
#6299=EDGE_LOOP('',(#35955,#35956,#35957,#35958));
#6300=EDGE_LOOP('',(#35959,#35960,#35961,#35962));
#6301=EDGE_LOOP('',(#35963,#35964,#35965,#35966));
#6302=EDGE_LOOP('',(#35967,#35968,#35969,#35970));
#6303=EDGE_LOOP('',(#35971,#35972,#35973,#35974));
#6304=EDGE_LOOP('',(#35975,#35976,#35977,#35978));
#6305=EDGE_LOOP('',(#35979,#35980,#35981,#35982));
#6306=EDGE_LOOP('',(#35983,#35984,#35985,#35986));
#6307=EDGE_LOOP('',(#35987,#35988,#35989,#35990));
#6308=EDGE_LOOP('',(#35991,#35992,#35993,#35994));
#6309=EDGE_LOOP('',(#35995,#35996,#35997,#35998));
#6310=EDGE_LOOP('',(#35999,#36000,#36001,#36002));
#6311=EDGE_LOOP('',(#36003,#36004,#36005,#36006));
#6312=EDGE_LOOP('',(#36007,#36008,#36009,#36010));
#6313=EDGE_LOOP('',(#36011,#36012,#36013,#36014));
#6314=EDGE_LOOP('',(#36015,#36016,#36017,#36018));
#6315=EDGE_LOOP('',(#36019,#36020,#36021,#36022));
#6316=EDGE_LOOP('',(#36023,#36024,#36025,#36026));
#6317=EDGE_LOOP('',(#36027,#36028,#36029,#36030));
#6318=EDGE_LOOP('',(#36031,#36032,#36033,#36034));
#6319=EDGE_LOOP('',(#36035,#36036,#36037,#36038));
#6320=EDGE_LOOP('',(#36039,#36040,#36041,#36042));
#6321=EDGE_LOOP('',(#36043,#36044,#36045,#36046));
#6322=EDGE_LOOP('',(#36047,#36048,#36049,#36050));
#6323=EDGE_LOOP('',(#36051,#36052,#36053,#36054));
#6324=EDGE_LOOP('',(#36055,#36056,#36057,#36058));
#6325=EDGE_LOOP('',(#36059,#36060,#36061,#36062));
#6326=EDGE_LOOP('',(#36063,#36064,#36065,#36066));
#6327=EDGE_LOOP('',(#36067,#36068,#36069,#36070));
#6328=EDGE_LOOP('',(#36071,#36072,#36073,#36074));
#6329=EDGE_LOOP('',(#36075,#36076,#36077,#36078));
#6330=EDGE_LOOP('',(#36079,#36080,#36081,#36082));
#6331=EDGE_LOOP('',(#36083,#36084,#36085,#36086));
#6332=EDGE_LOOP('',(#36087,#36088,#36089,#36090));
#6333=EDGE_LOOP('',(#36091,#36092,#36093,#36094));
#6334=EDGE_LOOP('',(#36095,#36096,#36097,#36098));
#6335=EDGE_LOOP('',(#36099,#36100,#36101,#36102));
#6336=EDGE_LOOP('',(#36103,#36104,#36105,#36106));
#6337=EDGE_LOOP('',(#36107,#36108,#36109,#36110));
#6338=EDGE_LOOP('',(#36111,#36112,#36113,#36114));
#6339=EDGE_LOOP('',(#36115,#36116,#36117,#36118));
#6340=EDGE_LOOP('',(#36119,#36120,#36121,#36122));
#6341=EDGE_LOOP('',(#36123,#36124,#36125,#36126));
#6342=EDGE_LOOP('',(#36127,#36128,#36129,#36130));
#6343=EDGE_LOOP('',(#36131,#36132,#36133,#36134));
#6344=EDGE_LOOP('',(#36135,#36136,#36137,#36138));
#6345=EDGE_LOOP('',(#36139,#36140,#36141,#36142));
#6346=EDGE_LOOP('',(#36143,#36144,#36145,#36146));
#6347=EDGE_LOOP('',(#36147,#36148,#36149,#36150));
#6348=EDGE_LOOP('',(#36151,#36152,#36153,#36154));
#6349=EDGE_LOOP('',(#36155,#36156,#36157,#36158));
#6350=EDGE_LOOP('',(#36159,#36160,#36161,#36162));
#6351=EDGE_LOOP('',(#36163,#36164,#36165,#36166));
#6352=EDGE_LOOP('',(#36167,#36168,#36169,#36170));
#6353=EDGE_LOOP('',(#36171,#36172,#36173,#36174));
#6354=EDGE_LOOP('',(#36175,#36176,#36177,#36178));
#6355=EDGE_LOOP('',(#36179,#36180,#36181,#36182));
#6356=EDGE_LOOP('',(#36183,#36184,#36185,#36186));
#6357=EDGE_LOOP('',(#36187,#36188,#36189,#36190));
#6358=EDGE_LOOP('',(#36191,#36192,#36193,#36194));
#6359=EDGE_LOOP('',(#36195,#36196,#36197,#36198));
#6360=EDGE_LOOP('',(#36199,#36200,#36201,#36202));
#6361=EDGE_LOOP('',(#36203,#36204,#36205,#36206));
#6362=EDGE_LOOP('',(#36207,#36208,#36209,#36210));
#6363=EDGE_LOOP('',(#36211,#36212,#36213,#36214));
#6364=EDGE_LOOP('',(#36215,#36216,#36217,#36218));
#6365=EDGE_LOOP('',(#36219,#36220,#36221,#36222));
#6366=EDGE_LOOP('',(#36223,#36224,#36225,#36226));
#6367=EDGE_LOOP('',(#36227,#36228,#36229,#36230));
#6368=EDGE_LOOP('',(#36231,#36232,#36233,#36234));
#6369=EDGE_LOOP('',(#36235,#36236,#36237,#36238));
#6370=EDGE_LOOP('',(#36239,#36240,#36241,#36242));
#6371=EDGE_LOOP('',(#36243,#36244,#36245,#36246));
#6372=EDGE_LOOP('',(#36247,#36248,#36249,#36250));
#6373=EDGE_LOOP('',(#36251,#36252,#36253,#36254));
#6374=EDGE_LOOP('',(#36255,#36256,#36257,#36258));
#6375=EDGE_LOOP('',(#36259,#36260,#36261,#36262));
#6376=EDGE_LOOP('',(#36263,#36264,#36265,#36266));
#6377=EDGE_LOOP('',(#36267,#36268,#36269,#36270));
#6378=EDGE_LOOP('',(#36271,#36272,#36273,#36274));
#6379=EDGE_LOOP('',(#36275,#36276,#36277,#36278));
#6380=EDGE_LOOP('',(#36279,#36280,#36281,#36282));
#6381=EDGE_LOOP('',(#36283,#36284,#36285,#36286));
#6382=EDGE_LOOP('',(#36287,#36288,#36289,#36290));
#6383=EDGE_LOOP('',(#36291,#36292,#36293,#36294));
#6384=EDGE_LOOP('',(#36295,#36296,#36297,#36298));
#6385=EDGE_LOOP('',(#36299,#36300,#36301,#36302));
#6386=EDGE_LOOP('',(#36303,#36304,#36305,#36306));
#6387=EDGE_LOOP('',(#36307,#36308,#36309,#36310));
#6388=EDGE_LOOP('',(#36311,#36312,#36313,#36314));
#6389=EDGE_LOOP('',(#36315,#36316,#36317,#36318));
#6390=EDGE_LOOP('',(#36319,#36320,#36321,#36322));
#6391=EDGE_LOOP('',(#36323,#36324,#36325,#36326));
#6392=EDGE_LOOP('',(#36327,#36328,#36329,#36330));
#6393=EDGE_LOOP('',(#36331,#36332,#36333,#36334));
#6394=EDGE_LOOP('',(#36335,#36336,#36337,#36338));
#6395=EDGE_LOOP('',(#36339,#36340,#36341,#36342));
#6396=EDGE_LOOP('',(#36343,#36344,#36345,#36346));
#6397=EDGE_LOOP('',(#36347,#36348,#36349,#36350));
#6398=EDGE_LOOP('',(#36351,#36352,#36353,#36354));
#6399=EDGE_LOOP('',(#36355,#36356,#36357,#36358));
#6400=EDGE_LOOP('',(#36359,#36360,#36361,#36362));
#6401=EDGE_LOOP('',(#36363,#36364,#36365,#36366));
#6402=EDGE_LOOP('',(#36367,#36368,#36369,#36370));
#6403=EDGE_LOOP('',(#36371,#36372,#36373,#36374));
#6404=EDGE_LOOP('',(#36375,#36376,#36377,#36378));
#6405=EDGE_LOOP('',(#36379,#36380,#36381,#36382));
#6406=EDGE_LOOP('',(#36383,#36384,#36385,#36386));
#6407=EDGE_LOOP('',(#36387,#36388,#36389,#36390));
#6408=EDGE_LOOP('',(#36391,#36392,#36393,#36394));
#6409=EDGE_LOOP('',(#36395,#36396,#36397,#36398));
#6410=EDGE_LOOP('',(#36399,#36400,#36401,#36402));
#6411=EDGE_LOOP('',(#36403,#36404,#36405,#36406));
#6412=EDGE_LOOP('',(#36407,#36408,#36409,#36410));
#6413=EDGE_LOOP('',(#36411,#36412,#36413,#36414));
#6414=EDGE_LOOP('',(#36415,#36416,#36417,#36418));
#6415=EDGE_LOOP('',(#36419,#36420,#36421,#36422));
#6416=EDGE_LOOP('',(#36423,#36424,#36425,#36426));
#6417=EDGE_LOOP('',(#36427,#36428,#36429,#36430));
#6418=EDGE_LOOP('',(#36431,#36432,#36433,#36434));
#6419=EDGE_LOOP('',(#36435,#36436,#36437,#36438));
#6420=EDGE_LOOP('',(#36439,#36440,#36441,#36442));
#6421=EDGE_LOOP('',(#36443,#36444,#36445,#36446));
#6422=EDGE_LOOP('',(#36447,#36448,#36449,#36450));
#6423=EDGE_LOOP('',(#36451,#36452,#36453,#36454));
#6424=EDGE_LOOP('',(#36455,#36456,#36457,#36458));
#6425=EDGE_LOOP('',(#36459,#36460,#36461,#36462));
#6426=EDGE_LOOP('',(#36463,#36464,#36465,#36466));
#6427=EDGE_LOOP('',(#36467,#36468,#36469,#36470));
#6428=EDGE_LOOP('',(#36471,#36472,#36473,#36474));
#6429=EDGE_LOOP('',(#36475,#36476,#36477,#36478));
#6430=EDGE_LOOP('',(#36479,#36480,#36481,#36482));
#6431=EDGE_LOOP('',(#36483,#36484,#36485,#36486));
#6432=EDGE_LOOP('',(#36487,#36488,#36489,#36490));
#6433=EDGE_LOOP('',(#36491,#36492,#36493,#36494));
#6434=EDGE_LOOP('',(#36495,#36496,#36497,#36498));
#6435=EDGE_LOOP('',(#36499,#36500,#36501,#36502));
#6436=EDGE_LOOP('',(#36503,#36504,#36505,#36506));
#6437=EDGE_LOOP('',(#36507,#36508,#36509,#36510));
#6438=EDGE_LOOP('',(#36511,#36512,#36513,#36514));
#6439=EDGE_LOOP('',(#36515,#36516,#36517,#36518));
#6440=EDGE_LOOP('',(#36519,#36520,#36521,#36522));
#6441=EDGE_LOOP('',(#36523,#36524,#36525,#36526));
#6442=EDGE_LOOP('',(#36527,#36528,#36529,#36530));
#6443=EDGE_LOOP('',(#36531,#36532,#36533,#36534));
#6444=EDGE_LOOP('',(#36535,#36536,#36537,#36538));
#6445=EDGE_LOOP('',(#36539,#36540,#36541,#36542));
#6446=EDGE_LOOP('',(#36543,#36544,#36545,#36546));
#6447=EDGE_LOOP('',(#36547,#36548,#36549,#36550));
#6448=EDGE_LOOP('',(#36551,#36552,#36553,#36554));
#6449=EDGE_LOOP('',(#36555,#36556,#36557,#36558));
#6450=EDGE_LOOP('',(#36559,#36560,#36561,#36562));
#6451=EDGE_LOOP('',(#36563,#36564,#36565,#36566));
#6452=EDGE_LOOP('',(#36567,#36568,#36569,#36570));
#6453=EDGE_LOOP('',(#36571,#36572,#36573,#36574));
#6454=EDGE_LOOP('',(#36575,#36576,#36577,#36578));
#6455=EDGE_LOOP('',(#36579,#36580,#36581,#36582));
#6456=EDGE_LOOP('',(#36583,#36584,#36585,#36586));
#6457=EDGE_LOOP('',(#36587,#36588,#36589,#36590));
#6458=EDGE_LOOP('',(#36591,#36592,#36593,#36594));
#6459=EDGE_LOOP('',(#36595,#36596,#36597,#36598));
#6460=EDGE_LOOP('',(#36599,#36600,#36601,#36602));
#6461=EDGE_LOOP('',(#36603,#36604,#36605,#36606));
#6462=EDGE_LOOP('',(#36607,#36608,#36609,#36610));
#6463=EDGE_LOOP('',(#36611,#36612,#36613,#36614));
#6464=EDGE_LOOP('',(#36615,#36616,#36617,#36618));
#6465=EDGE_LOOP('',(#36619,#36620,#36621,#36622));
#6466=EDGE_LOOP('',(#36623,#36624,#36625,#36626));
#6467=EDGE_LOOP('',(#36627,#36628,#36629,#36630));
#6468=EDGE_LOOP('',(#36631,#36632,#36633,#36634));
#6469=EDGE_LOOP('',(#36635,#36636,#36637,#36638));
#6470=EDGE_LOOP('',(#36639,#36640,#36641,#36642));
#6471=EDGE_LOOP('',(#36643,#36644,#36645,#36646));
#6472=EDGE_LOOP('',(#36647,#36648,#36649,#36650));
#6473=EDGE_LOOP('',(#36651,#36652,#36653,#36654));
#6474=EDGE_LOOP('',(#36655,#36656,#36657,#36658));
#6475=EDGE_LOOP('',(#36659,#36660,#36661,#36662));
#6476=EDGE_LOOP('',(#36663,#36664,#36665,#36666));
#6477=EDGE_LOOP('',(#36667,#36668,#36669,#36670));
#6478=EDGE_LOOP('',(#36671,#36672,#36673,#36674));
#6479=EDGE_LOOP('',(#36675,#36676,#36677,#36678));
#6480=EDGE_LOOP('',(#36679,#36680,#36681,#36682));
#6481=EDGE_LOOP('',(#36683,#36684,#36685,#36686));
#6482=EDGE_LOOP('',(#36687,#36688,#36689,#36690));
#6483=EDGE_LOOP('',(#36691,#36692,#36693,#36694));
#6484=EDGE_LOOP('',(#36695,#36696,#36697,#36698));
#6485=EDGE_LOOP('',(#36699,#36700,#36701,#36702));
#6486=EDGE_LOOP('',(#36703,#36704,#36705,#36706));
#6487=EDGE_LOOP('',(#36707,#36708,#36709,#36710));
#6488=EDGE_LOOP('',(#36711,#36712,#36713,#36714));
#6489=EDGE_LOOP('',(#36715,#36716,#36717,#36718));
#6490=EDGE_LOOP('',(#36719,#36720,#36721,#36722));
#6491=EDGE_LOOP('',(#36723,#36724,#36725,#36726));
#6492=EDGE_LOOP('',(#36727,#36728,#36729,#36730));
#6493=EDGE_LOOP('',(#36731,#36732,#36733,#36734));
#6494=EDGE_LOOP('',(#36735,#36736,#36737,#36738));
#6495=EDGE_LOOP('',(#36739,#36740,#36741,#36742));
#6496=EDGE_LOOP('',(#36743,#36744,#36745,#36746));
#6497=EDGE_LOOP('',(#36747,#36748,#36749,#36750));
#6498=EDGE_LOOP('',(#36751,#36752,#36753,#36754));
#6499=EDGE_LOOP('',(#36755,#36756,#36757,#36758));
#6500=EDGE_LOOP('',(#36759,#36760,#36761,#36762));
#6501=EDGE_LOOP('',(#36763,#36764,#36765,#36766));
#6502=EDGE_LOOP('',(#36767,#36768,#36769,#36770));
#6503=EDGE_LOOP('',(#36771,#36772,#36773,#36774));
#6504=EDGE_LOOP('',(#36775,#36776,#36777,#36778));
#6505=EDGE_LOOP('',(#36779,#36780,#36781,#36782));
#6506=EDGE_LOOP('',(#36783,#36784,#36785,#36786));
#6507=EDGE_LOOP('',(#36787,#36788,#36789,#36790));
#6508=EDGE_LOOP('',(#36791,#36792,#36793,#36794));
#6509=EDGE_LOOP('',(#36795,#36796,#36797,#36798));
#6510=EDGE_LOOP('',(#36799,#36800,#36801,#36802));
#6511=EDGE_LOOP('',(#36803,#36804,#36805,#36806));
#6512=EDGE_LOOP('',(#36807,#36808,#36809,#36810));
#6513=EDGE_LOOP('',(#36811,#36812,#36813,#36814));
#6514=EDGE_LOOP('',(#36815,#36816,#36817,#36818));
#6515=EDGE_LOOP('',(#36819,#36820,#36821,#36822));
#6516=EDGE_LOOP('',(#36823,#36824,#36825,#36826));
#6517=EDGE_LOOP('',(#36827,#36828,#36829,#36830));
#6518=EDGE_LOOP('',(#36831,#36832,#36833,#36834));
#6519=EDGE_LOOP('',(#36835,#36836,#36837,#36838));
#6520=EDGE_LOOP('',(#36839,#36840,#36841,#36842));
#6521=EDGE_LOOP('',(#36843,#36844,#36845,#36846));
#6522=EDGE_LOOP('',(#36847,#36848,#36849,#36850));
#6523=EDGE_LOOP('',(#36851,#36852,#36853,#36854));
#6524=EDGE_LOOP('',(#36855,#36856,#36857,#36858));
#6525=EDGE_LOOP('',(#36859,#36860,#36861,#36862));
#6526=EDGE_LOOP('',(#36863,#36864,#36865,#36866));
#6527=EDGE_LOOP('',(#36867,#36868,#36869,#36870));
#6528=EDGE_LOOP('',(#36871,#36872,#36873,#36874));
#6529=EDGE_LOOP('',(#36875,#36876,#36877,#36878));
#6530=EDGE_LOOP('',(#36879,#36880,#36881,#36882));
#6531=EDGE_LOOP('',(#36883,#36884,#36885,#36886));
#6532=EDGE_LOOP('',(#36887,#36888,#36889,#36890));
#6533=EDGE_LOOP('',(#36891,#36892,#36893,#36894));
#6534=EDGE_LOOP('',(#36895,#36896,#36897,#36898));
#6535=EDGE_LOOP('',(#36899,#36900,#36901,#36902));
#6536=EDGE_LOOP('',(#36903,#36904,#36905,#36906));
#6537=EDGE_LOOP('',(#36907,#36908,#36909,#36910));
#6538=EDGE_LOOP('',(#36911,#36912,#36913,#36914));
#6539=EDGE_LOOP('',(#36915,#36916,#36917,#36918));
#6540=EDGE_LOOP('',(#36919,#36920,#36921,#36922));
#6541=EDGE_LOOP('',(#36923,#36924,#36925,#36926));
#6542=EDGE_LOOP('',(#36927,#36928,#36929,#36930));
#6543=EDGE_LOOP('',(#36931,#36932,#36933,#36934));
#6544=EDGE_LOOP('',(#36935,#36936,#36937,#36938));
#6545=EDGE_LOOP('',(#36939,#36940,#36941,#36942));
#6546=EDGE_LOOP('',(#36943,#36944,#36945,#36946));
#6547=EDGE_LOOP('',(#36947,#36948,#36949,#36950));
#6548=EDGE_LOOP('',(#36951,#36952,#36953,#36954));
#6549=EDGE_LOOP('',(#36955,#36956,#36957,#36958));
#6550=EDGE_LOOP('',(#36959,#36960,#36961,#36962));
#6551=EDGE_LOOP('',(#36963,#36964,#36965,#36966));
#6552=EDGE_LOOP('',(#36967,#36968,#36969,#36970));
#6553=EDGE_LOOP('',(#36971,#36972,#36973,#36974));
#6554=EDGE_LOOP('',(#36975,#36976,#36977,#36978));
#6555=EDGE_LOOP('',(#36979,#36980,#36981,#36982));
#6556=EDGE_LOOP('',(#36983,#36984,#36985,#36986));
#6557=EDGE_LOOP('',(#36987,#36988,#36989,#36990));
#6558=EDGE_LOOP('',(#36991,#36992,#36993,#36994));
#6559=EDGE_LOOP('',(#36995,#36996,#36997,#36998));
#6560=EDGE_LOOP('',(#36999,#37000,#37001,#37002));
#6561=EDGE_LOOP('',(#37003,#37004,#37005,#37006));
#6562=EDGE_LOOP('',(#37007,#37008,#37009,#37010));
#6563=EDGE_LOOP('',(#37011,#37012,#37013,#37014));
#6564=EDGE_LOOP('',(#37015,#37016,#37017,#37018));
#6565=EDGE_LOOP('',(#37019,#37020,#37021,#37022));
#6566=EDGE_LOOP('',(#37023,#37024,#37025,#37026));
#6567=EDGE_LOOP('',(#37027,#37028,#37029,#37030));
#6568=EDGE_LOOP('',(#37031,#37032,#37033,#37034));
#6569=EDGE_LOOP('',(#37035,#37036,#37037,#37038));
#6570=EDGE_LOOP('',(#37039,#37040,#37041,#37042));
#6571=EDGE_LOOP('',(#37043,#37044,#37045,#37046));
#6572=EDGE_LOOP('',(#37047,#37048,#37049,#37050));
#6573=EDGE_LOOP('',(#37051,#37052,#37053,#37054));
#6574=EDGE_LOOP('',(#37055,#37056,#37057,#37058));
#6575=EDGE_LOOP('',(#37059,#37060,#37061,#37062));
#6576=EDGE_LOOP('',(#37063,#37064,#37065,#37066));
#6577=EDGE_LOOP('',(#37067,#37068,#37069,#37070));
#6578=EDGE_LOOP('',(#37071,#37072,#37073,#37074));
#6579=EDGE_LOOP('',(#37075,#37076,#37077,#37078));
#6580=EDGE_LOOP('',(#37079,#37080,#37081,#37082));
#6581=EDGE_LOOP('',(#37083,#37084,#37085,#37086));
#6582=EDGE_LOOP('',(#37087,#37088,#37089,#37090));
#6583=EDGE_LOOP('',(#37091,#37092,#37093,#37094));
#6584=EDGE_LOOP('',(#37095,#37096,#37097,#37098));
#6585=EDGE_LOOP('',(#37099,#37100,#37101,#37102));
#6586=EDGE_LOOP('',(#37103,#37104,#37105,#37106));
#6587=EDGE_LOOP('',(#37107,#37108,#37109,#37110));
#6588=EDGE_LOOP('',(#37111,#37112,#37113,#37114));
#6589=EDGE_LOOP('',(#37115,#37116,#37117,#37118));
#6590=EDGE_LOOP('',(#37119,#37120,#37121,#37122));
#6591=EDGE_LOOP('',(#37123,#37124,#37125,#37126));
#6592=EDGE_LOOP('',(#37127,#37128,#37129,#37130));
#6593=EDGE_LOOP('',(#37131,#37132,#37133,#37134));
#6594=EDGE_LOOP('',(#37135,#37136,#37137,#37138));
#6595=EDGE_LOOP('',(#37139,#37140,#37141,#37142));
#6596=EDGE_LOOP('',(#37143,#37144,#37145,#37146));
#6597=EDGE_LOOP('',(#37147,#37148,#37149,#37150));
#6598=EDGE_LOOP('',(#37151,#37152,#37153,#37154));
#6599=EDGE_LOOP('',(#37155,#37156,#37157,#37158));
#6600=EDGE_LOOP('',(#37159,#37160,#37161,#37162));
#6601=EDGE_LOOP('',(#37163,#37164,#37165,#37166));
#6602=EDGE_LOOP('',(#37167,#37168,#37169,#37170));
#6603=EDGE_LOOP('',(#37171,#37172,#37173,#37174));
#6604=EDGE_LOOP('',(#37175,#37176,#37177,#37178));
#6605=EDGE_LOOP('',(#37179,#37180,#37181,#37182));
#6606=EDGE_LOOP('',(#37183,#37184,#37185,#37186));
#6607=EDGE_LOOP('',(#37187,#37188,#37189,#37190));
#6608=EDGE_LOOP('',(#37191,#37192,#37193,#37194));
#6609=EDGE_LOOP('',(#37195,#37196,#37197,#37198));
#6610=EDGE_LOOP('',(#37199,#37200,#37201,#37202));
#6611=EDGE_LOOP('',(#37203,#37204,#37205,#37206));
#6612=EDGE_LOOP('',(#37207,#37208,#37209,#37210));
#6613=EDGE_LOOP('',(#37211,#37212,#37213,#37214));
#6614=EDGE_LOOP('',(#37215,#37216,#37217,#37218));
#6615=EDGE_LOOP('',(#37219,#37220,#37221,#37222));
#6616=EDGE_LOOP('',(#37223,#37224,#37225,#37226));
#6617=EDGE_LOOP('',(#37227,#37228,#37229,#37230));
#6618=EDGE_LOOP('',(#37231,#37232,#37233,#37234));
#6619=EDGE_LOOP('',(#37235,#37236,#37237,#37238));
#6620=EDGE_LOOP('',(#37239,#37240,#37241,#37242));
#6621=EDGE_LOOP('',(#37243,#37244,#37245,#37246));
#6622=EDGE_LOOP('',(#37247,#37248,#37249,#37250));
#6623=EDGE_LOOP('',(#37251,#37252,#37253,#37254));
#6624=EDGE_LOOP('',(#37255,#37256,#37257,#37258));
#6625=EDGE_LOOP('',(#37259,#37260,#37261,#37262));
#6626=EDGE_LOOP('',(#37263,#37264,#37265,#37266));
#6627=EDGE_LOOP('',(#37267,#37268,#37269,#37270));
#6628=EDGE_LOOP('',(#37271,#37272,#37273,#37274));
#6629=EDGE_LOOP('',(#37275,#37276,#37277,#37278));
#6630=EDGE_LOOP('',(#37279,#37280,#37281,#37282));
#6631=EDGE_LOOP('',(#37283,#37284,#37285,#37286));
#6632=EDGE_LOOP('',(#37287,#37288,#37289,#37290));
#6633=EDGE_LOOP('',(#37291,#37292,#37293,#37294));
#6634=EDGE_LOOP('',(#37295,#37296,#37297,#37298));
#6635=EDGE_LOOP('',(#37299,#37300,#37301,#37302));
#6636=EDGE_LOOP('',(#37303,#37304,#37305,#37306));
#6637=EDGE_LOOP('',(#37307,#37308,#37309,#37310));
#6638=EDGE_LOOP('',(#37311,#37312,#37313,#37314));
#6639=EDGE_LOOP('',(#37315,#37316,#37317,#37318));
#6640=EDGE_LOOP('',(#37319,#37320,#37321,#37322));
#6641=EDGE_LOOP('',(#37323,#37324,#37325,#37326));
#6642=EDGE_LOOP('',(#37327,#37328,#37329,#37330));
#6643=EDGE_LOOP('',(#37331,#37332,#37333,#37334));
#6644=EDGE_LOOP('',(#37335,#37336,#37337,#37338));
#6645=EDGE_LOOP('',(#37339,#37340,#37341,#37342));
#6646=EDGE_LOOP('',(#37343,#37344,#37345,#37346));
#6647=EDGE_LOOP('',(#37347,#37348,#37349,#37350));
#6648=EDGE_LOOP('',(#37351,#37352,#37353,#37354));
#6649=EDGE_LOOP('',(#37355,#37356,#37357,#37358));
#6650=EDGE_LOOP('',(#37359,#37360,#37361,#37362));
#6651=EDGE_LOOP('',(#37363,#37364,#37365,#37366));
#6652=EDGE_LOOP('',(#37367,#37368,#37369,#37370));
#6653=EDGE_LOOP('',(#37371,#37372,#37373,#37374));
#6654=EDGE_LOOP('',(#37375,#37376,#37377,#37378));
#6655=EDGE_LOOP('',(#37379,#37380,#37381,#37382));
#6656=EDGE_LOOP('',(#37383,#37384,#37385,#37386));
#6657=EDGE_LOOP('',(#37387,#37388,#37389,#37390));
#6658=EDGE_LOOP('',(#37391,#37392,#37393,#37394));
#6659=EDGE_LOOP('',(#37395,#37396,#37397,#37398));
#6660=EDGE_LOOP('',(#37399,#37400,#37401,#37402));
#6661=EDGE_LOOP('',(#37403,#37404,#37405,#37406));
#6662=EDGE_LOOP('',(#37407,#37408,#37409,#37410));
#6663=EDGE_LOOP('',(#37411,#37412,#37413,#37414));
#6664=EDGE_LOOP('',(#37415,#37416,#37417,#37418));
#6665=EDGE_LOOP('',(#37419,#37420,#37421,#37422));
#6666=EDGE_LOOP('',(#37423,#37424,#37425,#37426));
#6667=EDGE_LOOP('',(#37427,#37428,#37429,#37430));
#6668=EDGE_LOOP('',(#37431,#37432,#37433,#37434));
#6669=EDGE_LOOP('',(#37435,#37436,#37437,#37438));
#6670=EDGE_LOOP('',(#37439,#37440,#37441,#37442));
#6671=EDGE_LOOP('',(#37443,#37444,#37445,#37446));
#6672=EDGE_LOOP('',(#37447,#37448,#37449,#37450));
#6673=EDGE_LOOP('',(#37451,#37452,#37453,#37454));
#6674=EDGE_LOOP('',(#37455,#37456,#37457,#37458));
#6675=EDGE_LOOP('',(#37459,#37460,#37461,#37462));
#6676=EDGE_LOOP('',(#37463,#37464,#37465,#37466));
#6677=EDGE_LOOP('',(#37467,#37468,#37469,#37470));
#6678=EDGE_LOOP('',(#37471,#37472,#37473,#37474));
#6679=EDGE_LOOP('',(#37475,#37476,#37477,#37478));
#6680=EDGE_LOOP('',(#37479,#37480,#37481,#37482));
#6681=EDGE_LOOP('',(#37483,#37484,#37485,#37486));
#6682=EDGE_LOOP('',(#37487,#37488,#37489,#37490));
#6683=EDGE_LOOP('',(#37491,#37492,#37493,#37494));
#6684=EDGE_LOOP('',(#37495,#37496,#37497,#37498));
#6685=EDGE_LOOP('',(#37499,#37500,#37501,#37502));
#6686=EDGE_LOOP('',(#37503,#37504,#37505,#37506));
#6687=EDGE_LOOP('',(#37507,#37508,#37509,#37510));
#6688=EDGE_LOOP('',(#37511,#37512,#37513,#37514));
#6689=EDGE_LOOP('',(#37515,#37516,#37517,#37518));
#6690=EDGE_LOOP('',(#37519,#37520,#37521,#37522));
#6691=EDGE_LOOP('',(#37523,#37524,#37525,#37526));
#6692=EDGE_LOOP('',(#37527,#37528,#37529,#37530));
#6693=EDGE_LOOP('',(#37531,#37532,#37533,#37534));
#6694=EDGE_LOOP('',(#37535,#37536,#37537,#37538));
#6695=EDGE_LOOP('',(#37539,#37540,#37541,#37542));
#6696=EDGE_LOOP('',(#37543,#37544,#37545,#37546));
#6697=EDGE_LOOP('',(#37547,#37548,#37549,#37550));
#6698=EDGE_LOOP('',(#37551,#37552,#37553,#37554));
#6699=EDGE_LOOP('',(#37555,#37556,#37557,#37558));
#6700=EDGE_LOOP('',(#37559,#37560,#37561,#37562));
#6701=EDGE_LOOP('',(#37563,#37564,#37565,#37566));
#6702=EDGE_LOOP('',(#37567,#37568,#37569,#37570));
#6703=EDGE_LOOP('',(#37571,#37572,#37573,#37574));
#6704=EDGE_LOOP('',(#37575,#37576,#37577,#37578));
#6705=EDGE_LOOP('',(#37579,#37580,#37581,#37582));
#6706=EDGE_LOOP('',(#37583,#37584,#37585,#37586));
#6707=EDGE_LOOP('',(#37587,#37588,#37589,#37590));
#6708=EDGE_LOOP('',(#37591,#37592,#37593,#37594));
#6709=EDGE_LOOP('',(#37595,#37596,#37597,#37598));
#6710=EDGE_LOOP('',(#37599,#37600,#37601,#37602));
#6711=EDGE_LOOP('',(#37603,#37604,#37605,#37606));
#6712=EDGE_LOOP('',(#37607,#37608,#37609,#37610));
#6713=EDGE_LOOP('',(#37611,#37612,#37613,#37614));
#6714=EDGE_LOOP('',(#37615,#37616,#37617,#37618));
#6715=EDGE_LOOP('',(#37619,#37620,#37621,#37622));
#6716=EDGE_LOOP('',(#37623,#37624,#37625,#37626));
#6717=EDGE_LOOP('',(#37627,#37628,#37629,#37630));
#6718=EDGE_LOOP('',(#37631,#37632,#37633,#37634));
#6719=EDGE_LOOP('',(#37635,#37636,#37637,#37638));
#6720=EDGE_LOOP('',(#37639,#37640,#37641,#37642));
#6721=EDGE_LOOP('',(#37643,#37644,#37645,#37646));
#6722=EDGE_LOOP('',(#37647,#37648,#37649,#37650));
#6723=EDGE_LOOP('',(#37651,#37652,#37653,#37654));
#6724=EDGE_LOOP('',(#37655,#37656,#37657,#37658));
#6725=EDGE_LOOP('',(#37659,#37660,#37661,#37662));
#6726=EDGE_LOOP('',(#37663,#37664,#37665,#37666));
#6727=EDGE_LOOP('',(#37667,#37668,#37669,#37670));
#6728=EDGE_LOOP('',(#37671,#37672,#37673,#37674));
#6729=EDGE_LOOP('',(#37675,#37676,#37677,#37678));
#6730=EDGE_LOOP('',(#37679,#37680,#37681,#37682));
#6731=EDGE_LOOP('',(#37683,#37684,#37685,#37686));
#6732=EDGE_LOOP('',(#37687,#37688,#37689,#37690));
#6733=EDGE_LOOP('',(#37691,#37692,#37693,#37694));
#6734=EDGE_LOOP('',(#37695,#37696,#37697,#37698));
#6735=EDGE_LOOP('',(#37699,#37700,#37701,#37702));
#6736=EDGE_LOOP('',(#37703,#37704,#37705,#37706));
#6737=EDGE_LOOP('',(#37707,#37708,#37709,#37710));
#6738=EDGE_LOOP('',(#37711,#37712,#37713,#37714));
#6739=EDGE_LOOP('',(#37715,#37716,#37717,#37718));
#6740=LINE('',#52457,#11615);
#6741=LINE('',#52463,#11616);
#6742=LINE('',#52469,#11617);
#6743=LINE('',#52475,#11618);
#6744=LINE('',#52481,#11619);
#6745=LINE('',#52487,#11620);
#6746=LINE('',#52494,#11621);
#6747=LINE('',#52497,#11622);
#6748=LINE('',#52503,#11623);
#6749=LINE('',#52506,#11624);
#6750=LINE('',#52512,#11625);
#6751=LINE('',#52515,#11626);
#6752=LINE('',#52521,#11627);
#6753=LINE('',#52524,#11628);
#6754=LINE('',#52530,#11629);
#6755=LINE('',#52533,#11630);
#6756=LINE('',#52539,#11631);
#6757=LINE('',#52542,#11632);
#6758=LINE('',#52548,#11633);
#6759=LINE('',#52551,#11634);
#6760=LINE('',#52557,#11635);
#6761=LINE('',#52560,#11636);
#6762=LINE('',#52566,#11637);
#6763=LINE('',#52569,#11638);
#6764=LINE('',#52575,#11639);
#6765=LINE('',#52578,#11640);
#6766=LINE('',#52584,#11641);
#6767=LINE('',#52587,#11642);
#6768=LINE('',#52593,#11643);
#6769=LINE('',#52596,#11644);
#6770=LINE('',#52602,#11645);
#6771=LINE('',#52605,#11646);
#6772=LINE('',#52611,#11647);
#6773=LINE('',#52614,#11648);
#6774=LINE('',#52620,#11649);
#6775=LINE('',#52623,#11650);
#6776=LINE('',#52629,#11651);
#6777=LINE('',#52632,#11652);
#6778=LINE('',#52638,#11653);
#6779=LINE('',#52641,#11654);
#6780=LINE('',#52647,#11655);
#6781=LINE('',#52650,#11656);
#6782=LINE('',#52656,#11657);
#6783=LINE('',#52659,#11658);
#6784=LINE('',#52665,#11659);
#6785=LINE('',#52668,#11660);
#6786=LINE('',#52674,#11661);
#6787=LINE('',#52677,#11662);
#6788=LINE('',#52683,#11663);
#6789=LINE('',#52686,#11664);
#6790=LINE('',#52692,#11665);
#6791=LINE('',#52695,#11666);
#6792=LINE('',#52701,#11667);
#6793=LINE('',#52704,#11668);
#6794=LINE('',#52710,#11669);
#6795=LINE('',#52713,#11670);
#6796=LINE('',#52719,#11671);
#6797=LINE('',#52722,#11672);
#6798=LINE('',#52728,#11673);
#6799=LINE('',#52731,#11674);
#6800=LINE('',#52737,#11675);
#6801=LINE('',#52740,#11676);
#6802=LINE('',#52746,#11677);
#6803=LINE('',#52749,#11678);
#6804=LINE('',#52755,#11679);
#6805=LINE('',#52758,#11680);
#6806=LINE('',#52764,#11681);
#6807=LINE('',#52767,#11682);
#6808=LINE('',#52773,#11683);
#6809=LINE('',#52776,#11684);
#6810=LINE('',#52782,#11685);
#6811=LINE('',#52785,#11686);
#6812=LINE('',#52791,#11687);
#6813=LINE('',#52794,#11688);
#6814=LINE('',#52800,#11689);
#6815=LINE('',#52803,#11690);
#6816=LINE('',#52809,#11691);
#6817=LINE('',#52812,#11692);
#6818=LINE('',#52818,#11693);
#6819=LINE('',#52821,#11694);
#6820=LINE('',#52827,#11695);
#6821=LINE('',#52830,#11696);
#6822=LINE('',#52836,#11697);
#6823=LINE('',#52839,#11698);
#6824=LINE('',#52845,#11699);
#6825=LINE('',#52848,#11700);
#6826=LINE('',#52854,#11701);
#6827=LINE('',#52857,#11702);
#6828=LINE('',#52863,#11703);
#6829=LINE('',#52866,#11704);
#6830=LINE('',#52872,#11705);
#6831=LINE('',#52875,#11706);
#6832=LINE('',#52881,#11707);
#6833=LINE('',#52884,#11708);
#6834=LINE('',#52890,#11709);
#6835=LINE('',#52893,#11710);
#6836=LINE('',#52899,#11711);
#6837=LINE('',#52902,#11712);
#6838=LINE('',#52908,#11713);
#6839=LINE('',#52911,#11714);
#6840=LINE('',#52917,#11715);
#6841=LINE('',#52920,#11716);
#6842=LINE('',#52926,#11717);
#6843=LINE('',#52929,#11718);
#6844=LINE('',#52935,#11719);
#6845=LINE('',#52938,#11720);
#6846=LINE('',#52944,#11721);
#6847=LINE('',#52947,#11722);
#6848=LINE('',#52953,#11723);
#6849=LINE('',#52956,#11724);
#6850=LINE('',#52962,#11725);
#6851=LINE('',#52965,#11726);
#6852=LINE('',#52971,#11727);
#6853=LINE('',#52974,#11728);
#6854=LINE('',#52980,#11729);
#6855=LINE('',#52983,#11730);
#6856=LINE('',#52989,#11731);
#6857=LINE('',#52992,#11732);
#6858=LINE('',#52998,#11733);
#6859=LINE('',#53001,#11734);
#6860=LINE('',#53007,#11735);
#6861=LINE('',#53010,#11736);
#6862=LINE('',#53016,#11737);
#6863=LINE('',#53019,#11738);
#6864=LINE('',#53025,#11739);
#6865=LINE('',#53028,#11740);
#6866=LINE('',#53034,#11741);
#6867=LINE('',#53037,#11742);
#6868=LINE('',#53043,#11743);
#6869=LINE('',#53046,#11744);
#6870=LINE('',#53052,#11745);
#6871=LINE('',#53055,#11746);
#6872=LINE('',#53061,#11747);
#6873=LINE('',#53064,#11748);
#6874=LINE('',#53070,#11749);
#6875=LINE('',#53073,#11750);
#6876=LINE('',#53079,#11751);
#6877=LINE('',#53082,#11752);
#6878=LINE('',#53103,#11753);
#6879=LINE('',#53112,#11754);
#6880=LINE('',#53131,#11755);
#6881=LINE('',#53138,#11756);
#6882=LINE('',#53157,#11757);
#6883=LINE('',#53164,#11758);
#6884=LINE('',#53186,#11759);
#6885=LINE('',#53194,#11760);
#6886=LINE('',#53216,#11761);
#6887=LINE('',#53224,#11762);
#6888=LINE('',#53229,#11763);
#6889=LINE('',#53235,#11764);
#6890=LINE('',#53241,#11765);
#6891=LINE('',#53247,#11766);
#6892=LINE('',#53273,#11767);
#6893=LINE('',#53279,#11768);
#6894=LINE('',#53285,#11769);
#6895=LINE('',#53291,#11770);
#6896=LINE('',#53320,#11771);
#6897=LINE('',#53330,#11772);
#6898=LINE('',#53334,#11773);
#6899=LINE('',#53336,#11774);
#6900=LINE('',#53338,#11775);
#6901=LINE('',#53342,#11776);
#6902=LINE('',#53346,#11777);
#6903=LINE('',#53348,#11778);
#6904=LINE('',#53350,#11779);
#6905=LINE('',#53352,#11780);
#6906=LINE('',#53354,#11781);
#6907=LINE('',#53356,#11782);
#6908=LINE('',#53358,#11783);
#6909=LINE('',#53360,#11784);
#6910=LINE('',#53362,#11785);
#6911=LINE('',#53364,#11786);
#6912=LINE('',#53366,#11787);
#6913=LINE('',#53370,#11788);
#6914=LINE('',#53374,#11789);
#6915=LINE('',#53376,#11790);
#6916=LINE('',#53378,#11791);
#6917=LINE('',#53380,#11792);
#6918=LINE('',#53382,#11793);
#6919=LINE('',#53384,#11794);
#6920=LINE('',#53386,#11795);
#6921=LINE('',#53387,#11796);
#6922=LINE('',#53390,#11797);
#6923=LINE('',#53392,#11798);
#6924=LINE('',#53394,#11799);
#6925=LINE('',#53396,#11800);
#6926=LINE('',#53398,#11801);
#6927=LINE('',#53400,#11802);
#6928=LINE('',#53402,#11803);
#6929=LINE('',#53403,#11804);
#6930=LINE('',#53406,#11805);
#6931=LINE('',#53408,#11806);
#6932=LINE('',#53410,#11807);
#6933=LINE('',#53412,#11808);
#6934=LINE('',#53414,#11809);
#6935=LINE('',#53416,#11810);
#6936=LINE('',#53418,#11811);
#6937=LINE('',#53419,#11812);
#6938=LINE('',#53422,#11813);
#6939=LINE('',#53424,#11814);
#6940=LINE('',#53426,#11815);
#6941=LINE('',#53428,#11816);
#6942=LINE('',#53430,#11817);
#6943=LINE('',#53432,#11818);
#6944=LINE('',#53434,#11819);
#6945=LINE('',#53435,#11820);
#6946=LINE('',#53438,#11821);
#6947=LINE('',#53440,#11822);
#6948=LINE('',#53442,#11823);
#6949=LINE('',#53444,#11824);
#6950=LINE('',#53446,#11825);
#6951=LINE('',#53448,#11826);
#6952=LINE('',#53450,#11827);
#6953=LINE('',#53451,#11828);
#6954=LINE('',#53455,#11829);
#6955=LINE('',#53457,#11830);
#6956=LINE('',#53459,#11831);
#6957=LINE('',#53461,#11832);
#6958=LINE('',#53463,#11833);
#6959=LINE('',#53465,#11834);
#6960=LINE('',#53467,#11835);
#6961=LINE('',#53469,#11836);
#6962=LINE('',#53471,#11837);
#6963=LINE('',#53473,#11838);
#6964=LINE('',#53477,#11839);
#6965=LINE('',#53481,#11840);
#6966=LINE('',#53483,#11841);
#6967=LINE('',#53485,#11842);
#6968=LINE('',#53487,#11843);
#6969=LINE('',#53489,#11844);
#6970=LINE('',#53491,#11845);
#6971=LINE('',#53493,#11846);
#6972=LINE('',#53495,#11847);
#6973=LINE('',#53497,#11848);
#6974=LINE('',#53499,#11849);
#6975=LINE('',#53501,#11850);
#6976=LINE('',#53505,#11851);
#6977=LINE('',#53508,#11852);
#6978=LINE('',#53511,#11853);
#6979=LINE('',#53513,#11854);
#6980=LINE('',#53515,#11855);
#6981=LINE('',#53516,#11856);
#6982=LINE('',#53519,#11857);
#6983=LINE('',#53521,#11858);
#6984=LINE('',#53523,#11859);
#6985=LINE('',#53524,#11860);
#6986=LINE('',#53527,#11861);
#6987=LINE('',#53529,#11862);
#6988=LINE('',#53531,#11863);
#6989=LINE('',#53532,#11864);
#6990=LINE('',#53535,#11865);
#6991=LINE('',#53537,#11866);
#6992=LINE('',#53539,#11867);
#6993=LINE('',#53540,#11868);
#6994=LINE('',#53542,#11869);
#6995=LINE('',#53543,#11870);
#6996=LINE('',#53545,#11871);
#6997=LINE('',#53546,#11872);
#6998=LINE('',#53550,#11873);
#6999=LINE('',#53552,#11874);
#7000=LINE('',#53554,#11875);
#7001=LINE('',#53558,#11876);
#7002=LINE('',#53562,#11877);
#7003=LINE('',#53564,#11878);
#7004=LINE('',#53566,#11879);
#7005=LINE('',#53568,#11880);
#7006=LINE('',#53570,#11881);
#7007=LINE('',#53572,#11882);
#7008=LINE('',#53574,#11883);
#7009=LINE('',#53575,#11884);
#7010=LINE('',#53578,#11885);
#7011=LINE('',#53580,#11886);
#7012=LINE('',#53582,#11887);
#7013=LINE('',#53584,#11888);
#7014=LINE('',#53586,#11889);
#7015=LINE('',#53588,#11890);
#7016=LINE('',#53590,#11891);
#7017=LINE('',#53591,#11892);
#7018=LINE('',#53595,#11893);
#7019=LINE('',#53597,#11894);
#7020=LINE('',#53601,#11895);
#7021=LINE('',#53604,#11896);
#7022=LINE('',#53607,#11897);
#7023=LINE('',#53609,#11898);
#7024=LINE('',#53611,#11899);
#7025=LINE('',#53612,#11900);
#7026=LINE('',#53615,#11901);
#7027=LINE('',#53617,#11902);
#7028=LINE('',#53619,#11903);
#7029=LINE('',#53620,#11904);
#7030=LINE('',#53622,#11905);
#7031=LINE('',#53623,#11906);
#7032=LINE('',#53625,#11907);
#7033=LINE('',#53626,#11908);
#7034=LINE('',#53630,#11909);
#7035=LINE('',#53632,#11910);
#7036=LINE('',#53634,#11911);
#7037=LINE('',#53636,#11912);
#7038=LINE('',#53638,#11913);
#7039=LINE('',#53640,#11914);
#7040=LINE('',#53644,#11915);
#7041=LINE('',#53647,#11916);
#7042=LINE('',#53649,#11917);
#7043=LINE('',#53651,#11918);
#7044=LINE('',#53654,#11919);
#7045=LINE('',#53656,#11920);
#7046=LINE('',#53659,#11921);
#7047=LINE('',#53661,#11922);
#7048=LINE('',#53664,#11923);
#7049=LINE('',#53666,#11924);
#7050=LINE('',#53669,#11925);
#7051=LINE('',#53671,#11926);
#7052=LINE('',#53674,#11927);
#7053=LINE('',#53676,#11928);
#7054=LINE('',#53679,#11929);
#7055=LINE('',#53681,#11930);
#7056=LINE('',#53684,#11931);
#7057=LINE('',#53686,#11932);
#7058=LINE('',#53689,#11933);
#7059=LINE('',#53691,#11934);
#7060=LINE('',#53694,#11935);
#7061=LINE('',#53696,#11936);
#7062=LINE('',#53699,#11937);
#7063=LINE('',#53701,#11938);
#7064=LINE('',#53704,#11939);
#7065=LINE('',#53706,#11940);
#7066=LINE('',#53709,#11941);
#7067=LINE('',#53712,#11942);
#7068=LINE('',#53714,#11943);
#7069=LINE('',#53717,#11944);
#7070=LINE('',#53719,#11945);
#7071=LINE('',#53722,#11946);
#7072=LINE('',#53724,#11947);
#7073=LINE('',#53727,#11948);
#7074=LINE('',#53729,#11949);
#7075=LINE('',#53732,#11950);
#7076=LINE('',#53734,#11951);
#7077=LINE('',#53737,#11952);
#7078=LINE('',#53739,#11953);
#7079=LINE('',#53742,#11954);
#7080=LINE('',#53744,#11955);
#7081=LINE('',#53747,#11956);
#7082=LINE('',#53749,#11957);
#7083=LINE('',#53752,#11958);
#7084=LINE('',#53754,#11959);
#7085=LINE('',#53757,#11960);
#7086=LINE('',#53759,#11961);
#7087=LINE('',#53762,#11962);
#7088=LINE('',#53764,#11963);
#7089=LINE('',#53767,#11964);
#7090=LINE('',#53769,#11965);
#7091=LINE('',#53772,#11966);
#7092=LINE('',#53774,#11967);
#7093=LINE('',#53777,#11968);
#7094=LINE('',#53779,#11969);
#7095=LINE('',#53782,#11970);
#7096=LINE('',#53784,#11971);
#7097=LINE('',#53787,#11972);
#7098=LINE('',#53789,#11973);
#7099=LINE('',#53792,#11974);
#7100=LINE('',#53794,#11975);
#7101=LINE('',#53797,#11976);
#7102=LINE('',#53799,#11977);
#7103=LINE('',#53802,#11978);
#7104=LINE('',#53804,#11979);
#7105=LINE('',#53807,#11980);
#7106=LINE('',#53809,#11981);
#7107=LINE('',#53812,#11982);
#7108=LINE('',#53814,#11983);
#7109=LINE('',#53817,#11984);
#7110=LINE('',#53819,#11985);
#7111=LINE('',#53822,#11986);
#7112=LINE('',#53824,#11987);
#7113=LINE('',#53827,#11988);
#7114=LINE('',#53829,#11989);
#7115=LINE('',#53831,#11990);
#7116=LINE('',#53834,#11991);
#7117=LINE('',#53836,#11992);
#7118=LINE('',#53839,#11993);
#7119=LINE('',#53841,#11994);
#7120=LINE('',#53844,#11995);
#7121=LINE('',#53846,#11996);
#7122=LINE('',#53849,#11997);
#7123=LINE('',#53851,#11998);
#7124=LINE('',#53854,#11999);
#7125=LINE('',#53856,#12000);
#7126=LINE('',#53859,#12001);
#7127=LINE('',#53861,#12002);
#7128=LINE('',#53864,#12003);
#7129=LINE('',#53866,#12004);
#7130=LINE('',#53869,#12005);
#7131=LINE('',#53871,#12006);
#7132=LINE('',#53874,#12007);
#7133=LINE('',#53876,#12008);
#7134=LINE('',#53879,#12009);
#7135=LINE('',#53881,#12010);
#7136=LINE('',#53884,#12011);
#7137=LINE('',#53886,#12012);
#7138=LINE('',#53891,#12013);
#7139=LINE('',#53893,#12014);
#7140=LINE('',#53895,#12015);
#7141=LINE('',#53897,#12016);
#7142=LINE('',#53901,#12017);
#7143=LINE('',#53905,#12018);
#7144=LINE('',#53907,#12019);
#7145=LINE('',#53908,#12020);
#7146=LINE('',#53910,#12021);
#7147=LINE('',#53913,#12022);
#7148=LINE('',#53915,#12023);
#7149=LINE('',#53918,#12024);
#7150=LINE('',#53920,#12025);
#7151=LINE('',#53923,#12026);
#7152=LINE('',#53925,#12027);
#7153=LINE('',#53928,#12028);
#7154=LINE('',#53930,#12029);
#7155=LINE('',#53933,#12030);
#7156=LINE('',#53935,#12031);
#7157=LINE('',#53938,#12032);
#7158=LINE('',#53940,#12033);
#7159=LINE('',#53943,#12034);
#7160=LINE('',#53945,#12035);
#7161=LINE('',#53948,#12036);
#7162=LINE('',#53950,#12037);
#7163=LINE('',#53953,#12038);
#7164=LINE('',#53955,#12039);
#7165=LINE('',#53958,#12040);
#7166=LINE('',#53960,#12041);
#7167=LINE('',#53963,#12042);
#7168=LINE('',#53965,#12043);
#7169=LINE('',#53968,#12044);
#7170=LINE('',#53970,#12045);
#7171=LINE('',#53973,#12046);
#7172=LINE('',#53975,#12047);
#7173=LINE('',#53977,#12048);
#7174=LINE('',#53980,#12049);
#7175=LINE('',#53982,#12050);
#7176=LINE('',#53985,#12051);
#7177=LINE('',#53987,#12052);
#7178=LINE('',#53990,#12053);
#7179=LINE('',#53992,#12054);
#7180=LINE('',#53995,#12055);
#7181=LINE('',#53997,#12056);
#7182=LINE('',#54000,#12057);
#7183=LINE('',#54002,#12058);
#7184=LINE('',#54005,#12059);
#7185=LINE('',#54007,#12060);
#7186=LINE('',#54010,#12061);
#7187=LINE('',#54012,#12062);
#7188=LINE('',#54015,#12063);
#7189=LINE('',#54017,#12064);
#7190=LINE('',#54020,#12065);
#7191=LINE('',#54022,#12066);
#7192=LINE('',#54025,#12067);
#7193=LINE('',#54027,#12068);
#7194=LINE('',#54030,#12069);
#7195=LINE('',#54032,#12070);
#7196=LINE('',#54035,#12071);
#7197=LINE('',#54037,#12072);
#7198=LINE('',#54040,#12073);
#7199=LINE('',#54042,#12074);
#7200=LINE('',#54045,#12075);
#7201=LINE('',#54047,#12076);
#7202=LINE('',#54050,#12077);
#7203=LINE('',#54052,#12078);
#7204=LINE('',#54055,#12079);
#7205=LINE('',#54057,#12080);
#7206=LINE('',#54060,#12081);
#7207=LINE('',#54062,#12082);
#7208=LINE('',#54065,#12083);
#7209=LINE('',#54067,#12084);
#7210=LINE('',#54070,#12085);
#7211=LINE('',#54072,#12086);
#7212=LINE('',#54075,#12087);
#7213=LINE('',#54077,#12088);
#7214=LINE('',#54080,#12089);
#7215=LINE('',#54082,#12090);
#7216=LINE('',#54085,#12091);
#7217=LINE('',#54087,#12092);
#7218=LINE('',#54090,#12093);
#7219=LINE('',#54092,#12094);
#7220=LINE('',#54095,#12095);
#7221=LINE('',#54098,#12096);
#7222=LINE('',#54100,#12097);
#7223=LINE('',#54103,#12098);
#7224=LINE('',#54105,#12099);
#7225=LINE('',#54108,#12100);
#7226=LINE('',#54110,#12101);
#7227=LINE('',#54113,#12102);
#7228=LINE('',#54115,#12103);
#7229=LINE('',#54118,#12104);
#7230=LINE('',#54120,#12105);
#7231=LINE('',#54123,#12106);
#7232=LINE('',#54125,#12107);
#7233=LINE('',#54128,#12108);
#7234=LINE('',#54130,#12109);
#7235=LINE('',#54133,#12110);
#7236=LINE('',#54135,#12111);
#7237=LINE('',#54138,#12112);
#7238=LINE('',#54140,#12113);
#7239=LINE('',#54143,#12114);
#7240=LINE('',#54145,#12115);
#7241=LINE('',#54148,#12116);
#7242=LINE('',#54151,#12117);
#7243=LINE('',#54153,#12118);
#7244=LINE('',#54154,#12119);
#7245=LINE('',#54157,#12120);
#7246=LINE('',#54159,#12121);
#7247=LINE('',#54160,#12122);
#7248=LINE('',#54164,#12123);
#7249=LINE('',#54166,#12124);
#7250=LINE('',#54168,#12125);
#7251=LINE('',#54169,#12126);
#7252=LINE('',#54172,#12127);
#7253=LINE('',#54174,#12128);
#7254=LINE('',#54175,#12129);
#7255=LINE('',#54179,#12130);
#7256=LINE('',#54181,#12131);
#7257=LINE('',#54183,#12132);
#7258=LINE('',#54184,#12133);
#7259=LINE('',#54187,#12134);
#7260=LINE('',#54189,#12135);
#7261=LINE('',#54190,#12136);
#7262=LINE('',#54193,#12137);
#7263=LINE('',#54195,#12138);
#7264=LINE('',#54196,#12139);
#7265=LINE('',#54200,#12140);
#7266=LINE('',#54202,#12141);
#7267=LINE('',#54204,#12142);
#7268=LINE('',#54205,#12143);
#7269=LINE('',#54209,#12144);
#7270=LINE('',#54211,#12145);
#7271=LINE('',#54213,#12146);
#7272=LINE('',#54214,#12147);
#7273=LINE('',#54217,#12148);
#7274=LINE('',#54219,#12149);
#7275=LINE('',#54220,#12150);
#7276=LINE('',#54224,#12151);
#7277=LINE('',#54226,#12152);
#7278=LINE('',#54228,#12153);
#7279=LINE('',#54229,#12154);
#7280=LINE('',#54233,#12155);
#7281=LINE('',#54235,#12156);
#7282=LINE('',#54237,#12157);
#7283=LINE('',#54238,#12158);
#7284=LINE('',#54241,#12159);
#7285=LINE('',#54243,#12160);
#7286=LINE('',#54244,#12161);
#7287=LINE('',#54247,#12162);
#7288=LINE('',#54249,#12163);
#7289=LINE('',#54250,#12164);
#7290=LINE('',#54254,#12165);
#7291=LINE('',#54256,#12166);
#7292=LINE('',#54258,#12167);
#7293=LINE('',#54259,#12168);
#7294=LINE('',#54262,#12169);
#7295=LINE('',#54264,#12170);
#7296=LINE('',#54265,#12171);
#7297=LINE('',#54269,#12172);
#7298=LINE('',#54271,#12173);
#7299=LINE('',#54273,#12174);
#7300=LINE('',#54274,#12175);
#7301=LINE('',#54277,#12176);
#7302=LINE('',#54279,#12177);
#7303=LINE('',#54280,#12178);
#7304=LINE('',#54283,#12179);
#7305=LINE('',#54285,#12180);
#7306=LINE('',#54286,#12181);
#7307=LINE('',#54290,#12182);
#7308=LINE('',#54292,#12183);
#7309=LINE('',#54294,#12184);
#7310=LINE('',#54295,#12185);
#7311=LINE('',#54299,#12186);
#7312=LINE('',#54301,#12187);
#7313=LINE('',#54303,#12188);
#7314=LINE('',#54304,#12189);
#7315=LINE('',#54307,#12190);
#7316=LINE('',#54309,#12191);
#7317=LINE('',#54310,#12192);
#7318=LINE('',#54314,#12193);
#7319=LINE('',#54316,#12194);
#7320=LINE('',#54318,#12195);
#7321=LINE('',#54319,#12196);
#7322=LINE('',#54323,#12197);
#7323=LINE('',#54325,#12198);
#7324=LINE('',#54327,#12199);
#7325=LINE('',#54328,#12200);
#7326=LINE('',#54371,#12201);
#7327=LINE('',#54386,#12202);
#7328=LINE('',#54406,#12203);
#7329=LINE('',#54418,#12204);
#7330=LINE('',#54426,#12205);
#7331=LINE('',#54436,#12206);
#7332=LINE('',#54450,#12207);
#7333=LINE('',#54461,#12208);
#7334=LINE('',#54475,#12209);
#7335=LINE('',#54489,#12210);
#7336=LINE('',#54500,#12211);
#7337=LINE('',#54513,#12212);
#7338=LINE('',#54526,#12213);
#7339=LINE('',#54538,#12214);
#7340=LINE('',#54824,#12215);
#7341=LINE('',#54825,#12216);
#7342=LINE('',#54866,#12217);
#7343=LINE('',#54894,#12218);
#7344=LINE('',#54935,#12219);
#7345=LINE('',#54952,#12220);
#7346=LINE('',#54954,#12221);
#7347=LINE('',#54956,#12222);
#7348=LINE('',#54958,#12223);
#7349=LINE('',#54962,#12224);
#7350=LINE('',#54966,#12225);
#7351=LINE('',#54968,#12226);
#7352=LINE('',#54969,#12227);
#7353=LINE('',#54972,#12228);
#7354=LINE('',#54974,#12229);
#7355=LINE('',#54976,#12230);
#7356=LINE('',#54977,#12231);
#7357=LINE('',#54982,#12232);
#7358=LINE('',#54986,#12233);
#7359=LINE('',#54990,#12234);
#7360=LINE('',#54994,#12235);
#7361=LINE('',#54998,#12236);
#7362=LINE('',#55001,#12237);
#7363=LINE('',#55005,#12238);
#7364=LINE('',#55007,#12239);
#7365=LINE('',#55009,#12240);
#7366=LINE('',#55011,#12241);
#7367=LINE('',#55013,#12242);
#7368=LINE('',#55015,#12243);
#7369=LINE('',#55019,#12244);
#7370=LINE('',#55022,#12245);
#7371=LINE('',#55025,#12246);
#7372=LINE('',#55027,#12247);
#7373=LINE('',#55029,#12248);
#7374=LINE('',#55030,#12249);
#7375=LINE('',#55033,#12250);
#7376=LINE('',#55037,#12251);
#7377=LINE('',#55041,#12252);
#7378=LINE('',#55045,#12253);
#7379=LINE('',#55049,#12254);
#7380=LINE('',#55053,#12255);
#7381=LINE('',#55057,#12256);
#7382=LINE('',#55058,#12257);
#7383=LINE('',#55059,#12258);
#7384=LINE('',#55063,#12259);
#7385=LINE('',#55064,#12260);
#7386=LINE('',#55065,#12261);
#7387=LINE('',#55069,#12262);
#7388=LINE('',#55070,#12263);
#7389=LINE('',#55071,#12264);
#7390=LINE('',#55075,#12265);
#7391=LINE('',#55076,#12266);
#7392=LINE('',#55077,#12267);
#7393=LINE('',#55140,#12268);
#7394=LINE('',#55141,#12269);
#7395=LINE('',#55226,#12270);
#7396=LINE('',#55227,#12271);
#7397=LINE('',#55294,#12272);
#7398=LINE('',#55295,#12273);
#7399=LINE('',#55297,#12274);
#7400=LINE('',#55299,#12275);
#7401=LINE('',#55300,#12276);
#7402=LINE('',#55302,#12277);
#7403=LINE('',#55303,#12278);
#7404=LINE('',#55305,#12279);
#7405=LINE('',#55349,#12280);
#7406=LINE('',#55350,#12281);
#7407=LINE('',#55475,#12282);
#7408=LINE('',#55476,#12283);
#7409=LINE('',#55523,#12284);
#7410=LINE('',#55524,#12285);
#7411=LINE('',#55526,#12286);
#7412=LINE('',#55528,#12287);
#7413=LINE('',#55529,#12288);
#7414=LINE('',#55531,#12289);
#7415=LINE('',#55532,#12290);
#7416=LINE('',#55534,#12291);
#7417=LINE('',#55547,#12292);
#7418=LINE('',#55553,#12293);
#7419=LINE('',#55559,#12294);
#7420=LINE('',#55563,#12295);
#7421=LINE('',#55566,#12296);
#7422=LINE('',#55570,#12297);
#7423=LINE('',#55574,#12298);
#7424=LINE('',#55577,#12299);
#7425=LINE('',#55582,#12300);
#7426=LINE('',#55586,#12301);
#7427=LINE('',#55589,#12302);
#7428=LINE('',#55593,#12303);
#7429=LINE('',#55597,#12304);
#7430=LINE('',#55600,#12305);
#7431=LINE('',#55602,#12306);
#7432=LINE('',#55603,#12307);
#7433=LINE('',#55605,#12308);
#7434=LINE('',#55606,#12309);
#7435=LINE('',#55611,#12310);
#7436=LINE('',#55612,#12311);
#7437=LINE('',#55614,#12312);
#7438=LINE('',#55615,#12313);
#7439=LINE('',#55617,#12314);
#7440=LINE('',#55619,#12315);
#7441=LINE('',#55633,#12316);
#7442=LINE('',#55639,#12317);
#7443=LINE('',#55645,#12318);
#7444=LINE('',#55649,#12319);
#7445=LINE('',#55652,#12320);
#7446=LINE('',#55656,#12321);
#7447=LINE('',#55660,#12322);
#7448=LINE('',#55663,#12323);
#7449=LINE('',#55668,#12324);
#7450=LINE('',#55672,#12325);
#7451=LINE('',#55675,#12326);
#7452=LINE('',#55679,#12327);
#7453=LINE('',#55683,#12328);
#7454=LINE('',#55686,#12329);
#7455=LINE('',#55688,#12330);
#7456=LINE('',#55689,#12331);
#7457=LINE('',#55691,#12332);
#7458=LINE('',#55692,#12333);
#7459=LINE('',#55697,#12334);
#7460=LINE('',#55698,#12335);
#7461=LINE('',#55700,#12336);
#7462=LINE('',#55701,#12337);
#7463=LINE('',#55703,#12338);
#7464=LINE('',#55705,#12339);
#7465=LINE('',#55719,#12340);
#7466=LINE('',#55725,#12341);
#7467=LINE('',#55731,#12342);
#7468=LINE('',#55735,#12343);
#7469=LINE('',#55738,#12344);
#7470=LINE('',#55742,#12345);
#7471=LINE('',#55746,#12346);
#7472=LINE('',#55749,#12347);
#7473=LINE('',#55754,#12348);
#7474=LINE('',#55758,#12349);
#7475=LINE('',#55761,#12350);
#7476=LINE('',#55765,#12351);
#7477=LINE('',#55769,#12352);
#7478=LINE('',#55772,#12353);
#7479=LINE('',#55774,#12354);
#7480=LINE('',#55775,#12355);
#7481=LINE('',#55777,#12356);
#7482=LINE('',#55778,#12357);
#7483=LINE('',#55783,#12358);
#7484=LINE('',#55784,#12359);
#7485=LINE('',#55786,#12360);
#7486=LINE('',#55787,#12361);
#7487=LINE('',#55789,#12362);
#7488=LINE('',#55791,#12363);
#7489=LINE('',#55805,#12364);
#7490=LINE('',#55811,#12365);
#7491=LINE('',#55817,#12366);
#7492=LINE('',#55821,#12367);
#7493=LINE('',#55824,#12368);
#7494=LINE('',#55828,#12369);
#7495=LINE('',#55832,#12370);
#7496=LINE('',#55835,#12371);
#7497=LINE('',#55840,#12372);
#7498=LINE('',#55844,#12373);
#7499=LINE('',#55847,#12374);
#7500=LINE('',#55851,#12375);
#7501=LINE('',#55855,#12376);
#7502=LINE('',#55858,#12377);
#7503=LINE('',#55860,#12378);
#7504=LINE('',#55861,#12379);
#7505=LINE('',#55863,#12380);
#7506=LINE('',#55864,#12381);
#7507=LINE('',#55869,#12382);
#7508=LINE('',#55870,#12383);
#7509=LINE('',#55872,#12384);
#7510=LINE('',#55873,#12385);
#7511=LINE('',#55875,#12386);
#7512=LINE('',#55877,#12387);
#7513=LINE('',#55899,#12388);
#7514=LINE('',#55913,#12389);
#7515=LINE('',#55924,#12390);
#7516=LINE('',#55939,#12391);
#7517=LINE('',#55949,#12392);
#7518=LINE('',#55962,#12393);
#7519=LINE('',#55975,#12394);
#7520=LINE('',#55988,#12395);
#7521=LINE('',#56000,#12396);
#7522=LINE('',#56011,#12397);
#7523=LINE('',#56024,#12398);
#7524=LINE('',#56266,#12399);
#7525=LINE('',#56267,#12400);
#7526=LINE('',#56269,#12401);
#7527=LINE('',#56271,#12402);
#7528=LINE('',#56272,#12403);
#7529=LINE('',#56274,#12404);
#7530=LINE('',#56276,#12405);
#7531=LINE('',#56277,#12406);
#7532=LINE('',#56279,#12407);
#7533=LINE('',#56281,#12408);
#7534=LINE('',#56283,#12409);
#7535=LINE('',#56284,#12410);
#7536=LINE('',#56286,#12411);
#7537=LINE('',#56287,#12412);
#7538=LINE('',#56289,#12413);
#7539=LINE('',#56291,#12414);
#7540=LINE('',#56292,#12415);
#7541=LINE('',#56294,#12416);
#7542=LINE('',#56295,#12417);
#7543=LINE('',#56312,#12418);
#7544=LINE('',#56313,#12419);
#7545=LINE('',#56330,#12420);
#7546=LINE('',#56347,#12421);
#7547=LINE('',#56348,#12422);
#7548=LINE('',#56365,#12423);
#7549=LINE('',#56390,#12424);
#7550=LINE('',#56407,#12425);
#7551=LINE('',#56424,#12426);
#7552=LINE('',#56425,#12427);
#7553=LINE('',#56442,#12428);
#7554=LINE('',#56459,#12429);
#7555=LINE('',#56460,#12430);
#7556=LINE('',#56479,#12431);
#7557=LINE('',#56480,#12432);
#7558=LINE('',#56499,#12433);
#7559=LINE('',#56516,#12434);
#7560=LINE('',#56517,#12435);
#7561=LINE('',#56534,#12436);
#7562=LINE('',#56551,#12437);
#7563=LINE('',#56552,#12438);
#7564=LINE('',#56569,#12439);
#7565=LINE('',#56590,#12440);
#7566=LINE('',#56607,#12441);
#7567=LINE('',#56624,#12442);
#7568=LINE('',#56625,#12443);
#7569=LINE('',#56642,#12444);
#7570=LINE('',#56659,#12445);
#7571=LINE('',#56660,#12446);
#7572=LINE('',#56675,#12447);
#7573=LINE('',#56676,#12448);
#7574=LINE('',#56691,#12449);
#7575=LINE('',#56704,#12450);
#7576=LINE('',#56717,#12451);
#7577=LINE('',#56728,#12452);
#7578=LINE('',#56741,#12453);
#7579=LINE('',#56742,#12454);
#7580=LINE('',#56755,#12455);
#7581=LINE('',#56756,#12456);
#7582=LINE('',#56771,#12457);
#7583=LINE('',#56772,#12458);
#7584=LINE('',#56828,#12459);
#7585=LINE('',#56829,#12460);
#7586=LINE('',#56831,#12461);
#7587=LINE('',#56833,#12462);
#7588=LINE('',#56835,#12463);
#7589=LINE('',#56837,#12464);
#7590=LINE('',#56839,#12465);
#7591=LINE('',#56841,#12466);
#7592=LINE('',#56843,#12467);
#7593=LINE('',#56845,#12468);
#7594=LINE('',#56847,#12469);
#7595=LINE('',#56849,#12470);
#7596=LINE('',#56852,#12471);
#7597=LINE('',#56853,#12472);
#7598=LINE('',#56855,#12473);
#7599=LINE('',#56857,#12474);
#7600=LINE('',#56864,#12475);
#7601=LINE('',#56866,#12476);
#7602=LINE('',#56869,#12477);
#7603=LINE('',#56871,#12478);
#7604=LINE('',#56874,#12479);
#7605=LINE('',#56876,#12480);
#7606=LINE('',#56879,#12481);
#7607=LINE('',#56881,#12482);
#7608=LINE('',#56884,#12483);
#7609=LINE('',#56886,#12484);
#7610=LINE('',#56889,#12485);
#7611=LINE('',#56891,#12486);
#7612=LINE('',#56894,#12487);
#7613=LINE('',#56896,#12488);
#7614=LINE('',#56899,#12489);
#7615=LINE('',#56901,#12490);
#7616=LINE('',#56904,#12491);
#7617=LINE('',#56906,#12492);
#7618=LINE('',#56909,#12493);
#7619=LINE('',#56911,#12494);
#7620=LINE('',#56914,#12495);
#7621=LINE('',#56916,#12496);
#7622=LINE('',#56919,#12497);
#7623=LINE('',#56921,#12498);
#7624=LINE('',#56924,#12499);
#7625=LINE('',#56926,#12500);
#7626=LINE('',#56929,#12501);
#7627=LINE('',#56931,#12502);
#7628=LINE('',#56934,#12503);
#7629=LINE('',#56936,#12504);
#7630=LINE('',#56939,#12505);
#7631=LINE('',#56941,#12506);
#7632=LINE('',#56944,#12507);
#7633=LINE('',#56946,#12508);
#7634=LINE('',#56949,#12509);
#7635=LINE('',#56951,#12510);
#7636=LINE('',#56954,#12511);
#7637=LINE('',#56956,#12512);
#7638=LINE('',#56959,#12513);
#7639=LINE('',#56961,#12514);
#7640=LINE('',#56964,#12515);
#7641=LINE('',#56966,#12516);
#7642=LINE('',#56969,#12517);
#7643=LINE('',#56971,#12518);
#7644=LINE('',#56974,#12519);
#7645=LINE('',#56976,#12520);
#7646=LINE('',#56979,#12521);
#7647=LINE('',#56981,#12522);
#7648=LINE('',#56984,#12523);
#7649=LINE('',#56986,#12524);
#7650=LINE('',#56989,#12525);
#7651=LINE('',#56991,#12526);
#7652=LINE('',#56994,#12527);
#7653=LINE('',#56996,#12528);
#7654=LINE('',#56999,#12529);
#7655=LINE('',#57001,#12530);
#7656=LINE('',#57004,#12531);
#7657=LINE('',#57006,#12532);
#7658=LINE('',#57009,#12533);
#7659=LINE('',#57011,#12534);
#7660=LINE('',#57014,#12535);
#7661=LINE('',#57016,#12536);
#7662=LINE('',#57019,#12537);
#7663=LINE('',#57021,#12538);
#7664=LINE('',#57024,#12539);
#7665=LINE('',#57026,#12540);
#7666=LINE('',#57029,#12541);
#7667=LINE('',#57031,#12542);
#7668=LINE('',#57034,#12543);
#7669=LINE('',#57036,#12544);
#7670=LINE('',#57039,#12545);
#7671=LINE('',#57041,#12546);
#7672=LINE('',#57044,#12547);
#7673=LINE('',#57046,#12548);
#7674=LINE('',#57049,#12549);
#7675=LINE('',#57051,#12550);
#7676=LINE('',#57054,#12551);
#7677=LINE('',#57056,#12552);
#7678=LINE('',#57059,#12553);
#7679=LINE('',#57061,#12554);
#7680=LINE('',#57064,#12555);
#7681=LINE('',#57066,#12556);
#7682=LINE('',#57069,#12557);
#7683=LINE('',#57071,#12558);
#7684=LINE('',#57074,#12559);
#7685=LINE('',#57076,#12560);
#7686=LINE('',#57079,#12561);
#7687=LINE('',#57081,#12562);
#7688=LINE('',#57084,#12563);
#7689=LINE('',#57086,#12564);
#7690=LINE('',#57089,#12565);
#7691=LINE('',#57091,#12566);
#7692=LINE('',#57094,#12567);
#7693=LINE('',#57096,#12568);
#7694=LINE('',#57099,#12569);
#7695=LINE('',#57101,#12570);
#7696=LINE('',#57104,#12571);
#7697=LINE('',#57106,#12572);
#7698=LINE('',#57108,#12573);
#7699=LINE('',#57110,#12574);
#7700=LINE('',#57111,#12575);
#7701=LINE('',#57113,#12576);
#7702=LINE('',#57116,#12577);
#7703=LINE('',#57121,#12578);
#7704=LINE('',#57126,#12579);
#7705=LINE('',#57128,#12580);
#7706=LINE('',#57130,#12581);
#7707=LINE('',#57132,#12582);
#7708=LINE('',#57144,#12583);
#7709=LINE('',#57150,#12584);
#7710=LINE('',#57156,#12585);
#7711=LINE('',#57160,#12586);
#7712=LINE('',#57164,#12587);
#7713=LINE('',#57167,#12588);
#7714=LINE('',#57171,#12589);
#7715=LINE('',#57174,#12590);
#7716=LINE('',#57179,#12591);
#7717=LINE('',#57183,#12592);
#7718=LINE('',#57187,#12593);
#7719=LINE('',#57190,#12594);
#7720=LINE('',#57194,#12595);
#7721=LINE('',#57197,#12596);
#7722=LINE('',#57199,#12597);
#7723=LINE('',#57200,#12598);
#7724=LINE('',#57202,#12599);
#7725=LINE('',#57203,#12600);
#7726=LINE('',#57208,#12601);
#7727=LINE('',#57209,#12602);
#7728=LINE('',#57211,#12603);
#7729=LINE('',#57212,#12604);
#7730=LINE('',#57214,#12605);
#7731=LINE('',#57216,#12606);
#7732=LINE('',#57230,#12607);
#7733=LINE('',#57236,#12608);
#7734=LINE('',#57242,#12609);
#7735=LINE('',#57246,#12610);
#7736=LINE('',#57250,#12611);
#7737=LINE('',#57253,#12612);
#7738=LINE('',#57257,#12613);
#7739=LINE('',#57260,#12614);
#7740=LINE('',#57265,#12615);
#7741=LINE('',#57269,#12616);
#7742=LINE('',#57273,#12617);
#7743=LINE('',#57276,#12618);
#7744=LINE('',#57280,#12619);
#7745=LINE('',#57283,#12620);
#7746=LINE('',#57285,#12621);
#7747=LINE('',#57286,#12622);
#7748=LINE('',#57288,#12623);
#7749=LINE('',#57289,#12624);
#7750=LINE('',#57294,#12625);
#7751=LINE('',#57295,#12626);
#7752=LINE('',#57297,#12627);
#7753=LINE('',#57298,#12628);
#7754=LINE('',#57300,#12629);
#7755=LINE('',#57302,#12630);
#7756=LINE('',#57307,#12631);
#7757=LINE('',#57309,#12632);
#7758=LINE('',#57311,#12633);
#7759=LINE('',#57313,#12634);
#7760=LINE('',#57314,#12635);
#7761=LINE('',#57316,#12636);
#7762=LINE('',#57321,#12637);
#7763=LINE('',#57328,#12638);
#7764=LINE('',#57331,#12639);
#7765=LINE('',#57333,#12640);
#7766=LINE('',#57336,#12641);
#7767=LINE('',#57338,#12642);
#7768=LINE('',#57339,#12643);
#7769=LINE('',#57342,#12644);
#7770=LINE('',#57344,#12645);
#7771=LINE('',#57345,#12646);
#7772=LINE('',#57350,#12647);
#7773=LINE('',#57356,#12648);
#7774=LINE('',#57359,#12649);
#7775=LINE('',#57361,#12650);
#7776=LINE('',#57368,#12651);
#7777=LINE('',#57374,#12652);
#7778=LINE('',#57380,#12653);
#7779=LINE('',#57388,#12654);
#7780=LINE('',#57396,#12655);
#7781=LINE('',#57400,#12656);
#7782=LINE('',#57407,#12657);
#7783=LINE('',#57410,#12658);
#7784=LINE('',#57413,#12659);
#7785=LINE('',#57420,#12660);
#7786=LINE('',#57424,#12661);
#7787=LINE('',#57428,#12662);
#7788=LINE('',#57432,#12663);
#7789=LINE('',#57436,#12664);
#7790=LINE('',#57439,#12665);
#7791=LINE('',#57442,#12666);
#7792=LINE('',#57444,#12667);
#7793=LINE('',#57446,#12668);
#7794=LINE('',#57447,#12669);
#7795=LINE('',#57450,#12670);
#7796=LINE('',#57452,#12671);
#7797=LINE('',#57454,#12672);
#7798=LINE('',#57455,#12673);
#7799=LINE('',#57458,#12674);
#7800=LINE('',#57460,#12675);
#7801=LINE('',#57462,#12676);
#7802=LINE('',#57463,#12677);
#7803=LINE('',#57467,#12678);
#7804=LINE('',#57469,#12679);
#7805=LINE('',#57471,#12680);
#7806=LINE('',#57472,#12681);
#7807=LINE('',#57476,#12682);
#7808=LINE('',#57478,#12683);
#7809=LINE('',#57479,#12684);
#7810=LINE('',#57481,#12685);
#7811=LINE('',#57482,#12686);
#7812=LINE('',#57486,#12687);
#7813=LINE('',#57488,#12688);
#7814=LINE('',#57489,#12689);
#7815=LINE('',#57491,#12690);
#7816=LINE('',#57492,#12691);
#7817=LINE('',#57494,#12692);
#7818=LINE('',#57495,#12693);
#7819=LINE('',#57499,#12694);
#7820=LINE('',#57501,#12695);
#7821=LINE('',#57503,#12696);
#7822=LINE('',#57505,#12697);
#7823=LINE('',#57507,#12698);
#7824=LINE('',#57508,#12699);
#7825=LINE('',#57512,#12700);
#7826=LINE('',#57513,#12701);
#7827=LINE('',#57514,#12702);
#7828=LINE('',#57517,#12703);
#7829=LINE('',#57519,#12704);
#7830=LINE('',#57521,#12705);
#7831=LINE('',#57523,#12706);
#7832=LINE('',#57524,#12707);
#7833=LINE('',#57526,#12708);
#7834=LINE('',#57527,#12709);
#7835=LINE('',#57531,#12710);
#7836=LINE('',#57533,#12711);
#7837=LINE('',#57535,#12712);
#7838=LINE('',#57536,#12713);
#7839=LINE('',#57540,#12714);
#7840=LINE('',#57541,#12715);
#7841=LINE('',#57543,#12716);
#7842=LINE('',#57545,#12717);
#7843=LINE('',#57546,#12718);
#7844=LINE('',#57549,#12719);
#7845=LINE('',#57551,#12720);
#7846=LINE('',#57553,#12721);
#7847=LINE('',#57555,#12722);
#7848=LINE('',#57556,#12723);
#7849=LINE('',#57558,#12724);
#7850=LINE('',#57559,#12725);
#7851=LINE('',#57565,#12726);
#7852=LINE('',#57569,#12727);
#7853=LINE('',#57573,#12728);
#7854=LINE('',#57577,#12729);
#7855=LINE('',#57581,#12730);
#7856=LINE('',#57584,#12731);
#7857=LINE('',#57585,#12732);
#7858=LINE('',#57586,#12733);
#7859=LINE('',#57587,#12734);
#7860=LINE('',#57591,#12735);
#7861=LINE('',#57595,#12736);
#7862=LINE('',#57599,#12737);
#7863=LINE('',#57603,#12738);
#7864=LINE('',#57609,#12739);
#7865=LINE('',#57613,#12740);
#7866=LINE('',#57617,#12741);
#7867=LINE('',#57621,#12742);
#7868=LINE('',#57625,#12743);
#7869=LINE('',#57628,#12744);
#7870=LINE('',#57631,#12745);
#7871=LINE('',#57635,#12746);
#7872=LINE('',#57639,#12747);
#7873=LINE('',#57643,#12748);
#7874=LINE('',#57647,#12749);
#7875=LINE('',#57650,#12750);
#7876=LINE('',#57653,#12751);
#7877=LINE('',#57657,#12752);
#7878=LINE('',#57661,#12753);
#7879=LINE('',#57665,#12754);
#7880=LINE('',#57669,#12755);
#7881=LINE('',#57673,#12756);
#7882=LINE('',#57678,#12757);
#7883=LINE('',#57681,#12758);
#7884=LINE('',#57683,#12759);
#7885=LINE('',#57688,#12760);
#7886=LINE('',#57689,#12761);
#7887=LINE('',#57690,#12762);
#7888=LINE('',#57694,#12763);
#7889=LINE('',#57697,#12764);
#7890=LINE('',#57699,#12765);
#7891=LINE('',#57704,#12766);
#7892=LINE('',#57705,#12767);
#7893=LINE('',#57706,#12768);
#7894=LINE('',#57709,#12769);
#7895=LINE('',#57713,#12770);
#7896=LINE('',#57715,#12771);
#7897=LINE('',#57718,#12772);
#7898=LINE('',#57722,#12773);
#7899=LINE('',#57724,#12774);
#7900=LINE('',#57727,#12775);
#7901=LINE('',#57728,#12776);
#7902=LINE('',#57731,#12777);
#7903=LINE('',#57734,#12778);
#7904=LINE('',#57737,#12779);
#7905=LINE('',#57739,#12780);
#7906=LINE('',#57758,#12781);
#7907=LINE('',#57759,#12782);
#7908=LINE('',#57761,#12783);
#7909=LINE('',#57763,#12784);
#7910=LINE('',#57765,#12785);
#7911=LINE('',#57767,#12786);
#7912=LINE('',#57769,#12787);
#7913=LINE('',#57771,#12788);
#7914=LINE('',#57773,#12789);
#7915=LINE('',#57775,#12790);
#7916=LINE('',#57777,#12791);
#7917=LINE('',#57779,#12792);
#7918=LINE('',#57782,#12793);
#7919=LINE('',#57783,#12794);
#7920=LINE('',#57785,#12795);
#7921=LINE('',#57787,#12796);
#7922=LINE('',#57789,#12797);
#7923=LINE('',#57791,#12798);
#7924=LINE('',#57793,#12799);
#7925=LINE('',#57795,#12800);
#7926=LINE('',#57797,#12801);
#7927=LINE('',#57799,#12802);
#7928=LINE('',#57801,#12803);
#7929=LINE('',#57803,#12804);
#7930=LINE('',#57806,#12805);
#7931=LINE('',#57808,#12806);
#7932=LINE('',#57810,#12807);
#7933=LINE('',#57820,#12808);
#7934=LINE('',#57822,#12809);
#7935=LINE('',#57824,#12810);
#7936=LINE('',#57825,#12811);
#7937=LINE('',#57828,#12812);
#7938=LINE('',#57830,#12813);
#7939=LINE('',#57832,#12814);
#7940=LINE('',#57833,#12815);
#7941=LINE('',#57835,#12816);
#7942=LINE('',#57836,#12817);
#7943=LINE('',#57838,#12818);
#7944=LINE('',#57840,#12819);
#7945=LINE('',#57845,#12820);
#7946=LINE('',#57847,#12821);
#7947=LINE('',#57849,#12822);
#7948=LINE('',#57850,#12823);
#7949=LINE('',#57853,#12824);
#7950=LINE('',#57855,#12825);
#7951=LINE('',#57856,#12826);
#7952=LINE('',#57859,#12827);
#7953=LINE('',#57861,#12828);
#7954=LINE('',#57862,#12829);
#7955=LINE('',#57864,#12830);
#7956=LINE('',#57865,#12831);
#7957=LINE('',#57867,#12832);
#7958=LINE('',#57869,#12833);
#7959=LINE('',#57873,#12834);
#7960=LINE('',#57875,#12835);
#7961=LINE('',#57876,#12836);
#7962=LINE('',#57879,#12837);
#7963=LINE('',#57880,#12838);
#7964=LINE('',#57883,#12839);
#7965=LINE('',#57884,#12840);
#7966=LINE('',#57886,#12841);
#7967=LINE('',#57890,#12842);
#7968=LINE('',#57892,#12843);
#7969=LINE('',#57894,#12844);
#7970=LINE('',#57895,#12845);
#7971=LINE('',#57899,#12846);
#7972=LINE('',#57901,#12847);
#7973=LINE('',#57903,#12848);
#7974=LINE('',#57904,#12849);
#7975=LINE('',#57907,#12850);
#7976=LINE('',#57909,#12851);
#7977=LINE('',#57910,#12852);
#7978=LINE('',#57914,#12853);
#7979=LINE('',#57915,#12854);
#7980=LINE('',#57916,#12855);
#7981=LINE('',#57918,#12856);
#7982=LINE('',#57919,#12857);
#7983=LINE('',#57921,#12858);
#7984=LINE('',#57922,#12859);
#7985=LINE('',#57928,#12860);
#7986=LINE('',#57930,#12861);
#7987=LINE('',#57932,#12862);
#7988=LINE('',#57933,#12863);
#7989=LINE('',#57936,#12864);
#7990=LINE('',#57938,#12865);
#7991=LINE('',#57940,#12866);
#7992=LINE('',#57941,#12867);
#7993=LINE('',#57943,#12868);
#7994=LINE('',#57944,#12869);
#7995=LINE('',#57946,#12870);
#7996=LINE('',#57948,#12871);
#7997=LINE('',#57953,#12872);
#7998=LINE('',#57955,#12873);
#7999=LINE('',#57957,#12874);
#8000=LINE('',#57958,#12875);
#8001=LINE('',#57962,#12876);
#8002=LINE('',#57963,#12877);
#8003=LINE('',#57964,#12878);
#8004=LINE('',#57967,#12879);
#8005=LINE('',#57969,#12880);
#8006=LINE('',#57970,#12881);
#8007=LINE('',#57972,#12882);
#8008=LINE('',#57973,#12883);
#8009=LINE('',#57975,#12884);
#8010=LINE('',#57976,#12885);
#8011=LINE('',#57983,#12886);
#8012=LINE('',#57985,#12887);
#8013=LINE('',#57987,#12888);
#8014=LINE('',#57988,#12889);
#8015=LINE('',#57992,#12890);
#8016=LINE('',#57994,#12891);
#8017=LINE('',#57996,#12892);
#8018=LINE('',#57997,#12893);
#8019=LINE('',#57999,#12894);
#8020=LINE('',#58000,#12895);
#8021=LINE('',#58002,#12896);
#8022=LINE('',#58004,#12897);
#8023=LINE('',#58010,#12898);
#8024=LINE('',#58016,#12899);
#8025=LINE('',#58023,#12900);
#8026=LINE('',#58026,#12901);
#8027=LINE('',#58030,#12902);
#8028=LINE('',#58032,#12903);
#8029=LINE('',#58034,#12904);
#8030=LINE('',#58035,#12905);
#8031=LINE('',#58039,#12906);
#8032=LINE('',#58041,#12907);
#8033=LINE('',#58043,#12908);
#8034=LINE('',#58044,#12909);
#8035=LINE('',#58047,#12910);
#8036=LINE('',#58049,#12911);
#8037=LINE('',#58051,#12912);
#8038=LINE('',#58053,#12913);
#8039=LINE('',#58054,#12914);
#8040=LINE('',#58057,#12915);
#8041=LINE('',#58059,#12916);
#8042=LINE('',#58061,#12917);
#8043=LINE('',#58063,#12918);
#8044=LINE('',#58064,#12919);
#8045=LINE('',#58068,#12920);
#8046=LINE('',#58070,#12921);
#8047=LINE('',#58072,#12922);
#8048=LINE('',#58073,#12923);
#8049=LINE('',#58077,#12924);
#8050=LINE('',#58079,#12925);
#8051=LINE('',#58081,#12926);
#8052=LINE('',#58082,#12927);
#8053=LINE('',#58085,#12928);
#8054=LINE('',#58087,#12929);
#8055=LINE('',#58089,#12930);
#8056=LINE('',#58091,#12931);
#8057=LINE('',#58092,#12932);
#8058=LINE('',#58095,#12933);
#8059=LINE('',#58097,#12934);
#8060=LINE('',#58099,#12935);
#8061=LINE('',#58101,#12936);
#8062=LINE('',#58102,#12937);
#8063=LINE('',#58106,#12938);
#8064=LINE('',#58108,#12939);
#8065=LINE('',#58110,#12940);
#8066=LINE('',#58111,#12941);
#8067=LINE('',#58114,#12942);
#8068=LINE('',#58115,#12943);
#8069=LINE('',#58116,#12944);
#8070=LINE('',#58117,#12945);
#8071=LINE('',#58120,#12946);
#8072=LINE('',#58121,#12947);
#8073=LINE('',#58122,#12948);
#8074=LINE('',#58123,#12949);
#8075=LINE('',#58127,#12950);
#8076=LINE('',#58129,#12951);
#8077=LINE('',#58131,#12952);
#8078=LINE('',#58132,#12953);
#8079=LINE('',#58135,#12954);
#8080=LINE('',#58137,#12955);
#8081=LINE('',#58139,#12956);
#8082=LINE('',#58141,#12957);
#8083=LINE('',#58143,#12958);
#8084=LINE('',#58145,#12959);
#8085=LINE('',#58147,#12960);
#8086=LINE('',#58149,#12961);
#8087=LINE('',#58151,#12962);
#8088=LINE('',#58152,#12963);
#8089=LINE('',#58155,#12964);
#8090=LINE('',#58157,#12965);
#8091=LINE('',#58158,#12966);
#8092=LINE('',#58161,#12967);
#8093=LINE('',#58162,#12968);
#8094=LINE('',#58165,#12969);
#8095=LINE('',#58166,#12970);
#8096=LINE('',#58168,#12971);
#8097=LINE('',#58172,#12972);
#8098=LINE('',#58174,#12973);
#8099=LINE('',#58176,#12974);
#8100=LINE('',#58177,#12975);
#8101=LINE('',#58183,#12976);
#8102=LINE('',#58185,#12977);
#8103=LINE('',#58186,#12978);
#8104=LINE('',#58188,#12979);
#8105=LINE('',#58190,#12980);
#8106=LINE('',#58191,#12981);
#8107=LINE('',#58193,#12982);
#8108=LINE('',#58195,#12983);
#8109=LINE('',#58196,#12984);
#8110=LINE('',#58198,#12985);
#8111=LINE('',#58200,#12986);
#8112=LINE('',#58201,#12987);
#8113=LINE('',#58204,#12988);
#8114=LINE('',#58205,#12989);
#8115=LINE('',#58211,#12990);
#8116=LINE('',#58213,#12991);
#8117=LINE('',#58214,#12992);
#8118=LINE('',#58216,#12993);
#8119=LINE('',#58218,#12994);
#8120=LINE('',#58219,#12995);
#8121=LINE('',#58221,#12996);
#8122=LINE('',#58222,#12997);
#8123=LINE('',#58224,#12998);
#8124=LINE('',#58226,#12999);
#8125=LINE('',#58227,#13000);
#8126=LINE('',#58229,#13001);
#8127=LINE('',#58231,#13002);
#8128=LINE('',#58234,#13003);
#8129=LINE('',#58235,#13004);
#8130=LINE('',#58238,#13005);
#8131=LINE('',#58239,#13006);
#8132=LINE('',#58242,#13007);
#8133=LINE('',#58244,#13008);
#8134=LINE('',#58245,#13009);
#8135=LINE('',#58246,#13010);
#8136=LINE('',#58248,#13011);
#8137=LINE('',#58250,#13012);
#8138=LINE('',#58251,#13013);
#8139=LINE('',#58254,#13014);
#8140=LINE('',#58257,#13015);
#8141=LINE('',#58258,#13016);
#8142=LINE('',#58261,#13017);
#8143=LINE('',#58262,#13018);
#8144=LINE('',#58265,#13019);
#8145=LINE('',#58267,#13020);
#8146=LINE('',#58268,#13021);
#8147=LINE('',#58269,#13022);
#8148=LINE('',#58271,#13023);
#8149=LINE('',#58273,#13024);
#8150=LINE('',#58274,#13025);
#8151=LINE('',#58279,#13026);
#8152=LINE('',#58281,#13027);
#8153=LINE('',#58282,#13028);
#8154=LINE('',#58286,#13029);
#8155=LINE('',#58288,#13030);
#8156=LINE('',#58289,#13031);
#8157=LINE('',#58291,#13032);
#8158=LINE('',#58292,#13033);
#8159=LINE('',#58296,#13034);
#8160=LINE('',#58298,#13035);
#8161=LINE('',#58299,#13036);
#8162=LINE('',#58303,#13037);
#8163=LINE('',#58305,#13038);
#8164=LINE('',#58306,#13039);
#8165=LINE('',#58308,#13040);
#8166=LINE('',#58309,#13041);
#8167=LINE('',#58317,#13042);
#8168=LINE('',#58318,#13043);
#8169=LINE('',#58320,#13044);
#8170=LINE('',#58321,#13045);
#8171=LINE('',#58323,#13046);
#8172=LINE('',#58326,#13047);
#8173=LINE('',#58329,#13048);
#8174=LINE('',#58332,#13049);
#8175=LINE('',#58335,#13050);
#8176=LINE('',#58336,#13051);
#8177=LINE('',#58338,#13052);
#8178=LINE('',#58340,#13053);
#8179=LINE('',#58372,#13054);
#8180=LINE('',#58374,#13055);
#8181=LINE('',#58376,#13056);
#8182=LINE('',#58378,#13057);
#8183=LINE('',#58380,#13058);
#8184=LINE('',#58382,#13059);
#8185=LINE('',#58384,#13060);
#8186=LINE('',#58386,#13061);
#8187=LINE('',#58388,#13062);
#8188=LINE('',#58390,#13063);
#8189=LINE('',#58392,#13064);
#8190=LINE('',#58393,#13065);
#8191=LINE('',#58397,#13066);
#8192=LINE('',#58399,#13067);
#8193=LINE('',#58401,#13068);
#8194=LINE('',#58403,#13069);
#8195=LINE('',#58405,#13070);
#8196=LINE('',#58407,#13071);
#8197=LINE('',#58409,#13072);
#8198=LINE('',#58411,#13073);
#8199=LINE('',#58413,#13074);
#8200=LINE('',#58415,#13075);
#8201=LINE('',#58417,#13076);
#8202=LINE('',#58418,#13077);
#8203=LINE('',#58420,#13078);
#8204=LINE('',#58421,#13079);
#8205=LINE('',#58423,#13080);
#8206=LINE('',#58424,#13081);
#8207=LINE('',#58426,#13082);
#8208=LINE('',#58427,#13083);
#8209=LINE('',#58429,#13084);
#8210=LINE('',#58430,#13085);
#8211=LINE('',#58433,#13086);
#8212=LINE('',#58434,#13087);
#8213=LINE('',#58436,#13088);
#8214=LINE('',#58438,#13089);
#8215=LINE('',#58442,#13090);
#8216=LINE('',#58449,#13091);
#8217=LINE('',#58452,#13092);
#8218=LINE('',#58454,#13093);
#8219=LINE('',#58459,#13094);
#8220=LINE('',#58464,#13095);
#8221=LINE('',#58468,#13096);
#8222=LINE('',#58470,#13097);
#8223=LINE('',#58476,#13098);
#8224=LINE('',#58479,#13099);
#8225=LINE('',#58483,#13100);
#8226=LINE('',#58485,#13101);
#8227=LINE('',#58487,#13102);
#8228=LINE('',#58488,#13103);
#8229=LINE('',#58494,#13104);
#8230=LINE('',#58497,#13105);
#8231=LINE('',#58499,#13106);
#8232=LINE('',#58500,#13107);
#8233=LINE('',#58502,#13108);
#8234=LINE('',#58503,#13109);
#8235=LINE('',#58504,#13110);
#8236=LINE('',#58505,#13111);
#8237=LINE('',#58507,#13112);
#8238=LINE('',#58509,#13113);
#8239=LINE('',#58510,#13114);
#8240=LINE('',#58511,#13115);
#8241=LINE('',#58518,#13116);
#8242=LINE('',#58525,#13117);
#8243=LINE('',#58528,#13118);
#8244=LINE('',#58530,#13119);
#8245=LINE('',#58535,#13120);
#8246=LINE('',#58540,#13121);
#8247=LINE('',#58544,#13122);
#8248=LINE('',#58546,#13123);
#8249=LINE('',#58552,#13124);
#8250=LINE('',#58555,#13125);
#8251=LINE('',#58559,#13126);
#8252=LINE('',#58561,#13127);
#8253=LINE('',#58563,#13128);
#8254=LINE('',#58564,#13129);
#8255=LINE('',#58570,#13130);
#8256=LINE('',#58573,#13131);
#8257=LINE('',#58575,#13132);
#8258=LINE('',#58576,#13133);
#8259=LINE('',#58578,#13134);
#8260=LINE('',#58579,#13135);
#8261=LINE('',#58580,#13136);
#8262=LINE('',#58581,#13137);
#8263=LINE('',#58583,#13138);
#8264=LINE('',#58585,#13139);
#8265=LINE('',#58586,#13140);
#8266=LINE('',#58587,#13141);
#8267=LINE('',#58594,#13142);
#8268=LINE('',#58596,#13143);
#8269=LINE('',#58598,#13144);
#8270=LINE('',#58600,#13145);
#8271=LINE('',#58602,#13146);
#8272=LINE('',#58603,#13147);
#8273=LINE('',#58606,#13148);
#8274=LINE('',#58608,#13149);
#8275=LINE('',#58610,#13150);
#8276=LINE('',#58612,#13151);
#8277=LINE('',#58614,#13152);
#8278=LINE('',#58615,#13153);
#8279=LINE('',#58618,#13154);
#8280=LINE('',#58620,#13155);
#8281=LINE('',#58622,#13156);
#8282=LINE('',#58624,#13157);
#8283=LINE('',#58626,#13158);
#8284=LINE('',#58627,#13159);
#8285=LINE('',#58630,#13160);
#8286=LINE('',#58632,#13161);
#8287=LINE('',#58634,#13162);
#8288=LINE('',#58636,#13163);
#8289=LINE('',#58638,#13164);
#8290=LINE('',#58639,#13165);
#8291=LINE('',#58642,#13166);
#8292=LINE('',#58644,#13167);
#8293=LINE('',#58646,#13168);
#8294=LINE('',#58648,#13169);
#8295=LINE('',#58650,#13170);
#8296=LINE('',#58651,#13171);
#8297=LINE('',#58654,#13172);
#8298=LINE('',#58656,#13173);
#8299=LINE('',#58658,#13174);
#8300=LINE('',#58660,#13175);
#8301=LINE('',#58662,#13176);
#8302=LINE('',#58663,#13177);
#8303=LINE('',#58666,#13178);
#8304=LINE('',#58668,#13179);
#8305=LINE('',#58670,#13180);
#8306=LINE('',#58672,#13181);
#8307=LINE('',#58674,#13182);
#8308=LINE('',#58675,#13183);
#8309=LINE('',#58678,#13184);
#8310=LINE('',#58680,#13185);
#8311=LINE('',#58682,#13186);
#8312=LINE('',#58684,#13187);
#8313=LINE('',#58686,#13188);
#8314=LINE('',#58687,#13189);
#8315=LINE('',#58690,#13190);
#8316=LINE('',#58692,#13191);
#8317=LINE('',#58694,#13192);
#8318=LINE('',#58696,#13193);
#8319=LINE('',#58698,#13194);
#8320=LINE('',#58699,#13195);
#8321=LINE('',#58702,#13196);
#8322=LINE('',#58704,#13197);
#8323=LINE('',#58706,#13198);
#8324=LINE('',#58708,#13199);
#8325=LINE('',#58710,#13200);
#8326=LINE('',#58711,#13201);
#8327=LINE('',#58714,#13202);
#8328=LINE('',#58716,#13203);
#8329=LINE('',#58718,#13204);
#8330=LINE('',#58720,#13205);
#8331=LINE('',#58722,#13206);
#8332=LINE('',#58723,#13207);
#8333=LINE('',#58726,#13208);
#8334=LINE('',#58728,#13209);
#8335=LINE('',#58730,#13210);
#8336=LINE('',#58732,#13211);
#8337=LINE('',#58734,#13212);
#8338=LINE('',#58735,#13213);
#8339=LINE('',#58738,#13214);
#8340=LINE('',#58740,#13215);
#8341=LINE('',#58742,#13216);
#8342=LINE('',#58744,#13217);
#8343=LINE('',#58746,#13218);
#8344=LINE('',#58747,#13219);
#8345=LINE('',#58750,#13220);
#8346=LINE('',#58752,#13221);
#8347=LINE('',#58754,#13222);
#8348=LINE('',#58756,#13223);
#8349=LINE('',#58758,#13224);
#8350=LINE('',#58759,#13225);
#8351=LINE('',#58762,#13226);
#8352=LINE('',#58764,#13227);
#8353=LINE('',#58766,#13228);
#8354=LINE('',#58768,#13229);
#8355=LINE('',#58770,#13230);
#8356=LINE('',#58771,#13231);
#8357=LINE('',#58774,#13232);
#8358=LINE('',#58776,#13233);
#8359=LINE('',#58778,#13234);
#8360=LINE('',#58780,#13235);
#8361=LINE('',#58782,#13236);
#8362=LINE('',#58783,#13237);
#8363=LINE('',#58786,#13238);
#8364=LINE('',#58788,#13239);
#8365=LINE('',#58790,#13240);
#8366=LINE('',#58792,#13241);
#8367=LINE('',#58794,#13242);
#8368=LINE('',#58795,#13243);
#8369=LINE('',#58798,#13244);
#8370=LINE('',#58800,#13245);
#8371=LINE('',#58802,#13246);
#8372=LINE('',#58804,#13247);
#8373=LINE('',#58806,#13248);
#8374=LINE('',#58807,#13249);
#8375=LINE('',#58810,#13250);
#8376=LINE('',#58812,#13251);
#8377=LINE('',#58814,#13252);
#8378=LINE('',#58816,#13253);
#8379=LINE('',#58818,#13254);
#8380=LINE('',#58819,#13255);
#8381=LINE('',#58822,#13256);
#8382=LINE('',#58824,#13257);
#8383=LINE('',#58826,#13258);
#8384=LINE('',#58828,#13259);
#8385=LINE('',#58830,#13260);
#8386=LINE('',#58831,#13261);
#8387=LINE('',#58834,#13262);
#8388=LINE('',#58836,#13263);
#8389=LINE('',#58838,#13264);
#8390=LINE('',#58840,#13265);
#8391=LINE('',#58842,#13266);
#8392=LINE('',#58843,#13267);
#8393=LINE('',#58846,#13268);
#8394=LINE('',#58848,#13269);
#8395=LINE('',#58850,#13270);
#8396=LINE('',#58852,#13271);
#8397=LINE('',#58854,#13272);
#8398=LINE('',#58855,#13273);
#8399=LINE('',#58858,#13274);
#8400=LINE('',#58860,#13275);
#8401=LINE('',#58862,#13276);
#8402=LINE('',#58864,#13277);
#8403=LINE('',#58866,#13278);
#8404=LINE('',#58867,#13279);
#8405=LINE('',#58870,#13280);
#8406=LINE('',#58872,#13281);
#8407=LINE('',#58874,#13282);
#8408=LINE('',#58876,#13283);
#8409=LINE('',#58878,#13284);
#8410=LINE('',#58879,#13285);
#8411=LINE('',#58882,#13286);
#8412=LINE('',#58884,#13287);
#8413=LINE('',#58886,#13288);
#8414=LINE('',#58888,#13289);
#8415=LINE('',#58890,#13290);
#8416=LINE('',#58891,#13291);
#8417=LINE('',#58894,#13292);
#8418=LINE('',#58896,#13293);
#8419=LINE('',#58898,#13294);
#8420=LINE('',#58900,#13295);
#8421=LINE('',#58902,#13296);
#8422=LINE('',#58903,#13297);
#8423=LINE('',#58906,#13298);
#8424=LINE('',#58908,#13299);
#8425=LINE('',#58910,#13300);
#8426=LINE('',#58912,#13301);
#8427=LINE('',#58914,#13302);
#8428=LINE('',#58915,#13303);
#8429=LINE('',#58918,#13304);
#8430=LINE('',#58920,#13305);
#8431=LINE('',#58922,#13306);
#8432=LINE('',#58924,#13307);
#8433=LINE('',#58926,#13308);
#8434=LINE('',#58927,#13309);
#8435=LINE('',#58930,#13310);
#8436=LINE('',#58932,#13311);
#8437=LINE('',#58934,#13312);
#8438=LINE('',#58936,#13313);
#8439=LINE('',#58938,#13314);
#8440=LINE('',#58939,#13315);
#8441=LINE('',#58942,#13316);
#8442=LINE('',#58944,#13317);
#8443=LINE('',#58946,#13318);
#8444=LINE('',#58948,#13319);
#8445=LINE('',#58950,#13320);
#8446=LINE('',#58951,#13321);
#8447=LINE('',#58954,#13322);
#8448=LINE('',#58956,#13323);
#8449=LINE('',#58958,#13324);
#8450=LINE('',#58960,#13325);
#8451=LINE('',#58962,#13326);
#8452=LINE('',#58963,#13327);
#8453=LINE('',#58966,#13328);
#8454=LINE('',#58968,#13329);
#8455=LINE('',#58970,#13330);
#8456=LINE('',#58972,#13331);
#8457=LINE('',#58974,#13332);
#8458=LINE('',#58975,#13333);
#8459=LINE('',#58978,#13334);
#8460=LINE('',#58980,#13335);
#8461=LINE('',#58982,#13336);
#8462=LINE('',#58984,#13337);
#8463=LINE('',#58986,#13338);
#8464=LINE('',#58987,#13339);
#8465=LINE('',#58990,#13340);
#8466=LINE('',#58992,#13341);
#8467=LINE('',#58994,#13342);
#8468=LINE('',#58996,#13343);
#8469=LINE('',#58998,#13344);
#8470=LINE('',#58999,#13345);
#8471=LINE('',#59002,#13346);
#8472=LINE('',#59004,#13347);
#8473=LINE('',#59006,#13348);
#8474=LINE('',#59008,#13349);
#8475=LINE('',#59010,#13350);
#8476=LINE('',#59011,#13351);
#8477=LINE('',#59014,#13352);
#8478=LINE('',#59016,#13353);
#8479=LINE('',#59018,#13354);
#8480=LINE('',#59020,#13355);
#8481=LINE('',#59022,#13356);
#8482=LINE('',#59023,#13357);
#8483=LINE('',#59026,#13358);
#8484=LINE('',#59028,#13359);
#8485=LINE('',#59030,#13360);
#8486=LINE('',#59032,#13361);
#8487=LINE('',#59034,#13362);
#8488=LINE('',#59035,#13363);
#8489=LINE('',#59038,#13364);
#8490=LINE('',#59040,#13365);
#8491=LINE('',#59042,#13366);
#8492=LINE('',#59044,#13367);
#8493=LINE('',#59046,#13368);
#8494=LINE('',#59047,#13369);
#8495=LINE('',#59050,#13370);
#8496=LINE('',#59052,#13371);
#8497=LINE('',#59054,#13372);
#8498=LINE('',#59056,#13373);
#8499=LINE('',#59058,#13374);
#8500=LINE('',#59059,#13375);
#8501=LINE('',#59062,#13376);
#8502=LINE('',#59064,#13377);
#8503=LINE('',#59066,#13378);
#8504=LINE('',#59068,#13379);
#8505=LINE('',#59070,#13380);
#8506=LINE('',#59071,#13381);
#8507=LINE('',#59074,#13382);
#8508=LINE('',#59076,#13383);
#8509=LINE('',#59078,#13384);
#8510=LINE('',#59080,#13385);
#8511=LINE('',#59082,#13386);
#8512=LINE('',#59083,#13387);
#8513=LINE('',#59086,#13388);
#8514=LINE('',#59088,#13389);
#8515=LINE('',#59090,#13390);
#8516=LINE('',#59092,#13391);
#8517=LINE('',#59094,#13392);
#8518=LINE('',#59095,#13393);
#8519=LINE('',#59098,#13394);
#8520=LINE('',#59100,#13395);
#8521=LINE('',#59102,#13396);
#8522=LINE('',#59104,#13397);
#8523=LINE('',#59106,#13398);
#8524=LINE('',#59107,#13399);
#8525=LINE('',#59110,#13400);
#8526=LINE('',#59112,#13401);
#8527=LINE('',#59114,#13402);
#8528=LINE('',#59116,#13403);
#8529=LINE('',#59118,#13404);
#8530=LINE('',#59119,#13405);
#8531=LINE('',#59122,#13406);
#8532=LINE('',#59124,#13407);
#8533=LINE('',#59126,#13408);
#8534=LINE('',#59128,#13409);
#8535=LINE('',#59130,#13410);
#8536=LINE('',#59131,#13411);
#8537=LINE('',#59134,#13412);
#8538=LINE('',#59136,#13413);
#8539=LINE('',#59138,#13414);
#8540=LINE('',#59140,#13415);
#8541=LINE('',#59142,#13416);
#8542=LINE('',#59143,#13417);
#8543=LINE('',#59146,#13418);
#8544=LINE('',#59148,#13419);
#8545=LINE('',#59150,#13420);
#8546=LINE('',#59152,#13421);
#8547=LINE('',#59154,#13422);
#8548=LINE('',#59155,#13423);
#8549=LINE('',#59158,#13424);
#8550=LINE('',#59160,#13425);
#8551=LINE('',#59162,#13426);
#8552=LINE('',#59164,#13427);
#8553=LINE('',#59166,#13428);
#8554=LINE('',#59167,#13429);
#8555=LINE('',#59170,#13430);
#8556=LINE('',#59172,#13431);
#8557=LINE('',#59174,#13432);
#8558=LINE('',#59176,#13433);
#8559=LINE('',#59178,#13434);
#8560=LINE('',#59179,#13435);
#8561=LINE('',#59182,#13436);
#8562=LINE('',#59184,#13437);
#8563=LINE('',#59186,#13438);
#8564=LINE('',#59188,#13439);
#8565=LINE('',#59190,#13440);
#8566=LINE('',#59191,#13441);
#8567=LINE('',#59194,#13442);
#8568=LINE('',#59196,#13443);
#8569=LINE('',#59198,#13444);
#8570=LINE('',#59200,#13445);
#8571=LINE('',#59202,#13446);
#8572=LINE('',#59203,#13447);
#8573=LINE('',#59206,#13448);
#8574=LINE('',#59208,#13449);
#8575=LINE('',#59210,#13450);
#8576=LINE('',#59212,#13451);
#8577=LINE('',#59214,#13452);
#8578=LINE('',#59215,#13453);
#8579=LINE('',#59218,#13454);
#8580=LINE('',#59220,#13455);
#8581=LINE('',#59222,#13456);
#8582=LINE('',#59224,#13457);
#8583=LINE('',#59226,#13458);
#8584=LINE('',#59227,#13459);
#8585=LINE('',#59230,#13460);
#8586=LINE('',#59232,#13461);
#8587=LINE('',#59234,#13462);
#8588=LINE('',#59236,#13463);
#8589=LINE('',#59238,#13464);
#8590=LINE('',#59239,#13465);
#8591=LINE('',#59242,#13466);
#8592=LINE('',#59244,#13467);
#8593=LINE('',#59246,#13468);
#8594=LINE('',#59248,#13469);
#8595=LINE('',#59250,#13470);
#8596=LINE('',#59251,#13471);
#8597=LINE('',#59254,#13472);
#8598=LINE('',#59256,#13473);
#8599=LINE('',#59258,#13474);
#8600=LINE('',#59260,#13475);
#8601=LINE('',#59262,#13476);
#8602=LINE('',#59263,#13477);
#8603=LINE('',#59266,#13478);
#8604=LINE('',#59268,#13479);
#8605=LINE('',#59270,#13480);
#8606=LINE('',#59272,#13481);
#8607=LINE('',#59274,#13482);
#8608=LINE('',#59275,#13483);
#8609=LINE('',#59278,#13484);
#8610=LINE('',#59280,#13485);
#8611=LINE('',#59282,#13486);
#8612=LINE('',#59284,#13487);
#8613=LINE('',#59286,#13488);
#8614=LINE('',#59287,#13489);
#8615=LINE('',#59290,#13490);
#8616=LINE('',#59292,#13491);
#8617=LINE('',#59294,#13492);
#8618=LINE('',#59296,#13493);
#8619=LINE('',#59298,#13494);
#8620=LINE('',#59299,#13495);
#8621=LINE('',#59302,#13496);
#8622=LINE('',#59304,#13497);
#8623=LINE('',#59306,#13498);
#8624=LINE('',#59308,#13499);
#8625=LINE('',#59310,#13500);
#8626=LINE('',#59311,#13501);
#8627=LINE('',#59314,#13502);
#8628=LINE('',#59316,#13503);
#8629=LINE('',#59318,#13504);
#8630=LINE('',#59320,#13505);
#8631=LINE('',#59322,#13506);
#8632=LINE('',#59323,#13507);
#8633=LINE('',#59326,#13508);
#8634=LINE('',#59328,#13509);
#8635=LINE('',#59330,#13510);
#8636=LINE('',#59332,#13511);
#8637=LINE('',#59334,#13512);
#8638=LINE('',#59335,#13513);
#8639=LINE('',#59338,#13514);
#8640=LINE('',#59340,#13515);
#8641=LINE('',#59342,#13516);
#8642=LINE('',#59344,#13517);
#8643=LINE('',#59346,#13518);
#8644=LINE('',#59347,#13519);
#8645=LINE('',#59350,#13520);
#8646=LINE('',#59352,#13521);
#8647=LINE('',#59354,#13522);
#8648=LINE('',#59356,#13523);
#8649=LINE('',#59358,#13524);
#8650=LINE('',#59359,#13525);
#8651=LINE('',#59362,#13526);
#8652=LINE('',#59364,#13527);
#8653=LINE('',#59366,#13528);
#8654=LINE('',#59368,#13529);
#8655=LINE('',#59370,#13530);
#8656=LINE('',#59371,#13531);
#8657=LINE('',#59374,#13532);
#8658=LINE('',#59376,#13533);
#8659=LINE('',#59378,#13534);
#8660=LINE('',#59380,#13535);
#8661=LINE('',#59382,#13536);
#8662=LINE('',#59383,#13537);
#8663=LINE('',#59386,#13538);
#8664=LINE('',#59388,#13539);
#8665=LINE('',#59390,#13540);
#8666=LINE('',#59392,#13541);
#8667=LINE('',#59394,#13542);
#8668=LINE('',#59395,#13543);
#8669=LINE('',#59398,#13544);
#8670=LINE('',#59400,#13545);
#8671=LINE('',#59402,#13546);
#8672=LINE('',#59404,#13547);
#8673=LINE('',#59406,#13548);
#8674=LINE('',#59407,#13549);
#8675=LINE('',#59410,#13550);
#8676=LINE('',#59412,#13551);
#8677=LINE('',#59414,#13552);
#8678=LINE('',#59416,#13553);
#8679=LINE('',#59418,#13554);
#8680=LINE('',#59419,#13555);
#8681=LINE('',#59422,#13556);
#8682=LINE('',#59424,#13557);
#8683=LINE('',#59426,#13558);
#8684=LINE('',#59428,#13559);
#8685=LINE('',#59430,#13560);
#8686=LINE('',#59431,#13561);
#8687=LINE('',#59434,#13562);
#8688=LINE('',#59436,#13563);
#8689=LINE('',#59438,#13564);
#8690=LINE('',#59440,#13565);
#8691=LINE('',#59442,#13566);
#8692=LINE('',#59443,#13567);
#8693=LINE('',#59446,#13568);
#8694=LINE('',#59448,#13569);
#8695=LINE('',#59450,#13570);
#8696=LINE('',#59452,#13571);
#8697=LINE('',#59454,#13572);
#8698=LINE('',#59455,#13573);
#8699=LINE('',#59458,#13574);
#8700=LINE('',#59460,#13575);
#8701=LINE('',#59462,#13576);
#8702=LINE('',#59464,#13577);
#8703=LINE('',#59466,#13578);
#8704=LINE('',#59467,#13579);
#8705=LINE('',#59470,#13580);
#8706=LINE('',#59472,#13581);
#8707=LINE('',#59474,#13582);
#8708=LINE('',#59476,#13583);
#8709=LINE('',#59478,#13584);
#8710=LINE('',#59479,#13585);
#8711=LINE('',#59482,#13586);
#8712=LINE('',#59484,#13587);
#8713=LINE('',#59486,#13588);
#8714=LINE('',#59488,#13589);
#8715=LINE('',#59490,#13590);
#8716=LINE('',#59491,#13591);
#8717=LINE('',#59494,#13592);
#8718=LINE('',#59496,#13593);
#8719=LINE('',#59498,#13594);
#8720=LINE('',#59500,#13595);
#8721=LINE('',#59502,#13596);
#8722=LINE('',#59503,#13597);
#8723=LINE('',#59506,#13598);
#8724=LINE('',#59508,#13599);
#8725=LINE('',#59510,#13600);
#8726=LINE('',#59512,#13601);
#8727=LINE('',#59514,#13602);
#8728=LINE('',#59515,#13603);
#8729=LINE('',#59518,#13604);
#8730=LINE('',#59520,#13605);
#8731=LINE('',#59522,#13606);
#8732=LINE('',#59524,#13607);
#8733=LINE('',#59526,#13608);
#8734=LINE('',#59527,#13609);
#8735=LINE('',#59530,#13610);
#8736=LINE('',#59532,#13611);
#8737=LINE('',#59534,#13612);
#8738=LINE('',#59536,#13613);
#8739=LINE('',#59538,#13614);
#8740=LINE('',#59539,#13615);
#8741=LINE('',#59542,#13616);
#8742=LINE('',#59544,#13617);
#8743=LINE('',#59546,#13618);
#8744=LINE('',#59548,#13619);
#8745=LINE('',#59550,#13620);
#8746=LINE('',#59551,#13621);
#8747=LINE('',#59554,#13622);
#8748=LINE('',#59556,#13623);
#8749=LINE('',#59558,#13624);
#8750=LINE('',#59560,#13625);
#8751=LINE('',#59562,#13626);
#8752=LINE('',#59563,#13627);
#8753=LINE('',#59566,#13628);
#8754=LINE('',#59568,#13629);
#8755=LINE('',#59570,#13630);
#8756=LINE('',#59572,#13631);
#8757=LINE('',#59574,#13632);
#8758=LINE('',#59575,#13633);
#8759=LINE('',#59578,#13634);
#8760=LINE('',#59580,#13635);
#8761=LINE('',#59582,#13636);
#8762=LINE('',#59584,#13637);
#8763=LINE('',#59586,#13638);
#8764=LINE('',#59587,#13639);
#8765=LINE('',#59590,#13640);
#8766=LINE('',#59592,#13641);
#8767=LINE('',#59594,#13642);
#8768=LINE('',#59596,#13643);
#8769=LINE('',#59598,#13644);
#8770=LINE('',#59599,#13645);
#8771=LINE('',#59602,#13646);
#8772=LINE('',#59604,#13647);
#8773=LINE('',#59606,#13648);
#8774=LINE('',#59608,#13649);
#8775=LINE('',#59610,#13650);
#8776=LINE('',#59611,#13651);
#8777=LINE('',#59614,#13652);
#8778=LINE('',#59616,#13653);
#8779=LINE('',#59618,#13654);
#8780=LINE('',#59620,#13655);
#8781=LINE('',#59622,#13656);
#8782=LINE('',#59623,#13657);
#8783=LINE('',#59626,#13658);
#8784=LINE('',#59628,#13659);
#8785=LINE('',#59630,#13660);
#8786=LINE('',#59632,#13661);
#8787=LINE('',#59634,#13662);
#8788=LINE('',#59635,#13663);
#8789=LINE('',#59638,#13664);
#8790=LINE('',#59640,#13665);
#8791=LINE('',#59642,#13666);
#8792=LINE('',#59644,#13667);
#8793=LINE('',#59646,#13668);
#8794=LINE('',#59647,#13669);
#8795=LINE('',#59650,#13670);
#8796=LINE('',#59652,#13671);
#8797=LINE('',#59654,#13672);
#8798=LINE('',#59656,#13673);
#8799=LINE('',#59658,#13674);
#8800=LINE('',#59659,#13675);
#8801=LINE('',#59662,#13676);
#8802=LINE('',#59664,#13677);
#8803=LINE('',#59666,#13678);
#8804=LINE('',#59668,#13679);
#8805=LINE('',#59670,#13680);
#8806=LINE('',#59671,#13681);
#8807=LINE('',#59674,#13682);
#8808=LINE('',#59676,#13683);
#8809=LINE('',#59678,#13684);
#8810=LINE('',#59680,#13685);
#8811=LINE('',#59682,#13686);
#8812=LINE('',#59683,#13687);
#8813=LINE('',#59686,#13688);
#8814=LINE('',#59688,#13689);
#8815=LINE('',#59690,#13690);
#8816=LINE('',#59692,#13691);
#8817=LINE('',#59694,#13692);
#8818=LINE('',#59695,#13693);
#8819=LINE('',#59698,#13694);
#8820=LINE('',#59700,#13695);
#8821=LINE('',#59702,#13696);
#8822=LINE('',#59704,#13697);
#8823=LINE('',#59706,#13698);
#8824=LINE('',#59707,#13699);
#8825=LINE('',#59710,#13700);
#8826=LINE('',#59712,#13701);
#8827=LINE('',#59714,#13702);
#8828=LINE('',#59716,#13703);
#8829=LINE('',#59718,#13704);
#8830=LINE('',#59719,#13705);
#8831=LINE('',#59722,#13706);
#8832=LINE('',#59724,#13707);
#8833=LINE('',#59726,#13708);
#8834=LINE('',#59728,#13709);
#8835=LINE('',#59730,#13710);
#8836=LINE('',#59731,#13711);
#8837=LINE('',#59734,#13712);
#8838=LINE('',#59736,#13713);
#8839=LINE('',#59738,#13714);
#8840=LINE('',#59740,#13715);
#8841=LINE('',#59742,#13716);
#8842=LINE('',#59743,#13717);
#8843=LINE('',#59746,#13718);
#8844=LINE('',#59748,#13719);
#8845=LINE('',#59750,#13720);
#8846=LINE('',#59752,#13721);
#8847=LINE('',#59754,#13722);
#8848=LINE('',#59755,#13723);
#8849=LINE('',#59758,#13724);
#8850=LINE('',#59760,#13725);
#8851=LINE('',#59762,#13726);
#8852=LINE('',#59764,#13727);
#8853=LINE('',#59766,#13728);
#8854=LINE('',#59767,#13729);
#8855=LINE('',#59770,#13730);
#8856=LINE('',#59772,#13731);
#8857=LINE('',#59774,#13732);
#8858=LINE('',#59776,#13733);
#8859=LINE('',#59778,#13734);
#8860=LINE('',#59779,#13735);
#8861=LINE('',#59782,#13736);
#8862=LINE('',#59784,#13737);
#8863=LINE('',#59786,#13738);
#8864=LINE('',#59788,#13739);
#8865=LINE('',#59790,#13740);
#8866=LINE('',#59791,#13741);
#8867=LINE('',#59794,#13742);
#8868=LINE('',#59796,#13743);
#8869=LINE('',#59798,#13744);
#8870=LINE('',#59800,#13745);
#8871=LINE('',#59802,#13746);
#8872=LINE('',#59803,#13747);
#8873=LINE('',#59806,#13748);
#8874=LINE('',#59808,#13749);
#8875=LINE('',#59810,#13750);
#8876=LINE('',#59812,#13751);
#8877=LINE('',#59814,#13752);
#8878=LINE('',#59815,#13753);
#8879=LINE('',#59818,#13754);
#8880=LINE('',#59820,#13755);
#8881=LINE('',#59822,#13756);
#8882=LINE('',#59824,#13757);
#8883=LINE('',#59826,#13758);
#8884=LINE('',#59827,#13759);
#8885=LINE('',#59830,#13760);
#8886=LINE('',#59832,#13761);
#8887=LINE('',#59834,#13762);
#8888=LINE('',#59836,#13763);
#8889=LINE('',#59838,#13764);
#8890=LINE('',#59839,#13765);
#8891=LINE('',#59842,#13766);
#8892=LINE('',#59844,#13767);
#8893=LINE('',#59846,#13768);
#8894=LINE('',#59848,#13769);
#8895=LINE('',#59850,#13770);
#8896=LINE('',#59851,#13771);
#8897=LINE('',#59854,#13772);
#8898=LINE('',#59856,#13773);
#8899=LINE('',#59858,#13774);
#8900=LINE('',#59860,#13775);
#8901=LINE('',#59862,#13776);
#8902=LINE('',#59863,#13777);
#8903=LINE('',#59866,#13778);
#8904=LINE('',#59868,#13779);
#8905=LINE('',#59870,#13780);
#8906=LINE('',#59872,#13781);
#8907=LINE('',#59874,#13782);
#8908=LINE('',#59875,#13783);
#8909=LINE('',#59878,#13784);
#8910=LINE('',#59880,#13785);
#8911=LINE('',#59882,#13786);
#8912=LINE('',#59884,#13787);
#8913=LINE('',#59886,#13788);
#8914=LINE('',#59887,#13789);
#8915=LINE('',#59890,#13790);
#8916=LINE('',#59892,#13791);
#8917=LINE('',#59894,#13792);
#8918=LINE('',#59896,#13793);
#8919=LINE('',#59898,#13794);
#8920=LINE('',#59899,#13795);
#8921=LINE('',#59902,#13796);
#8922=LINE('',#59904,#13797);
#8923=LINE('',#59906,#13798);
#8924=LINE('',#59908,#13799);
#8925=LINE('',#59910,#13800);
#8926=LINE('',#59911,#13801);
#8927=LINE('',#59914,#13802);
#8928=LINE('',#59916,#13803);
#8929=LINE('',#59918,#13804);
#8930=LINE('',#59920,#13805);
#8931=LINE('',#59922,#13806);
#8932=LINE('',#59923,#13807);
#8933=LINE('',#59926,#13808);
#8934=LINE('',#59928,#13809);
#8935=LINE('',#59930,#13810);
#8936=LINE('',#59932,#13811);
#8937=LINE('',#59934,#13812);
#8938=LINE('',#59935,#13813);
#8939=LINE('',#59938,#13814);
#8940=LINE('',#59940,#13815);
#8941=LINE('',#59942,#13816);
#8942=LINE('',#59944,#13817);
#8943=LINE('',#59946,#13818);
#8944=LINE('',#59947,#13819);
#8945=LINE('',#59950,#13820);
#8946=LINE('',#59952,#13821);
#8947=LINE('',#59954,#13822);
#8948=LINE('',#59956,#13823);
#8949=LINE('',#59958,#13824);
#8950=LINE('',#59959,#13825);
#8951=LINE('',#59962,#13826);
#8952=LINE('',#59964,#13827);
#8953=LINE('',#59966,#13828);
#8954=LINE('',#59968,#13829);
#8955=LINE('',#59970,#13830);
#8956=LINE('',#59971,#13831);
#8957=LINE('',#59974,#13832);
#8958=LINE('',#59976,#13833);
#8959=LINE('',#59978,#13834);
#8960=LINE('',#59980,#13835);
#8961=LINE('',#59982,#13836);
#8962=LINE('',#59983,#13837);
#8963=LINE('',#59986,#13838);
#8964=LINE('',#59988,#13839);
#8965=LINE('',#59990,#13840);
#8966=LINE('',#59992,#13841);
#8967=LINE('',#59994,#13842);
#8968=LINE('',#59995,#13843);
#8969=LINE('',#59998,#13844);
#8970=LINE('',#60000,#13845);
#8971=LINE('',#60002,#13846);
#8972=LINE('',#60004,#13847);
#8973=LINE('',#60006,#13848);
#8974=LINE('',#60007,#13849);
#8975=LINE('',#60010,#13850);
#8976=LINE('',#60012,#13851);
#8977=LINE('',#60014,#13852);
#8978=LINE('',#60016,#13853);
#8979=LINE('',#60018,#13854);
#8980=LINE('',#60019,#13855);
#8981=LINE('',#60022,#13856);
#8982=LINE('',#60024,#13857);
#8983=LINE('',#60026,#13858);
#8984=LINE('',#60028,#13859);
#8985=LINE('',#60030,#13860);
#8986=LINE('',#60031,#13861);
#8987=LINE('',#60034,#13862);
#8988=LINE('',#60036,#13863);
#8989=LINE('',#60038,#13864);
#8990=LINE('',#60040,#13865);
#8991=LINE('',#60042,#13866);
#8992=LINE('',#60043,#13867);
#8993=LINE('',#60046,#13868);
#8994=LINE('',#60048,#13869);
#8995=LINE('',#60050,#13870);
#8996=LINE('',#60052,#13871);
#8997=LINE('',#60054,#13872);
#8998=LINE('',#60055,#13873);
#8999=LINE('',#60058,#13874);
#9000=LINE('',#60060,#13875);
#9001=LINE('',#60062,#13876);
#9002=LINE('',#60064,#13877);
#9003=LINE('',#60066,#13878);
#9004=LINE('',#60067,#13879);
#9005=LINE('',#60070,#13880);
#9006=LINE('',#60072,#13881);
#9007=LINE('',#60074,#13882);
#9008=LINE('',#60076,#13883);
#9009=LINE('',#60078,#13884);
#9010=LINE('',#60079,#13885);
#9011=LINE('',#60082,#13886);
#9012=LINE('',#60084,#13887);
#9013=LINE('',#60086,#13888);
#9014=LINE('',#60088,#13889);
#9015=LINE('',#60090,#13890);
#9016=LINE('',#60091,#13891);
#9017=LINE('',#60094,#13892);
#9018=LINE('',#60096,#13893);
#9019=LINE('',#60098,#13894);
#9020=LINE('',#60100,#13895);
#9021=LINE('',#60102,#13896);
#9022=LINE('',#60103,#13897);
#9023=LINE('',#60106,#13898);
#9024=LINE('',#60108,#13899);
#9025=LINE('',#60110,#13900);
#9026=LINE('',#60112,#13901);
#9027=LINE('',#60114,#13902);
#9028=LINE('',#60115,#13903);
#9029=LINE('',#60118,#13904);
#9030=LINE('',#60120,#13905);
#9031=LINE('',#60122,#13906);
#9032=LINE('',#60124,#13907);
#9033=LINE('',#60126,#13908);
#9034=LINE('',#60127,#13909);
#9035=LINE('',#60130,#13910);
#9036=LINE('',#60132,#13911);
#9037=LINE('',#60134,#13912);
#9038=LINE('',#60136,#13913);
#9039=LINE('',#60138,#13914);
#9040=LINE('',#60139,#13915);
#9041=LINE('',#60142,#13916);
#9042=LINE('',#60144,#13917);
#9043=LINE('',#60146,#13918);
#9044=LINE('',#60148,#13919);
#9045=LINE('',#60150,#13920);
#9046=LINE('',#60151,#13921);
#9047=LINE('',#60154,#13922);
#9048=LINE('',#60156,#13923);
#9049=LINE('',#60158,#13924);
#9050=LINE('',#60160,#13925);
#9051=LINE('',#60162,#13926);
#9052=LINE('',#60163,#13927);
#9053=LINE('',#60166,#13928);
#9054=LINE('',#60168,#13929);
#9055=LINE('',#60170,#13930);
#9056=LINE('',#60172,#13931);
#9057=LINE('',#60174,#13932);
#9058=LINE('',#60175,#13933);
#9059=LINE('',#60178,#13934);
#9060=LINE('',#60180,#13935);
#9061=LINE('',#60182,#13936);
#9062=LINE('',#60184,#13937);
#9063=LINE('',#60186,#13938);
#9064=LINE('',#60187,#13939);
#9065=LINE('',#60190,#13940);
#9066=LINE('',#60192,#13941);
#9067=LINE('',#60194,#13942);
#9068=LINE('',#60196,#13943);
#9069=LINE('',#60198,#13944);
#9070=LINE('',#60199,#13945);
#9071=LINE('',#60202,#13946);
#9072=LINE('',#60204,#13947);
#9073=LINE('',#60206,#13948);
#9074=LINE('',#60208,#13949);
#9075=LINE('',#60210,#13950);
#9076=LINE('',#60211,#13951);
#9077=LINE('',#60214,#13952);
#9078=LINE('',#60216,#13953);
#9079=LINE('',#60218,#13954);
#9080=LINE('',#60220,#13955);
#9081=LINE('',#60222,#13956);
#9082=LINE('',#60223,#13957);
#9083=LINE('',#60226,#13958);
#9084=LINE('',#60228,#13959);
#9085=LINE('',#60230,#13960);
#9086=LINE('',#60232,#13961);
#9087=LINE('',#60234,#13962);
#9088=LINE('',#60235,#13963);
#9089=LINE('',#60238,#13964);
#9090=LINE('',#60240,#13965);
#9091=LINE('',#60242,#13966);
#9092=LINE('',#60244,#13967);
#9093=LINE('',#60246,#13968);
#9094=LINE('',#60247,#13969);
#9095=LINE('',#60250,#13970);
#9096=LINE('',#60252,#13971);
#9097=LINE('',#60254,#13972);
#9098=LINE('',#60256,#13973);
#9099=LINE('',#60258,#13974);
#9100=LINE('',#60259,#13975);
#9101=LINE('',#60262,#13976);
#9102=LINE('',#60264,#13977);
#9103=LINE('',#60266,#13978);
#9104=LINE('',#60268,#13979);
#9105=LINE('',#60270,#13980);
#9106=LINE('',#60271,#13981);
#9107=LINE('',#60274,#13982);
#9108=LINE('',#60276,#13983);
#9109=LINE('',#60278,#13984);
#9110=LINE('',#60280,#13985);
#9111=LINE('',#60282,#13986);
#9112=LINE('',#60283,#13987);
#9113=LINE('',#60286,#13988);
#9114=LINE('',#60288,#13989);
#9115=LINE('',#60290,#13990);
#9116=LINE('',#60292,#13991);
#9117=LINE('',#60294,#13992);
#9118=LINE('',#60295,#13993);
#9119=LINE('',#60298,#13994);
#9120=LINE('',#60300,#13995);
#9121=LINE('',#60302,#13996);
#9122=LINE('',#60304,#13997);
#9123=LINE('',#60306,#13998);
#9124=LINE('',#60307,#13999);
#9125=LINE('',#60310,#14000);
#9126=LINE('',#60312,#14001);
#9127=LINE('',#60314,#14002);
#9128=LINE('',#60316,#14003);
#9129=LINE('',#60318,#14004);
#9130=LINE('',#60319,#14005);
#9131=LINE('',#60322,#14006);
#9132=LINE('',#60324,#14007);
#9133=LINE('',#60326,#14008);
#9134=LINE('',#60328,#14009);
#9135=LINE('',#60330,#14010);
#9136=LINE('',#60331,#14011);
#9137=LINE('',#60334,#14012);
#9138=LINE('',#60336,#14013);
#9139=LINE('',#60338,#14014);
#9140=LINE('',#60340,#14015);
#9141=LINE('',#60342,#14016);
#9142=LINE('',#60343,#14017);
#9143=LINE('',#60346,#14018);
#9144=LINE('',#60348,#14019);
#9145=LINE('',#60350,#14020);
#9146=LINE('',#60352,#14021);
#9147=LINE('',#60354,#14022);
#9148=LINE('',#60355,#14023);
#9149=LINE('',#60358,#14024);
#9150=LINE('',#60360,#14025);
#9151=LINE('',#60362,#14026);
#9152=LINE('',#60364,#14027);
#9153=LINE('',#60366,#14028);
#9154=LINE('',#60367,#14029);
#9155=LINE('',#60370,#14030);
#9156=LINE('',#60372,#14031);
#9157=LINE('',#60374,#14032);
#9158=LINE('',#60376,#14033);
#9159=LINE('',#60378,#14034);
#9160=LINE('',#60379,#14035);
#9161=LINE('',#60382,#14036);
#9162=LINE('',#60384,#14037);
#9163=LINE('',#60386,#14038);
#9164=LINE('',#60388,#14039);
#9165=LINE('',#60390,#14040);
#9166=LINE('',#60391,#14041);
#9167=LINE('',#60394,#14042);
#9168=LINE('',#60396,#14043);
#9169=LINE('',#60398,#14044);
#9170=LINE('',#60400,#14045);
#9171=LINE('',#60402,#14046);
#9172=LINE('',#60403,#14047);
#9173=LINE('',#60406,#14048);
#9174=LINE('',#60408,#14049);
#9175=LINE('',#60410,#14050);
#9176=LINE('',#60412,#14051);
#9177=LINE('',#60414,#14052);
#9178=LINE('',#60415,#14053);
#9179=LINE('',#60418,#14054);
#9180=LINE('',#60420,#14055);
#9181=LINE('',#60422,#14056);
#9182=LINE('',#60424,#14057);
#9183=LINE('',#60426,#14058);
#9184=LINE('',#60427,#14059);
#9185=LINE('',#60430,#14060);
#9186=LINE('',#60432,#14061);
#9187=LINE('',#60434,#14062);
#9188=LINE('',#60436,#14063);
#9189=LINE('',#60438,#14064);
#9190=LINE('',#60439,#14065);
#9191=LINE('',#60442,#14066);
#9192=LINE('',#60444,#14067);
#9193=LINE('',#60446,#14068);
#9194=LINE('',#60448,#14069);
#9195=LINE('',#60450,#14070);
#9196=LINE('',#60451,#14071);
#9197=LINE('',#60454,#14072);
#9198=LINE('',#60456,#14073);
#9199=LINE('',#60458,#14074);
#9200=LINE('',#60460,#14075);
#9201=LINE('',#60462,#14076);
#9202=LINE('',#60463,#14077);
#9203=LINE('',#60466,#14078);
#9204=LINE('',#60468,#14079);
#9205=LINE('',#60470,#14080);
#9206=LINE('',#60472,#14081);
#9207=LINE('',#60474,#14082);
#9208=LINE('',#60475,#14083);
#9209=LINE('',#60478,#14084);
#9210=LINE('',#60480,#14085);
#9211=LINE('',#60482,#14086);
#9212=LINE('',#60484,#14087);
#9213=LINE('',#60486,#14088);
#9214=LINE('',#60487,#14089);
#9215=LINE('',#60490,#14090);
#9216=LINE('',#60492,#14091);
#9217=LINE('',#60494,#14092);
#9218=LINE('',#60496,#14093);
#9219=LINE('',#60498,#14094);
#9220=LINE('',#60499,#14095);
#9221=LINE('',#60502,#14096);
#9222=LINE('',#60504,#14097);
#9223=LINE('',#60506,#14098);
#9224=LINE('',#60508,#14099);
#9225=LINE('',#60510,#14100);
#9226=LINE('',#60511,#14101);
#9227=LINE('',#60514,#14102);
#9228=LINE('',#60516,#14103);
#9229=LINE('',#60518,#14104);
#9230=LINE('',#60520,#14105);
#9231=LINE('',#60522,#14106);
#9232=LINE('',#60523,#14107);
#9233=LINE('',#60526,#14108);
#9234=LINE('',#60528,#14109);
#9235=LINE('',#60530,#14110);
#9236=LINE('',#60532,#14111);
#9237=LINE('',#60534,#14112);
#9238=LINE('',#60535,#14113);
#9239=LINE('',#60538,#14114);
#9240=LINE('',#60540,#14115);
#9241=LINE('',#60542,#14116);
#9242=LINE('',#60544,#14117);
#9243=LINE('',#60546,#14118);
#9244=LINE('',#60547,#14119);
#9245=LINE('',#60550,#14120);
#9246=LINE('',#60552,#14121);
#9247=LINE('',#60554,#14122);
#9248=LINE('',#60556,#14123);
#9249=LINE('',#60558,#14124);
#9250=LINE('',#60559,#14125);
#9251=LINE('',#60562,#14126);
#9252=LINE('',#60564,#14127);
#9253=LINE('',#60566,#14128);
#9254=LINE('',#60568,#14129);
#9255=LINE('',#60570,#14130);
#9256=LINE('',#60571,#14131);
#9257=LINE('',#60574,#14132);
#9258=LINE('',#60576,#14133);
#9259=LINE('',#60578,#14134);
#9260=LINE('',#60580,#14135);
#9261=LINE('',#60582,#14136);
#9262=LINE('',#60583,#14137);
#9263=LINE('',#60586,#14138);
#9264=LINE('',#60588,#14139);
#9265=LINE('',#60590,#14140);
#9266=LINE('',#60592,#14141);
#9267=LINE('',#60594,#14142);
#9268=LINE('',#60595,#14143);
#9269=LINE('',#60598,#14144);
#9270=LINE('',#60600,#14145);
#9271=LINE('',#60602,#14146);
#9272=LINE('',#60604,#14147);
#9273=LINE('',#60606,#14148);
#9274=LINE('',#60607,#14149);
#9275=LINE('',#60610,#14150);
#9276=LINE('',#60612,#14151);
#9277=LINE('',#60614,#14152);
#9278=LINE('',#60616,#14153);
#9279=LINE('',#60618,#14154);
#9280=LINE('',#60619,#14155);
#9281=LINE('',#60622,#14156);
#9282=LINE('',#60624,#14157);
#9283=LINE('',#60626,#14158);
#9284=LINE('',#60628,#14159);
#9285=LINE('',#60630,#14160);
#9286=LINE('',#60631,#14161);
#9287=LINE('',#60634,#14162);
#9288=LINE('',#60636,#14163);
#9289=LINE('',#60638,#14164);
#9290=LINE('',#60640,#14165);
#9291=LINE('',#60642,#14166);
#9292=LINE('',#60643,#14167);
#9293=LINE('',#60646,#14168);
#9294=LINE('',#60648,#14169);
#9295=LINE('',#60650,#14170);
#9296=LINE('',#60652,#14171);
#9297=LINE('',#60654,#14172);
#9298=LINE('',#60655,#14173);
#9299=LINE('',#60658,#14174);
#9300=LINE('',#60660,#14175);
#9301=LINE('',#60662,#14176);
#9302=LINE('',#60664,#14177);
#9303=LINE('',#60666,#14178);
#9304=LINE('',#60667,#14179);
#9305=LINE('',#60670,#14180);
#9306=LINE('',#60672,#14181);
#9307=LINE('',#60674,#14182);
#9308=LINE('',#60676,#14183);
#9309=LINE('',#60678,#14184);
#9310=LINE('',#60679,#14185);
#9311=LINE('',#60682,#14186);
#9312=LINE('',#60684,#14187);
#9313=LINE('',#60686,#14188);
#9314=LINE('',#60688,#14189);
#9315=LINE('',#60690,#14190);
#9316=LINE('',#60691,#14191);
#9317=LINE('',#60694,#14192);
#9318=LINE('',#60696,#14193);
#9319=LINE('',#60698,#14194);
#9320=LINE('',#60700,#14195);
#9321=LINE('',#60702,#14196);
#9322=LINE('',#60703,#14197);
#9323=LINE('',#60706,#14198);
#9324=LINE('',#60708,#14199);
#9325=LINE('',#60710,#14200);
#9326=LINE('',#60712,#14201);
#9327=LINE('',#60714,#14202);
#9328=LINE('',#60715,#14203);
#9329=LINE('',#60718,#14204);
#9330=LINE('',#60720,#14205);
#9331=LINE('',#60722,#14206);
#9332=LINE('',#60724,#14207);
#9333=LINE('',#60726,#14208);
#9334=LINE('',#60727,#14209);
#9335=LINE('',#60730,#14210);
#9336=LINE('',#60732,#14211);
#9337=LINE('',#60734,#14212);
#9338=LINE('',#60736,#14213);
#9339=LINE('',#60738,#14214);
#9340=LINE('',#60739,#14215);
#9341=LINE('',#60742,#14216);
#9342=LINE('',#60744,#14217);
#9343=LINE('',#60746,#14218);
#9344=LINE('',#60748,#14219);
#9345=LINE('',#60750,#14220);
#9346=LINE('',#60751,#14221);
#9347=LINE('',#60754,#14222);
#9348=LINE('',#60756,#14223);
#9349=LINE('',#60758,#14224);
#9350=LINE('',#60760,#14225);
#9351=LINE('',#60762,#14226);
#9352=LINE('',#60763,#14227);
#9353=LINE('',#60766,#14228);
#9354=LINE('',#60768,#14229);
#9355=LINE('',#60770,#14230);
#9356=LINE('',#60772,#14231);
#9357=LINE('',#60774,#14232);
#9358=LINE('',#60775,#14233);
#9359=LINE('',#60778,#14234);
#9360=LINE('',#60780,#14235);
#9361=LINE('',#60782,#14236);
#9362=LINE('',#60784,#14237);
#9363=LINE('',#60786,#14238);
#9364=LINE('',#60787,#14239);
#9365=LINE('',#60790,#14240);
#9366=LINE('',#60792,#14241);
#9367=LINE('',#60794,#14242);
#9368=LINE('',#60796,#14243);
#9369=LINE('',#60798,#14244);
#9370=LINE('',#60799,#14245);
#9371=LINE('',#60802,#14246);
#9372=LINE('',#60804,#14247);
#9373=LINE('',#60806,#14248);
#9374=LINE('',#60808,#14249);
#9375=LINE('',#60810,#14250);
#9376=LINE('',#60811,#14251);
#9377=LINE('',#60814,#14252);
#9378=LINE('',#60816,#14253);
#9379=LINE('',#60818,#14254);
#9380=LINE('',#60820,#14255);
#9381=LINE('',#60822,#14256);
#9382=LINE('',#60823,#14257);
#9383=LINE('',#60827,#14258);
#9384=LINE('',#60829,#14259);
#9385=LINE('',#60831,#14260);
#9386=LINE('',#60833,#14261);
#9387=LINE('',#60835,#14262);
#9388=LINE('',#60836,#14263);
#9389=LINE('',#60839,#14264);
#9390=LINE('',#60841,#14265);
#9391=LINE('',#60843,#14266);
#9392=LINE('',#60845,#14267);
#9393=LINE('',#60847,#14268);
#9394=LINE('',#60848,#14269);
#9395=LINE('',#60851,#14270);
#9396=LINE('',#60853,#14271);
#9397=LINE('',#60855,#14272);
#9398=LINE('',#60857,#14273);
#9399=LINE('',#60859,#14274);
#9400=LINE('',#60860,#14275);
#9401=LINE('',#60863,#14276);
#9402=LINE('',#60865,#14277);
#9403=LINE('',#60867,#14278);
#9404=LINE('',#60869,#14279);
#9405=LINE('',#60871,#14280);
#9406=LINE('',#60872,#14281);
#9407=LINE('',#60875,#14282);
#9408=LINE('',#60877,#14283);
#9409=LINE('',#60879,#14284);
#9410=LINE('',#60881,#14285);
#9411=LINE('',#60883,#14286);
#9412=LINE('',#60884,#14287);
#9413=LINE('',#60887,#14288);
#9414=LINE('',#60889,#14289);
#9415=LINE('',#60891,#14290);
#9416=LINE('',#60893,#14291);
#9417=LINE('',#60895,#14292);
#9418=LINE('',#60896,#14293);
#9419=LINE('',#60899,#14294);
#9420=LINE('',#60901,#14295);
#9421=LINE('',#60903,#14296);
#9422=LINE('',#60905,#14297);
#9423=LINE('',#60907,#14298);
#9424=LINE('',#60908,#14299);
#9425=LINE('',#60911,#14300);
#9426=LINE('',#60913,#14301);
#9427=LINE('',#60915,#14302);
#9428=LINE('',#60917,#14303);
#9429=LINE('',#60919,#14304);
#9430=LINE('',#60920,#14305);
#9431=LINE('',#60923,#14306);
#9432=LINE('',#60925,#14307);
#9433=LINE('',#60927,#14308);
#9434=LINE('',#60929,#14309);
#9435=LINE('',#60931,#14310);
#9436=LINE('',#60932,#14311);
#9437=LINE('',#60935,#14312);
#9438=LINE('',#60937,#14313);
#9439=LINE('',#60939,#14314);
#9440=LINE('',#60941,#14315);
#9441=LINE('',#60943,#14316);
#9442=LINE('',#60944,#14317);
#9443=LINE('',#60947,#14318);
#9444=LINE('',#60949,#14319);
#9445=LINE('',#60951,#14320);
#9446=LINE('',#60953,#14321);
#9447=LINE('',#60955,#14322);
#9448=LINE('',#60956,#14323);
#9449=LINE('',#60959,#14324);
#9450=LINE('',#60961,#14325);
#9451=LINE('',#60963,#14326);
#9452=LINE('',#60965,#14327);
#9453=LINE('',#60967,#14328);
#9454=LINE('',#60968,#14329);
#9455=LINE('',#60971,#14330);
#9456=LINE('',#60973,#14331);
#9457=LINE('',#60975,#14332);
#9458=LINE('',#60977,#14333);
#9459=LINE('',#60979,#14334);
#9460=LINE('',#60980,#14335);
#9461=LINE('',#60983,#14336);
#9462=LINE('',#60985,#14337);
#9463=LINE('',#60987,#14338);
#9464=LINE('',#60989,#14339);
#9465=LINE('',#60991,#14340);
#9466=LINE('',#60992,#14341);
#9467=LINE('',#60995,#14342);
#9468=LINE('',#60997,#14343);
#9469=LINE('',#60999,#14344);
#9470=LINE('',#61001,#14345);
#9471=LINE('',#61003,#14346);
#9472=LINE('',#61004,#14347);
#9473=LINE('',#61007,#14348);
#9474=LINE('',#61009,#14349);
#9475=LINE('',#61011,#14350);
#9476=LINE('',#61013,#14351);
#9477=LINE('',#61015,#14352);
#9478=LINE('',#61016,#14353);
#9479=LINE('',#61019,#14354);
#9480=LINE('',#61021,#14355);
#9481=LINE('',#61023,#14356);
#9482=LINE('',#61025,#14357);
#9483=LINE('',#61027,#14358);
#9484=LINE('',#61028,#14359);
#9485=LINE('',#61031,#14360);
#9486=LINE('',#61033,#14361);
#9487=LINE('',#61035,#14362);
#9488=LINE('',#61037,#14363);
#9489=LINE('',#61039,#14364);
#9490=LINE('',#61040,#14365);
#9491=LINE('',#61043,#14366);
#9492=LINE('',#61045,#14367);
#9493=LINE('',#61047,#14368);
#9494=LINE('',#61049,#14369);
#9495=LINE('',#61051,#14370);
#9496=LINE('',#61052,#14371);
#9497=LINE('',#61055,#14372);
#9498=LINE('',#61057,#14373);
#9499=LINE('',#61059,#14374);
#9500=LINE('',#61061,#14375);
#9501=LINE('',#61063,#14376);
#9502=LINE('',#61064,#14377);
#9503=LINE('',#61067,#14378);
#9504=LINE('',#61069,#14379);
#9505=LINE('',#61071,#14380);
#9506=LINE('',#61073,#14381);
#9507=LINE('',#61075,#14382);
#9508=LINE('',#61076,#14383);
#9509=LINE('',#61079,#14384);
#9510=LINE('',#61081,#14385);
#9511=LINE('',#61083,#14386);
#9512=LINE('',#61085,#14387);
#9513=LINE('',#61087,#14388);
#9514=LINE('',#61088,#14389);
#9515=LINE('',#61091,#14390);
#9516=LINE('',#61093,#14391);
#9517=LINE('',#61095,#14392);
#9518=LINE('',#61097,#14393);
#9519=LINE('',#61099,#14394);
#9520=LINE('',#61100,#14395);
#9521=LINE('',#61103,#14396);
#9522=LINE('',#61105,#14397);
#9523=LINE('',#61107,#14398);
#9524=LINE('',#61109,#14399);
#9525=LINE('',#61111,#14400);
#9526=LINE('',#61112,#14401);
#9527=LINE('',#61115,#14402);
#9528=LINE('',#61117,#14403);
#9529=LINE('',#61119,#14404);
#9530=LINE('',#61121,#14405);
#9531=LINE('',#61123,#14406);
#9532=LINE('',#61124,#14407);
#9533=LINE('',#61127,#14408);
#9534=LINE('',#61129,#14409);
#9535=LINE('',#61131,#14410);
#9536=LINE('',#61133,#14411);
#9537=LINE('',#61135,#14412);
#9538=LINE('',#61136,#14413);
#9539=LINE('',#61139,#14414);
#9540=LINE('',#61141,#14415);
#9541=LINE('',#61143,#14416);
#9542=LINE('',#61145,#14417);
#9543=LINE('',#61147,#14418);
#9544=LINE('',#61148,#14419);
#9545=LINE('',#61151,#14420);
#9546=LINE('',#61153,#14421);
#9547=LINE('',#61155,#14422);
#9548=LINE('',#61157,#14423);
#9549=LINE('',#61159,#14424);
#9550=LINE('',#61160,#14425);
#9551=LINE('',#61163,#14426);
#9552=LINE('',#61165,#14427);
#9553=LINE('',#61167,#14428);
#9554=LINE('',#61169,#14429);
#9555=LINE('',#61171,#14430);
#9556=LINE('',#61172,#14431);
#9557=LINE('',#61175,#14432);
#9558=LINE('',#61177,#14433);
#9559=LINE('',#61179,#14434);
#9560=LINE('',#61181,#14435);
#9561=LINE('',#61183,#14436);
#9562=LINE('',#61184,#14437);
#9563=LINE('',#61187,#14438);
#9564=LINE('',#61189,#14439);
#9565=LINE('',#61191,#14440);
#9566=LINE('',#61193,#14441);
#9567=LINE('',#61195,#14442);
#9568=LINE('',#61196,#14443);
#9569=LINE('',#61199,#14444);
#9570=LINE('',#61201,#14445);
#9571=LINE('',#61203,#14446);
#9572=LINE('',#61205,#14447);
#9573=LINE('',#61207,#14448);
#9574=LINE('',#61208,#14449);
#9575=LINE('',#61211,#14450);
#9576=LINE('',#61213,#14451);
#9577=LINE('',#61215,#14452);
#9578=LINE('',#61217,#14453);
#9579=LINE('',#61219,#14454);
#9580=LINE('',#61220,#14455);
#9581=LINE('',#61223,#14456);
#9582=LINE('',#61225,#14457);
#9583=LINE('',#61227,#14458);
#9584=LINE('',#61229,#14459);
#9585=LINE('',#61231,#14460);
#9586=LINE('',#61232,#14461);
#9587=LINE('',#61235,#14462);
#9588=LINE('',#61237,#14463);
#9589=LINE('',#61239,#14464);
#9590=LINE('',#61241,#14465);
#9591=LINE('',#61243,#14466);
#9592=LINE('',#61244,#14467);
#9593=LINE('',#61247,#14468);
#9594=LINE('',#61249,#14469);
#9595=LINE('',#61251,#14470);
#9596=LINE('',#61253,#14471);
#9597=LINE('',#61255,#14472);
#9598=LINE('',#61256,#14473);
#9599=LINE('',#61259,#14474);
#9600=LINE('',#61261,#14475);
#9601=LINE('',#61263,#14476);
#9602=LINE('',#61265,#14477);
#9603=LINE('',#61267,#14478);
#9604=LINE('',#61268,#14479);
#9605=LINE('',#61271,#14480);
#9606=LINE('',#61273,#14481);
#9607=LINE('',#61275,#14482);
#9608=LINE('',#61277,#14483);
#9609=LINE('',#61279,#14484);
#9610=LINE('',#61280,#14485);
#9611=LINE('',#61283,#14486);
#9612=LINE('',#61285,#14487);
#9613=LINE('',#61287,#14488);
#9614=LINE('',#61289,#14489);
#9615=LINE('',#61291,#14490);
#9616=LINE('',#61292,#14491);
#9617=LINE('',#61295,#14492);
#9618=LINE('',#61297,#14493);
#9619=LINE('',#61299,#14494);
#9620=LINE('',#61301,#14495);
#9621=LINE('',#61303,#14496);
#9622=LINE('',#61304,#14497);
#9623=LINE('',#61307,#14498);
#9624=LINE('',#61309,#14499);
#9625=LINE('',#61311,#14500);
#9626=LINE('',#61313,#14501);
#9627=LINE('',#61315,#14502);
#9628=LINE('',#61316,#14503);
#9629=LINE('',#61319,#14504);
#9630=LINE('',#61321,#14505);
#9631=LINE('',#61323,#14506);
#9632=LINE('',#61325,#14507);
#9633=LINE('',#61327,#14508);
#9634=LINE('',#61328,#14509);
#9635=LINE('',#61331,#14510);
#9636=LINE('',#61333,#14511);
#9637=LINE('',#61335,#14512);
#9638=LINE('',#61337,#14513);
#9639=LINE('',#61339,#14514);
#9640=LINE('',#61340,#14515);
#9641=LINE('',#61343,#14516);
#9642=LINE('',#61345,#14517);
#9643=LINE('',#61347,#14518);
#9644=LINE('',#61349,#14519);
#9645=LINE('',#61351,#14520);
#9646=LINE('',#61352,#14521);
#9647=LINE('',#61355,#14522);
#9648=LINE('',#61357,#14523);
#9649=LINE('',#61359,#14524);
#9650=LINE('',#61361,#14525);
#9651=LINE('',#61363,#14526);
#9652=LINE('',#61364,#14527);
#9653=LINE('',#61367,#14528);
#9654=LINE('',#61369,#14529);
#9655=LINE('',#61371,#14530);
#9656=LINE('',#61373,#14531);
#9657=LINE('',#61375,#14532);
#9658=LINE('',#61376,#14533);
#9659=LINE('',#61379,#14534);
#9660=LINE('',#61381,#14535);
#9661=LINE('',#61383,#14536);
#9662=LINE('',#61385,#14537);
#9663=LINE('',#61387,#14538);
#9664=LINE('',#61388,#14539);
#9665=LINE('',#61391,#14540);
#9666=LINE('',#61393,#14541);
#9667=LINE('',#61395,#14542);
#9668=LINE('',#61397,#14543);
#9669=LINE('',#61399,#14544);
#9670=LINE('',#61400,#14545);
#9671=LINE('',#61403,#14546);
#9672=LINE('',#61405,#14547);
#9673=LINE('',#61407,#14548);
#9674=LINE('',#61409,#14549);
#9675=LINE('',#61411,#14550);
#9676=LINE('',#61412,#14551);
#9677=LINE('',#61415,#14552);
#9678=LINE('',#61417,#14553);
#9679=LINE('',#61419,#14554);
#9680=LINE('',#61421,#14555);
#9681=LINE('',#61423,#14556);
#9682=LINE('',#61424,#14557);
#9683=LINE('',#61427,#14558);
#9684=LINE('',#61429,#14559);
#9685=LINE('',#61431,#14560);
#9686=LINE('',#61433,#14561);
#9687=LINE('',#61435,#14562);
#9688=LINE('',#61436,#14563);
#9689=LINE('',#61439,#14564);
#9690=LINE('',#61441,#14565);
#9691=LINE('',#61443,#14566);
#9692=LINE('',#61445,#14567);
#9693=LINE('',#61447,#14568);
#9694=LINE('',#61448,#14569);
#9695=LINE('',#61451,#14570);
#9696=LINE('',#61453,#14571);
#9697=LINE('',#61455,#14572);
#9698=LINE('',#61457,#14573);
#9699=LINE('',#61459,#14574);
#9700=LINE('',#61460,#14575);
#9701=LINE('',#61463,#14576);
#9702=LINE('',#61465,#14577);
#9703=LINE('',#61467,#14578);
#9704=LINE('',#61469,#14579);
#9705=LINE('',#61471,#14580);
#9706=LINE('',#61472,#14581);
#9707=LINE('',#61475,#14582);
#9708=LINE('',#61477,#14583);
#9709=LINE('',#61479,#14584);
#9710=LINE('',#61481,#14585);
#9711=LINE('',#61483,#14586);
#9712=LINE('',#61484,#14587);
#9713=LINE('',#61487,#14588);
#9714=LINE('',#61489,#14589);
#9715=LINE('',#61491,#14590);
#9716=LINE('',#61493,#14591);
#9717=LINE('',#61495,#14592);
#9718=LINE('',#61496,#14593);
#9719=LINE('',#61499,#14594);
#9720=LINE('',#61501,#14595);
#9721=LINE('',#61503,#14596);
#9722=LINE('',#61505,#14597);
#9723=LINE('',#61507,#14598);
#9724=LINE('',#61508,#14599);
#9725=LINE('',#61511,#14600);
#9726=LINE('',#61513,#14601);
#9727=LINE('',#61515,#14602);
#9728=LINE('',#61517,#14603);
#9729=LINE('',#61519,#14604);
#9730=LINE('',#61520,#14605);
#9731=LINE('',#61523,#14606);
#9732=LINE('',#61525,#14607);
#9733=LINE('',#61527,#14608);
#9734=LINE('',#61529,#14609);
#9735=LINE('',#61531,#14610);
#9736=LINE('',#61532,#14611);
#9737=LINE('',#61535,#14612);
#9738=LINE('',#61537,#14613);
#9739=LINE('',#61539,#14614);
#9740=LINE('',#61541,#14615);
#9741=LINE('',#61543,#14616);
#9742=LINE('',#61544,#14617);
#9743=LINE('',#61547,#14618);
#9744=LINE('',#61549,#14619);
#9745=LINE('',#61551,#14620);
#9746=LINE('',#61553,#14621);
#9747=LINE('',#61555,#14622);
#9748=LINE('',#61556,#14623);
#9749=LINE('',#61559,#14624);
#9750=LINE('',#61561,#14625);
#9751=LINE('',#61563,#14626);
#9752=LINE('',#61565,#14627);
#9753=LINE('',#61567,#14628);
#9754=LINE('',#61568,#14629);
#9755=LINE('',#61571,#14630);
#9756=LINE('',#61573,#14631);
#9757=LINE('',#61575,#14632);
#9758=LINE('',#61577,#14633);
#9759=LINE('',#61579,#14634);
#9760=LINE('',#61580,#14635);
#9761=LINE('',#61583,#14636);
#9762=LINE('',#61585,#14637);
#9763=LINE('',#61587,#14638);
#9764=LINE('',#61589,#14639);
#9765=LINE('',#61591,#14640);
#9766=LINE('',#61592,#14641);
#9767=LINE('',#61595,#14642);
#9768=LINE('',#61597,#14643);
#9769=LINE('',#61599,#14644);
#9770=LINE('',#61601,#14645);
#9771=LINE('',#61603,#14646);
#9772=LINE('',#61604,#14647);
#9773=LINE('',#61607,#14648);
#9774=LINE('',#61609,#14649);
#9775=LINE('',#61611,#14650);
#9776=LINE('',#61613,#14651);
#9777=LINE('',#61615,#14652);
#9778=LINE('',#61616,#14653);
#9779=LINE('',#61619,#14654);
#9780=LINE('',#61621,#14655);
#9781=LINE('',#61623,#14656);
#9782=LINE('',#61625,#14657);
#9783=LINE('',#61627,#14658);
#9784=LINE('',#61628,#14659);
#9785=LINE('',#61631,#14660);
#9786=LINE('',#61633,#14661);
#9787=LINE('',#61635,#14662);
#9788=LINE('',#61637,#14663);
#9789=LINE('',#61639,#14664);
#9790=LINE('',#61640,#14665);
#9791=LINE('',#61643,#14666);
#9792=LINE('',#61645,#14667);
#9793=LINE('',#61647,#14668);
#9794=LINE('',#61649,#14669);
#9795=LINE('',#61651,#14670);
#9796=LINE('',#61652,#14671);
#9797=LINE('',#61655,#14672);
#9798=LINE('',#61657,#14673);
#9799=LINE('',#61659,#14674);
#9800=LINE('',#61661,#14675);
#9801=LINE('',#61663,#14676);
#9802=LINE('',#61664,#14677);
#9803=LINE('',#61667,#14678);
#9804=LINE('',#61669,#14679);
#9805=LINE('',#61671,#14680);
#9806=LINE('',#61673,#14681);
#9807=LINE('',#61675,#14682);
#9808=LINE('',#61676,#14683);
#9809=LINE('',#61679,#14684);
#9810=LINE('',#61681,#14685);
#9811=LINE('',#61683,#14686);
#9812=LINE('',#61685,#14687);
#9813=LINE('',#61687,#14688);
#9814=LINE('',#61688,#14689);
#9815=LINE('',#61691,#14690);
#9816=LINE('',#61693,#14691);
#9817=LINE('',#61695,#14692);
#9818=LINE('',#61697,#14693);
#9819=LINE('',#61699,#14694);
#9820=LINE('',#61700,#14695);
#9821=LINE('',#61703,#14696);
#9822=LINE('',#61705,#14697);
#9823=LINE('',#61707,#14698);
#9824=LINE('',#61709,#14699);
#9825=LINE('',#61711,#14700);
#9826=LINE('',#61712,#14701);
#9827=LINE('',#61715,#14702);
#9828=LINE('',#61717,#14703);
#9829=LINE('',#61719,#14704);
#9830=LINE('',#61721,#14705);
#9831=LINE('',#61723,#14706);
#9832=LINE('',#61724,#14707);
#9833=LINE('',#61727,#14708);
#9834=LINE('',#61729,#14709);
#9835=LINE('',#61731,#14710);
#9836=LINE('',#61733,#14711);
#9837=LINE('',#61735,#14712);
#9838=LINE('',#61736,#14713);
#9839=LINE('',#61739,#14714);
#9840=LINE('',#61741,#14715);
#9841=LINE('',#61743,#14716);
#9842=LINE('',#61745,#14717);
#9843=LINE('',#61747,#14718);
#9844=LINE('',#61748,#14719);
#9845=LINE('',#61751,#14720);
#9846=LINE('',#61753,#14721);
#9847=LINE('',#61755,#14722);
#9848=LINE('',#61757,#14723);
#9849=LINE('',#61759,#14724);
#9850=LINE('',#61760,#14725);
#9851=LINE('',#61763,#14726);
#9852=LINE('',#61765,#14727);
#9853=LINE('',#61767,#14728);
#9854=LINE('',#61769,#14729);
#9855=LINE('',#61771,#14730);
#9856=LINE('',#61772,#14731);
#9857=LINE('',#61775,#14732);
#9858=LINE('',#61777,#14733);
#9859=LINE('',#61779,#14734);
#9860=LINE('',#61781,#14735);
#9861=LINE('',#61783,#14736);
#9862=LINE('',#61784,#14737);
#9863=LINE('',#61787,#14738);
#9864=LINE('',#61789,#14739);
#9865=LINE('',#61791,#14740);
#9866=LINE('',#61793,#14741);
#9867=LINE('',#61795,#14742);
#9868=LINE('',#61796,#14743);
#9869=LINE('',#61799,#14744);
#9870=LINE('',#61801,#14745);
#9871=LINE('',#61803,#14746);
#9872=LINE('',#61805,#14747);
#9873=LINE('',#61807,#14748);
#9874=LINE('',#61808,#14749);
#9875=LINE('',#61811,#14750);
#9876=LINE('',#61813,#14751);
#9877=LINE('',#61815,#14752);
#9878=LINE('',#61817,#14753);
#9879=LINE('',#61819,#14754);
#9880=LINE('',#61820,#14755);
#9881=LINE('',#61823,#14756);
#9882=LINE('',#61825,#14757);
#9883=LINE('',#61827,#14758);
#9884=LINE('',#61829,#14759);
#9885=LINE('',#61831,#14760);
#9886=LINE('',#61832,#14761);
#9887=LINE('',#61835,#14762);
#9888=LINE('',#61837,#14763);
#9889=LINE('',#61839,#14764);
#9890=LINE('',#61841,#14765);
#9891=LINE('',#61843,#14766);
#9892=LINE('',#61844,#14767);
#9893=LINE('',#61847,#14768);
#9894=LINE('',#61849,#14769);
#9895=LINE('',#61851,#14770);
#9896=LINE('',#61853,#14771);
#9897=LINE('',#61855,#14772);
#9898=LINE('',#61856,#14773);
#9899=LINE('',#61859,#14774);
#9900=LINE('',#61861,#14775);
#9901=LINE('',#61863,#14776);
#9902=LINE('',#61865,#14777);
#9903=LINE('',#61867,#14778);
#9904=LINE('',#61868,#14779);
#9905=LINE('',#61871,#14780);
#9906=LINE('',#61873,#14781);
#9907=LINE('',#61875,#14782);
#9908=LINE('',#61877,#14783);
#9909=LINE('',#61879,#14784);
#9910=LINE('',#61880,#14785);
#9911=LINE('',#61883,#14786);
#9912=LINE('',#61885,#14787);
#9913=LINE('',#61887,#14788);
#9914=LINE('',#61889,#14789);
#9915=LINE('',#61891,#14790);
#9916=LINE('',#61892,#14791);
#9917=LINE('',#61895,#14792);
#9918=LINE('',#61897,#14793);
#9919=LINE('',#61899,#14794);
#9920=LINE('',#61901,#14795);
#9921=LINE('',#61903,#14796);
#9922=LINE('',#61904,#14797);
#9923=LINE('',#61907,#14798);
#9924=LINE('',#61909,#14799);
#9925=LINE('',#61911,#14800);
#9926=LINE('',#61913,#14801);
#9927=LINE('',#61915,#14802);
#9928=LINE('',#61916,#14803);
#9929=LINE('',#61919,#14804);
#9930=LINE('',#61921,#14805);
#9931=LINE('',#61923,#14806);
#9932=LINE('',#61925,#14807);
#9933=LINE('',#61927,#14808);
#9934=LINE('',#61928,#14809);
#9935=LINE('',#61931,#14810);
#9936=LINE('',#61933,#14811);
#9937=LINE('',#61935,#14812);
#9938=LINE('',#61937,#14813);
#9939=LINE('',#61939,#14814);
#9940=LINE('',#61940,#14815);
#9941=LINE('',#61943,#14816);
#9942=LINE('',#61945,#14817);
#9943=LINE('',#61947,#14818);
#9944=LINE('',#61949,#14819);
#9945=LINE('',#61951,#14820);
#9946=LINE('',#61952,#14821);
#9947=LINE('',#61955,#14822);
#9948=LINE('',#61957,#14823);
#9949=LINE('',#61959,#14824);
#9950=LINE('',#61961,#14825);
#9951=LINE('',#61963,#14826);
#9952=LINE('',#61964,#14827);
#9953=LINE('',#61967,#14828);
#9954=LINE('',#61969,#14829);
#9955=LINE('',#61971,#14830);
#9956=LINE('',#61973,#14831);
#9957=LINE('',#61975,#14832);
#9958=LINE('',#61976,#14833);
#9959=LINE('',#61979,#14834);
#9960=LINE('',#61981,#14835);
#9961=LINE('',#61983,#14836);
#9962=LINE('',#61985,#14837);
#9963=LINE('',#61987,#14838);
#9964=LINE('',#61988,#14839);
#9965=LINE('',#61991,#14840);
#9966=LINE('',#61993,#14841);
#9967=LINE('',#61995,#14842);
#9968=LINE('',#61997,#14843);
#9969=LINE('',#61999,#14844);
#9970=LINE('',#62000,#14845);
#9971=LINE('',#62003,#14846);
#9972=LINE('',#62005,#14847);
#9973=LINE('',#62007,#14848);
#9974=LINE('',#62009,#14849);
#9975=LINE('',#62011,#14850);
#9976=LINE('',#62012,#14851);
#9977=LINE('',#62015,#14852);
#9978=LINE('',#62017,#14853);
#9979=LINE('',#62019,#14854);
#9980=LINE('',#62021,#14855);
#9981=LINE('',#62023,#14856);
#9982=LINE('',#62024,#14857);
#9983=LINE('',#62027,#14858);
#9984=LINE('',#62029,#14859);
#9985=LINE('',#62031,#14860);
#9986=LINE('',#62033,#14861);
#9987=LINE('',#62035,#14862);
#9988=LINE('',#62036,#14863);
#9989=LINE('',#62039,#14864);
#9990=LINE('',#62041,#14865);
#9991=LINE('',#62043,#14866);
#9992=LINE('',#62045,#14867);
#9993=LINE('',#62047,#14868);
#9994=LINE('',#62048,#14869);
#9995=LINE('',#62051,#14870);
#9996=LINE('',#62053,#14871);
#9997=LINE('',#62055,#14872);
#9998=LINE('',#62057,#14873);
#9999=LINE('',#62059,#14874);
#10000=LINE('',#62060,#14875);
#10001=LINE('',#62063,#14876);
#10002=LINE('',#62065,#14877);
#10003=LINE('',#62067,#14878);
#10004=LINE('',#62069,#14879);
#10005=LINE('',#62071,#14880);
#10006=LINE('',#62072,#14881);
#10007=LINE('',#62075,#14882);
#10008=LINE('',#62077,#14883);
#10009=LINE('',#62079,#14884);
#10010=LINE('',#62081,#14885);
#10011=LINE('',#62083,#14886);
#10012=LINE('',#62084,#14887);
#10013=LINE('',#62087,#14888);
#10014=LINE('',#62089,#14889);
#10015=LINE('',#62091,#14890);
#10016=LINE('',#62093,#14891);
#10017=LINE('',#62095,#14892);
#10018=LINE('',#62096,#14893);
#10019=LINE('',#62099,#14894);
#10020=LINE('',#62101,#14895);
#10021=LINE('',#62103,#14896);
#10022=LINE('',#62105,#14897);
#10023=LINE('',#62107,#14898);
#10024=LINE('',#62108,#14899);
#10025=LINE('',#62111,#14900);
#10026=LINE('',#62113,#14901);
#10027=LINE('',#62115,#14902);
#10028=LINE('',#62117,#14903);
#10029=LINE('',#62119,#14904);
#10030=LINE('',#62120,#14905);
#10031=LINE('',#62123,#14906);
#10032=LINE('',#62125,#14907);
#10033=LINE('',#62127,#14908);
#10034=LINE('',#62129,#14909);
#10035=LINE('',#62131,#14910);
#10036=LINE('',#62132,#14911);
#10037=LINE('',#62135,#14912);
#10038=LINE('',#62137,#14913);
#10039=LINE('',#62139,#14914);
#10040=LINE('',#62141,#14915);
#10041=LINE('',#62143,#14916);
#10042=LINE('',#62144,#14917);
#10043=LINE('',#62147,#14918);
#10044=LINE('',#62149,#14919);
#10045=LINE('',#62151,#14920);
#10046=LINE('',#62153,#14921);
#10047=LINE('',#62155,#14922);
#10048=LINE('',#62156,#14923);
#10049=LINE('',#62159,#14924);
#10050=LINE('',#62161,#14925);
#10051=LINE('',#62163,#14926);
#10052=LINE('',#62165,#14927);
#10053=LINE('',#62167,#14928);
#10054=LINE('',#62168,#14929);
#10055=LINE('',#62171,#14930);
#10056=LINE('',#62173,#14931);
#10057=LINE('',#62175,#14932);
#10058=LINE('',#62177,#14933);
#10059=LINE('',#62179,#14934);
#10060=LINE('',#62180,#14935);
#10061=LINE('',#62183,#14936);
#10062=LINE('',#62185,#14937);
#10063=LINE('',#62187,#14938);
#10064=LINE('',#62189,#14939);
#10065=LINE('',#62191,#14940);
#10066=LINE('',#62192,#14941);
#10067=LINE('',#62195,#14942);
#10068=LINE('',#62197,#14943);
#10069=LINE('',#62199,#14944);
#10070=LINE('',#62201,#14945);
#10071=LINE('',#62203,#14946);
#10072=LINE('',#62204,#14947);
#10073=LINE('',#62207,#14948);
#10074=LINE('',#62209,#14949);
#10075=LINE('',#62211,#14950);
#10076=LINE('',#62213,#14951);
#10077=LINE('',#62215,#14952);
#10078=LINE('',#62216,#14953);
#10079=LINE('',#62219,#14954);
#10080=LINE('',#62221,#14955);
#10081=LINE('',#62223,#14956);
#10082=LINE('',#62225,#14957);
#10083=LINE('',#62227,#14958);
#10084=LINE('',#62228,#14959);
#10085=LINE('',#62231,#14960);
#10086=LINE('',#62233,#14961);
#10087=LINE('',#62235,#14962);
#10088=LINE('',#62237,#14963);
#10089=LINE('',#62239,#14964);
#10090=LINE('',#62240,#14965);
#10091=LINE('',#62243,#14966);
#10092=LINE('',#62245,#14967);
#10093=LINE('',#62247,#14968);
#10094=LINE('',#62249,#14969);
#10095=LINE('',#62251,#14970);
#10096=LINE('',#62252,#14971);
#10097=LINE('',#62255,#14972);
#10098=LINE('',#62257,#14973);
#10099=LINE('',#62259,#14974);
#10100=LINE('',#62261,#14975);
#10101=LINE('',#62263,#14976);
#10102=LINE('',#62264,#14977);
#10103=LINE('',#62267,#14978);
#10104=LINE('',#62269,#14979);
#10105=LINE('',#62271,#14980);
#10106=LINE('',#62273,#14981);
#10107=LINE('',#62275,#14982);
#10108=LINE('',#62276,#14983);
#10109=LINE('',#62279,#14984);
#10110=LINE('',#62281,#14985);
#10111=LINE('',#62283,#14986);
#10112=LINE('',#62285,#14987);
#10113=LINE('',#62287,#14988);
#10114=LINE('',#62288,#14989);
#10115=LINE('',#62291,#14990);
#10116=LINE('',#62293,#14991);
#10117=LINE('',#62295,#14992);
#10118=LINE('',#62297,#14993);
#10119=LINE('',#62299,#14994);
#10120=LINE('',#62300,#14995);
#10121=LINE('',#62303,#14996);
#10122=LINE('',#62305,#14997);
#10123=LINE('',#62307,#14998);
#10124=LINE('',#62309,#14999);
#10125=LINE('',#62311,#15000);
#10126=LINE('',#62312,#15001);
#10127=LINE('',#62315,#15002);
#10128=LINE('',#62317,#15003);
#10129=LINE('',#62319,#15004);
#10130=LINE('',#62321,#15005);
#10131=LINE('',#62323,#15006);
#10132=LINE('',#62324,#15007);
#10133=LINE('',#62327,#15008);
#10134=LINE('',#62329,#15009);
#10135=LINE('',#62331,#15010);
#10136=LINE('',#62333,#15011);
#10137=LINE('',#62335,#15012);
#10138=LINE('',#62336,#15013);
#10139=LINE('',#62339,#15014);
#10140=LINE('',#62341,#15015);
#10141=LINE('',#62343,#15016);
#10142=LINE('',#62345,#15017);
#10143=LINE('',#62347,#15018);
#10144=LINE('',#62348,#15019);
#10145=LINE('',#62351,#15020);
#10146=LINE('',#62353,#15021);
#10147=LINE('',#62355,#15022);
#10148=LINE('',#62357,#15023);
#10149=LINE('',#62359,#15024);
#10150=LINE('',#62360,#15025);
#10151=LINE('',#62363,#15026);
#10152=LINE('',#62365,#15027);
#10153=LINE('',#62367,#15028);
#10154=LINE('',#62369,#15029);
#10155=LINE('',#62371,#15030);
#10156=LINE('',#62372,#15031);
#10157=LINE('',#62375,#15032);
#10158=LINE('',#62377,#15033);
#10159=LINE('',#62379,#15034);
#10160=LINE('',#62381,#15035);
#10161=LINE('',#62383,#15036);
#10162=LINE('',#62384,#15037);
#10163=LINE('',#62387,#15038);
#10164=LINE('',#62389,#15039);
#10165=LINE('',#62391,#15040);
#10166=LINE('',#62393,#15041);
#10167=LINE('',#62395,#15042);
#10168=LINE('',#62396,#15043);
#10169=LINE('',#62399,#15044);
#10170=LINE('',#62401,#15045);
#10171=LINE('',#62403,#15046);
#10172=LINE('',#62405,#15047);
#10173=LINE('',#62407,#15048);
#10174=LINE('',#62408,#15049);
#10175=LINE('',#62411,#15050);
#10176=LINE('',#62413,#15051);
#10177=LINE('',#62415,#15052);
#10178=LINE('',#62417,#15053);
#10179=LINE('',#62419,#15054);
#10180=LINE('',#62420,#15055);
#10181=LINE('',#62423,#15056);
#10182=LINE('',#62425,#15057);
#10183=LINE('',#62427,#15058);
#10184=LINE('',#62429,#15059);
#10185=LINE('',#62431,#15060);
#10186=LINE('',#62432,#15061);
#10187=LINE('',#62435,#15062);
#10188=LINE('',#62437,#15063);
#10189=LINE('',#62439,#15064);
#10190=LINE('',#62441,#15065);
#10191=LINE('',#62443,#15066);
#10192=LINE('',#62444,#15067);
#10193=LINE('',#62447,#15068);
#10194=LINE('',#62449,#15069);
#10195=LINE('',#62451,#15070);
#10196=LINE('',#62453,#15071);
#10197=LINE('',#62455,#15072);
#10198=LINE('',#62456,#15073);
#10199=LINE('',#62459,#15074);
#10200=LINE('',#62461,#15075);
#10201=LINE('',#62463,#15076);
#10202=LINE('',#62465,#15077);
#10203=LINE('',#62467,#15078);
#10204=LINE('',#62468,#15079);
#10205=LINE('',#62471,#15080);
#10206=LINE('',#62473,#15081);
#10207=LINE('',#62475,#15082);
#10208=LINE('',#62477,#15083);
#10209=LINE('',#62479,#15084);
#10210=LINE('',#62480,#15085);
#10211=LINE('',#62483,#15086);
#10212=LINE('',#62485,#15087);
#10213=LINE('',#62487,#15088);
#10214=LINE('',#62489,#15089);
#10215=LINE('',#62491,#15090);
#10216=LINE('',#62492,#15091);
#10217=LINE('',#62495,#15092);
#10218=LINE('',#62497,#15093);
#10219=LINE('',#62499,#15094);
#10220=LINE('',#62501,#15095);
#10221=LINE('',#62503,#15096);
#10222=LINE('',#62504,#15097);
#10223=LINE('',#62507,#15098);
#10224=LINE('',#62509,#15099);
#10225=LINE('',#62511,#15100);
#10226=LINE('',#62513,#15101);
#10227=LINE('',#62515,#15102);
#10228=LINE('',#62516,#15103);
#10229=LINE('',#62519,#15104);
#10230=LINE('',#62521,#15105);
#10231=LINE('',#62523,#15106);
#10232=LINE('',#62525,#15107);
#10233=LINE('',#62527,#15108);
#10234=LINE('',#62528,#15109);
#10235=LINE('',#62531,#15110);
#10236=LINE('',#62533,#15111);
#10237=LINE('',#62535,#15112);
#10238=LINE('',#62537,#15113);
#10239=LINE('',#62539,#15114);
#10240=LINE('',#62540,#15115);
#10241=LINE('',#62543,#15116);
#10242=LINE('',#62545,#15117);
#10243=LINE('',#62547,#15118);
#10244=LINE('',#62549,#15119);
#10245=LINE('',#62551,#15120);
#10246=LINE('',#62552,#15121);
#10247=LINE('',#62555,#15122);
#10248=LINE('',#62557,#15123);
#10249=LINE('',#62559,#15124);
#10250=LINE('',#62561,#15125);
#10251=LINE('',#62563,#15126);
#10252=LINE('',#62564,#15127);
#10253=LINE('',#62567,#15128);
#10254=LINE('',#62569,#15129);
#10255=LINE('',#62571,#15130);
#10256=LINE('',#62573,#15131);
#10257=LINE('',#62575,#15132);
#10258=LINE('',#62576,#15133);
#10259=LINE('',#62579,#15134);
#10260=LINE('',#62581,#15135);
#10261=LINE('',#62583,#15136);
#10262=LINE('',#62585,#15137);
#10263=LINE('',#62587,#15138);
#10264=LINE('',#62588,#15139);
#10265=LINE('',#62591,#15140);
#10266=LINE('',#62593,#15141);
#10267=LINE('',#62595,#15142);
#10268=LINE('',#62597,#15143);
#10269=LINE('',#62599,#15144);
#10270=LINE('',#62600,#15145);
#10271=LINE('',#62603,#15146);
#10272=LINE('',#62605,#15147);
#10273=LINE('',#62607,#15148);
#10274=LINE('',#62609,#15149);
#10275=LINE('',#62611,#15150);
#10276=LINE('',#62612,#15151);
#10277=LINE('',#62615,#15152);
#10278=LINE('',#62617,#15153);
#10279=LINE('',#62619,#15154);
#10280=LINE('',#62621,#15155);
#10281=LINE('',#62623,#15156);
#10282=LINE('',#62624,#15157);
#10283=LINE('',#62627,#15158);
#10284=LINE('',#62629,#15159);
#10285=LINE('',#62631,#15160);
#10286=LINE('',#62633,#15161);
#10287=LINE('',#62635,#15162);
#10288=LINE('',#62636,#15163);
#10289=LINE('',#62639,#15164);
#10290=LINE('',#62641,#15165);
#10291=LINE('',#62643,#15166);
#10292=LINE('',#62645,#15167);
#10293=LINE('',#62647,#15168);
#10294=LINE('',#62648,#15169);
#10295=LINE('',#62651,#15170);
#10296=LINE('',#62653,#15171);
#10297=LINE('',#62655,#15172);
#10298=LINE('',#62657,#15173);
#10299=LINE('',#62659,#15174);
#10300=LINE('',#62660,#15175);
#10301=LINE('',#62663,#15176);
#10302=LINE('',#62665,#15177);
#10303=LINE('',#62667,#15178);
#10304=LINE('',#62669,#15179);
#10305=LINE('',#62671,#15180);
#10306=LINE('',#62672,#15181);
#10307=LINE('',#62675,#15182);
#10308=LINE('',#62677,#15183);
#10309=LINE('',#62679,#15184);
#10310=LINE('',#62681,#15185);
#10311=LINE('',#62683,#15186);
#10312=LINE('',#62684,#15187);
#10313=LINE('',#62687,#15188);
#10314=LINE('',#62689,#15189);
#10315=LINE('',#62691,#15190);
#10316=LINE('',#62693,#15191);
#10317=LINE('',#62695,#15192);
#10318=LINE('',#62696,#15193);
#10319=LINE('',#62699,#15194);
#10320=LINE('',#62701,#15195);
#10321=LINE('',#62703,#15196);
#10322=LINE('',#62705,#15197);
#10323=LINE('',#62707,#15198);
#10324=LINE('',#62708,#15199);
#10325=LINE('',#62711,#15200);
#10326=LINE('',#62713,#15201);
#10327=LINE('',#62715,#15202);
#10328=LINE('',#62717,#15203);
#10329=LINE('',#62719,#15204);
#10330=LINE('',#62720,#15205);
#10331=LINE('',#62723,#15206);
#10332=LINE('',#62725,#15207);
#10333=LINE('',#62727,#15208);
#10334=LINE('',#62729,#15209);
#10335=LINE('',#62731,#15210);
#10336=LINE('',#62732,#15211);
#10337=LINE('',#62735,#15212);
#10338=LINE('',#62737,#15213);
#10339=LINE('',#62739,#15214);
#10340=LINE('',#62741,#15215);
#10341=LINE('',#62743,#15216);
#10342=LINE('',#62744,#15217);
#10343=LINE('',#62747,#15218);
#10344=LINE('',#62749,#15219);
#10345=LINE('',#62751,#15220);
#10346=LINE('',#62753,#15221);
#10347=LINE('',#62755,#15222);
#10348=LINE('',#62756,#15223);
#10349=LINE('',#62759,#15224);
#10350=LINE('',#62761,#15225);
#10351=LINE('',#62763,#15226);
#10352=LINE('',#62765,#15227);
#10353=LINE('',#62767,#15228);
#10354=LINE('',#62768,#15229);
#10355=LINE('',#62771,#15230);
#10356=LINE('',#62773,#15231);
#10357=LINE('',#62775,#15232);
#10358=LINE('',#62777,#15233);
#10359=LINE('',#62779,#15234);
#10360=LINE('',#62780,#15235);
#10361=LINE('',#62783,#15236);
#10362=LINE('',#62785,#15237);
#10363=LINE('',#62787,#15238);
#10364=LINE('',#62789,#15239);
#10365=LINE('',#62791,#15240);
#10366=LINE('',#62792,#15241);
#10367=LINE('',#62795,#15242);
#10368=LINE('',#62797,#15243);
#10369=LINE('',#62799,#15244);
#10370=LINE('',#62801,#15245);
#10371=LINE('',#62803,#15246);
#10372=LINE('',#62804,#15247);
#10373=LINE('',#62807,#15248);
#10374=LINE('',#62809,#15249);
#10375=LINE('',#62811,#15250);
#10376=LINE('',#62813,#15251);
#10377=LINE('',#62815,#15252);
#10378=LINE('',#62816,#15253);
#10379=LINE('',#62819,#15254);
#10380=LINE('',#62821,#15255);
#10381=LINE('',#62823,#15256);
#10382=LINE('',#62825,#15257);
#10383=LINE('',#62827,#15258);
#10384=LINE('',#62828,#15259);
#10385=LINE('',#62831,#15260);
#10386=LINE('',#62833,#15261);
#10387=LINE('',#62835,#15262);
#10388=LINE('',#62837,#15263);
#10389=LINE('',#62839,#15264);
#10390=LINE('',#62840,#15265);
#10391=LINE('',#62843,#15266);
#10392=LINE('',#62845,#15267);
#10393=LINE('',#62847,#15268);
#10394=LINE('',#62849,#15269);
#10395=LINE('',#62851,#15270);
#10396=LINE('',#62852,#15271);
#10397=LINE('',#62855,#15272);
#10398=LINE('',#62857,#15273);
#10399=LINE('',#62859,#15274);
#10400=LINE('',#62861,#15275);
#10401=LINE('',#62863,#15276);
#10402=LINE('',#62864,#15277);
#10403=LINE('',#62867,#15278);
#10404=LINE('',#62869,#15279);
#10405=LINE('',#62871,#15280);
#10406=LINE('',#62873,#15281);
#10407=LINE('',#62875,#15282);
#10408=LINE('',#62876,#15283);
#10409=LINE('',#62879,#15284);
#10410=LINE('',#62881,#15285);
#10411=LINE('',#62883,#15286);
#10412=LINE('',#62885,#15287);
#10413=LINE('',#62887,#15288);
#10414=LINE('',#62888,#15289);
#10415=LINE('',#62891,#15290);
#10416=LINE('',#62893,#15291);
#10417=LINE('',#62895,#15292);
#10418=LINE('',#62897,#15293);
#10419=LINE('',#62899,#15294);
#10420=LINE('',#62900,#15295);
#10421=LINE('',#62903,#15296);
#10422=LINE('',#62905,#15297);
#10423=LINE('',#62907,#15298);
#10424=LINE('',#62909,#15299);
#10425=LINE('',#62911,#15300);
#10426=LINE('',#62912,#15301);
#10427=LINE('',#62915,#15302);
#10428=LINE('',#62917,#15303);
#10429=LINE('',#62919,#15304);
#10430=LINE('',#62921,#15305);
#10431=LINE('',#62923,#15306);
#10432=LINE('',#62924,#15307);
#10433=LINE('',#62927,#15308);
#10434=LINE('',#62929,#15309);
#10435=LINE('',#62931,#15310);
#10436=LINE('',#62933,#15311);
#10437=LINE('',#62935,#15312);
#10438=LINE('',#62936,#15313);
#10439=LINE('',#62939,#15314);
#10440=LINE('',#62941,#15315);
#10441=LINE('',#62943,#15316);
#10442=LINE('',#62945,#15317);
#10443=LINE('',#62947,#15318);
#10444=LINE('',#62948,#15319);
#10445=LINE('',#62951,#15320);
#10446=LINE('',#62953,#15321);
#10447=LINE('',#62955,#15322);
#10448=LINE('',#62957,#15323);
#10449=LINE('',#62959,#15324);
#10450=LINE('',#62960,#15325);
#10451=LINE('',#62963,#15326);
#10452=LINE('',#62965,#15327);
#10453=LINE('',#62967,#15328);
#10454=LINE('',#62969,#15329);
#10455=LINE('',#62971,#15330);
#10456=LINE('',#62972,#15331);
#10457=LINE('',#62975,#15332);
#10458=LINE('',#62977,#15333);
#10459=LINE('',#62979,#15334);
#10460=LINE('',#62981,#15335);
#10461=LINE('',#62983,#15336);
#10462=LINE('',#62984,#15337);
#10463=LINE('',#62987,#15338);
#10464=LINE('',#62989,#15339);
#10465=LINE('',#62991,#15340);
#10466=LINE('',#62993,#15341);
#10467=LINE('',#62995,#15342);
#10468=LINE('',#62996,#15343);
#10469=LINE('',#62999,#15344);
#10470=LINE('',#63001,#15345);
#10471=LINE('',#63003,#15346);
#10472=LINE('',#63005,#15347);
#10473=LINE('',#63007,#15348);
#10474=LINE('',#63008,#15349);
#10475=LINE('',#63011,#15350);
#10476=LINE('',#63013,#15351);
#10477=LINE('',#63015,#15352);
#10478=LINE('',#63017,#15353);
#10479=LINE('',#63019,#15354);
#10480=LINE('',#63020,#15355);
#10481=LINE('',#63023,#15356);
#10482=LINE('',#63025,#15357);
#10483=LINE('',#63027,#15358);
#10484=LINE('',#63029,#15359);
#10485=LINE('',#63031,#15360);
#10486=LINE('',#63032,#15361);
#10487=LINE('',#63035,#15362);
#10488=LINE('',#63037,#15363);
#10489=LINE('',#63039,#15364);
#10490=LINE('',#63041,#15365);
#10491=LINE('',#63043,#15366);
#10492=LINE('',#63044,#15367);
#10493=LINE('',#63047,#15368);
#10494=LINE('',#63049,#15369);
#10495=LINE('',#63051,#15370);
#10496=LINE('',#63053,#15371);
#10497=LINE('',#63055,#15372);
#10498=LINE('',#63056,#15373);
#10499=LINE('',#63058,#15374);
#10500=LINE('',#63059,#15375);
#10501=LINE('',#63061,#15376);
#10502=LINE('',#63063,#15377);
#10503=LINE('',#63065,#15378);
#10504=LINE('',#63067,#15379);
#10505=LINE('',#63070,#15380);
#10506=LINE('',#63071,#15381);
#10507=LINE('',#63073,#15382);
#10508=LINE('',#63075,#15383);
#10509=LINE('',#63077,#15384);
#10510=LINE('',#63079,#15385);
#10511=LINE('',#63082,#15386);
#10512=LINE('',#63083,#15387);
#10513=LINE('',#63085,#15388);
#10514=LINE('',#63087,#15389);
#10515=LINE('',#63089,#15390);
#10516=LINE('',#63091,#15391);
#10517=LINE('',#63094,#15392);
#10518=LINE('',#63095,#15393);
#10519=LINE('',#63097,#15394);
#10520=LINE('',#63099,#15395);
#10521=LINE('',#63101,#15396);
#10522=LINE('',#63103,#15397);
#10523=LINE('',#63106,#15398);
#10524=LINE('',#63107,#15399);
#10525=LINE('',#63109,#15400);
#10526=LINE('',#63111,#15401);
#10527=LINE('',#63113,#15402);
#10528=LINE('',#63115,#15403);
#10529=LINE('',#63118,#15404);
#10530=LINE('',#63119,#15405);
#10531=LINE('',#63121,#15406);
#10532=LINE('',#63123,#15407);
#10533=LINE('',#63125,#15408);
#10534=LINE('',#63127,#15409);
#10535=LINE('',#63130,#15410);
#10536=LINE('',#63131,#15411);
#10537=LINE('',#63133,#15412);
#10538=LINE('',#63135,#15413);
#10539=LINE('',#63137,#15414);
#10540=LINE('',#63139,#15415);
#10541=LINE('',#63142,#15416);
#10542=LINE('',#63143,#15417);
#10543=LINE('',#63145,#15418);
#10544=LINE('',#63147,#15419);
#10545=LINE('',#63149,#15420);
#10546=LINE('',#63151,#15421);
#10547=LINE('',#63154,#15422);
#10548=LINE('',#63155,#15423);
#10549=LINE('',#63157,#15424);
#10550=LINE('',#63159,#15425);
#10551=LINE('',#63161,#15426);
#10552=LINE('',#63163,#15427);
#10553=LINE('',#63166,#15428);
#10554=LINE('',#63167,#15429);
#10555=LINE('',#63169,#15430);
#10556=LINE('',#63171,#15431);
#10557=LINE('',#63173,#15432);
#10558=LINE('',#63175,#15433);
#10559=LINE('',#63178,#15434);
#10560=LINE('',#63179,#15435);
#10561=LINE('',#63181,#15436);
#10562=LINE('',#63183,#15437);
#10563=LINE('',#63185,#15438);
#10564=LINE('',#63187,#15439);
#10565=LINE('',#63190,#15440);
#10566=LINE('',#63191,#15441);
#10567=LINE('',#63193,#15442);
#10568=LINE('',#63195,#15443);
#10569=LINE('',#63197,#15444);
#10570=LINE('',#63199,#15445);
#10571=LINE('',#63202,#15446);
#10572=LINE('',#63203,#15447);
#10573=LINE('',#63205,#15448);
#10574=LINE('',#63207,#15449);
#10575=LINE('',#63209,#15450);
#10576=LINE('',#63211,#15451);
#10577=LINE('',#63214,#15452);
#10578=LINE('',#63215,#15453);
#10579=LINE('',#63217,#15454);
#10580=LINE('',#63219,#15455);
#10581=LINE('',#63221,#15456);
#10582=LINE('',#63223,#15457);
#10583=LINE('',#63226,#15458);
#10584=LINE('',#63227,#15459);
#10585=LINE('',#63229,#15460);
#10586=LINE('',#63231,#15461);
#10587=LINE('',#63233,#15462);
#10588=LINE('',#63235,#15463);
#10589=LINE('',#63238,#15464);
#10590=LINE('',#63239,#15465);
#10591=LINE('',#63241,#15466);
#10592=LINE('',#63243,#15467);
#10593=LINE('',#63245,#15468);
#10594=LINE('',#63247,#15469);
#10595=LINE('',#63250,#15470);
#10596=LINE('',#63251,#15471);
#10597=LINE('',#63253,#15472);
#10598=LINE('',#63255,#15473);
#10599=LINE('',#63257,#15474);
#10600=LINE('',#63259,#15475);
#10601=LINE('',#63262,#15476);
#10602=LINE('',#63263,#15477);
#10603=LINE('',#63265,#15478);
#10604=LINE('',#63267,#15479);
#10605=LINE('',#63269,#15480);
#10606=LINE('',#63271,#15481);
#10607=LINE('',#63274,#15482);
#10608=LINE('',#63275,#15483);
#10609=LINE('',#63277,#15484);
#10610=LINE('',#63279,#15485);
#10611=LINE('',#63281,#15486);
#10612=LINE('',#63283,#15487);
#10613=LINE('',#63286,#15488);
#10614=LINE('',#63287,#15489);
#10615=LINE('',#63289,#15490);
#10616=LINE('',#63291,#15491);
#10617=LINE('',#63293,#15492);
#10618=LINE('',#63295,#15493);
#10619=LINE('',#63298,#15494);
#10620=LINE('',#63299,#15495);
#10621=LINE('',#63301,#15496);
#10622=LINE('',#63303,#15497);
#10623=LINE('',#63305,#15498);
#10624=LINE('',#63307,#15499);
#10625=LINE('',#63310,#15500);
#10626=LINE('',#63311,#15501);
#10627=LINE('',#63313,#15502);
#10628=LINE('',#63315,#15503);
#10629=LINE('',#63317,#15504);
#10630=LINE('',#63319,#15505);
#10631=LINE('',#63322,#15506);
#10632=LINE('',#63323,#15507);
#10633=LINE('',#63325,#15508);
#10634=LINE('',#63327,#15509);
#10635=LINE('',#63329,#15510);
#10636=LINE('',#63331,#15511);
#10637=LINE('',#63334,#15512);
#10638=LINE('',#63335,#15513);
#10639=LINE('',#63337,#15514);
#10640=LINE('',#63339,#15515);
#10641=LINE('',#63341,#15516);
#10642=LINE('',#63343,#15517);
#10643=LINE('',#63346,#15518);
#10644=LINE('',#63347,#15519);
#10645=LINE('',#63349,#15520);
#10646=LINE('',#63351,#15521);
#10647=LINE('',#63353,#15522);
#10648=LINE('',#63355,#15523);
#10649=LINE('',#63358,#15524);
#10650=LINE('',#63359,#15525);
#10651=LINE('',#63361,#15526);
#10652=LINE('',#63363,#15527);
#10653=LINE('',#63365,#15528);
#10654=LINE('',#63367,#15529);
#10655=LINE('',#63370,#15530);
#10656=LINE('',#63371,#15531);
#10657=LINE('',#63373,#15532);
#10658=LINE('',#63375,#15533);
#10659=LINE('',#63377,#15534);
#10660=LINE('',#63379,#15535);
#10661=LINE('',#63382,#15536);
#10662=LINE('',#63383,#15537);
#10663=LINE('',#63385,#15538);
#10664=LINE('',#63387,#15539);
#10665=LINE('',#63389,#15540);
#10666=LINE('',#63391,#15541);
#10667=LINE('',#63394,#15542);
#10668=LINE('',#63395,#15543);
#10669=LINE('',#63397,#15544);
#10670=LINE('',#63399,#15545);
#10671=LINE('',#63401,#15546);
#10672=LINE('',#63403,#15547);
#10673=LINE('',#63406,#15548);
#10674=LINE('',#63407,#15549);
#10675=LINE('',#63409,#15550);
#10676=LINE('',#63411,#15551);
#10677=LINE('',#63413,#15552);
#10678=LINE('',#63415,#15553);
#10679=LINE('',#63418,#15554);
#10680=LINE('',#63419,#15555);
#10681=LINE('',#63421,#15556);
#10682=LINE('',#63423,#15557);
#10683=LINE('',#63425,#15558);
#10684=LINE('',#63427,#15559);
#10685=LINE('',#63430,#15560);
#10686=LINE('',#63431,#15561);
#10687=LINE('',#63433,#15562);
#10688=LINE('',#63435,#15563);
#10689=LINE('',#63437,#15564);
#10690=LINE('',#63439,#15565);
#10691=LINE('',#63442,#15566);
#10692=LINE('',#63443,#15567);
#10693=LINE('',#63445,#15568);
#10694=LINE('',#63447,#15569);
#10695=LINE('',#63449,#15570);
#10696=LINE('',#63451,#15571);
#10697=LINE('',#63454,#15572);
#10698=LINE('',#63455,#15573);
#10699=LINE('',#63457,#15574);
#10700=LINE('',#63459,#15575);
#10701=LINE('',#63461,#15576);
#10702=LINE('',#63463,#15577);
#10703=LINE('',#63466,#15578);
#10704=LINE('',#63467,#15579);
#10705=LINE('',#63469,#15580);
#10706=LINE('',#63471,#15581);
#10707=LINE('',#63473,#15582);
#10708=LINE('',#63475,#15583);
#10709=LINE('',#63478,#15584);
#10710=LINE('',#63479,#15585);
#10711=LINE('',#63481,#15586);
#10712=LINE('',#63483,#15587);
#10713=LINE('',#63485,#15588);
#10714=LINE('',#63487,#15589);
#10715=LINE('',#63490,#15590);
#10716=LINE('',#63491,#15591);
#10717=LINE('',#63493,#15592);
#10718=LINE('',#63495,#15593);
#10719=LINE('',#63497,#15594);
#10720=LINE('',#63499,#15595);
#10721=LINE('',#63502,#15596);
#10722=LINE('',#63503,#15597);
#10723=LINE('',#63505,#15598);
#10724=LINE('',#63507,#15599);
#10725=LINE('',#63509,#15600);
#10726=LINE('',#63511,#15601);
#10727=LINE('',#63514,#15602);
#10728=LINE('',#63515,#15603);
#10729=LINE('',#63517,#15604);
#10730=LINE('',#63519,#15605);
#10731=LINE('',#63521,#15606);
#10732=LINE('',#63523,#15607);
#10733=LINE('',#63526,#15608);
#10734=LINE('',#63527,#15609);
#10735=LINE('',#63529,#15610);
#10736=LINE('',#63531,#15611);
#10737=LINE('',#63533,#15612);
#10738=LINE('',#63535,#15613);
#10739=LINE('',#63538,#15614);
#10740=LINE('',#63539,#15615);
#10741=LINE('',#63541,#15616);
#10742=LINE('',#63543,#15617);
#10743=LINE('',#63545,#15618);
#10744=LINE('',#63547,#15619);
#10745=LINE('',#63550,#15620);
#10746=LINE('',#63551,#15621);
#10747=LINE('',#63553,#15622);
#10748=LINE('',#63555,#15623);
#10749=LINE('',#63557,#15624);
#10750=LINE('',#63559,#15625);
#10751=LINE('',#63562,#15626);
#10752=LINE('',#63563,#15627);
#10753=LINE('',#63565,#15628);
#10754=LINE('',#63567,#15629);
#10755=LINE('',#63569,#15630);
#10756=LINE('',#63571,#15631);
#10757=LINE('',#63574,#15632);
#10758=LINE('',#63575,#15633);
#10759=LINE('',#63577,#15634);
#10760=LINE('',#63579,#15635);
#10761=LINE('',#63581,#15636);
#10762=LINE('',#63583,#15637);
#10763=LINE('',#63586,#15638);
#10764=LINE('',#63587,#15639);
#10765=LINE('',#63589,#15640);
#10766=LINE('',#63591,#15641);
#10767=LINE('',#63593,#15642);
#10768=LINE('',#63595,#15643);
#10769=LINE('',#63598,#15644);
#10770=LINE('',#63599,#15645);
#10771=LINE('',#63601,#15646);
#10772=LINE('',#63603,#15647);
#10773=LINE('',#63605,#15648);
#10774=LINE('',#63607,#15649);
#10775=LINE('',#63610,#15650);
#10776=LINE('',#63611,#15651);
#10777=LINE('',#63613,#15652);
#10778=LINE('',#63615,#15653);
#10779=LINE('',#63617,#15654);
#10780=LINE('',#63619,#15655);
#10781=LINE('',#63622,#15656);
#10782=LINE('',#63623,#15657);
#10783=LINE('',#63625,#15658);
#10784=LINE('',#63627,#15659);
#10785=LINE('',#63629,#15660);
#10786=LINE('',#63631,#15661);
#10787=LINE('',#63634,#15662);
#10788=LINE('',#63635,#15663);
#10789=LINE('',#63637,#15664);
#10790=LINE('',#63639,#15665);
#10791=LINE('',#63641,#15666);
#10792=LINE('',#63643,#15667);
#10793=LINE('',#63646,#15668);
#10794=LINE('',#63647,#15669);
#10795=LINE('',#63649,#15670);
#10796=LINE('',#63651,#15671);
#10797=LINE('',#63653,#15672);
#10798=LINE('',#63655,#15673);
#10799=LINE('',#63658,#15674);
#10800=LINE('',#63659,#15675);
#10801=LINE('',#63661,#15676);
#10802=LINE('',#63663,#15677);
#10803=LINE('',#63665,#15678);
#10804=LINE('',#63667,#15679);
#10805=LINE('',#63670,#15680);
#10806=LINE('',#63671,#15681);
#10807=LINE('',#63673,#15682);
#10808=LINE('',#63675,#15683);
#10809=LINE('',#63677,#15684);
#10810=LINE('',#63679,#15685);
#10811=LINE('',#63682,#15686);
#10812=LINE('',#63683,#15687);
#10813=LINE('',#63685,#15688);
#10814=LINE('',#63687,#15689);
#10815=LINE('',#63689,#15690);
#10816=LINE('',#63691,#15691);
#10817=LINE('',#63694,#15692);
#10818=LINE('',#63695,#15693);
#10819=LINE('',#63697,#15694);
#10820=LINE('',#63699,#15695);
#10821=LINE('',#63701,#15696);
#10822=LINE('',#63703,#15697);
#10823=LINE('',#63706,#15698);
#10824=LINE('',#63707,#15699);
#10825=LINE('',#63709,#15700);
#10826=LINE('',#63711,#15701);
#10827=LINE('',#63713,#15702);
#10828=LINE('',#63715,#15703);
#10829=LINE('',#63718,#15704);
#10830=LINE('',#63719,#15705);
#10831=LINE('',#63721,#15706);
#10832=LINE('',#63723,#15707);
#10833=LINE('',#63725,#15708);
#10834=LINE('',#63727,#15709);
#10835=LINE('',#63730,#15710);
#10836=LINE('',#63731,#15711);
#10837=LINE('',#63733,#15712);
#10838=LINE('',#63735,#15713);
#10839=LINE('',#63737,#15714);
#10840=LINE('',#63739,#15715);
#10841=LINE('',#63742,#15716);
#10842=LINE('',#63743,#15717);
#10843=LINE('',#63745,#15718);
#10844=LINE('',#63747,#15719);
#10845=LINE('',#63749,#15720);
#10846=LINE('',#63751,#15721);
#10847=LINE('',#63754,#15722);
#10848=LINE('',#63755,#15723);
#10849=LINE('',#63757,#15724);
#10850=LINE('',#63759,#15725);
#10851=LINE('',#63761,#15726);
#10852=LINE('',#63763,#15727);
#10853=LINE('',#63766,#15728);
#10854=LINE('',#63767,#15729);
#10855=LINE('',#63769,#15730);
#10856=LINE('',#63771,#15731);
#10857=LINE('',#63773,#15732);
#10858=LINE('',#63775,#15733);
#10859=LINE('',#63778,#15734);
#10860=LINE('',#63779,#15735);
#10861=LINE('',#63781,#15736);
#10862=LINE('',#63783,#15737);
#10863=LINE('',#63785,#15738);
#10864=LINE('',#63787,#15739);
#10865=LINE('',#63790,#15740);
#10866=LINE('',#63791,#15741);
#10867=LINE('',#63793,#15742);
#10868=LINE('',#63795,#15743);
#10869=LINE('',#63797,#15744);
#10870=LINE('',#63799,#15745);
#10871=LINE('',#63802,#15746);
#10872=LINE('',#63803,#15747);
#10873=LINE('',#63805,#15748);
#10874=LINE('',#63807,#15749);
#10875=LINE('',#63809,#15750);
#10876=LINE('',#63811,#15751);
#10877=LINE('',#63814,#15752);
#10878=LINE('',#63815,#15753);
#10879=LINE('',#63817,#15754);
#10880=LINE('',#63819,#15755);
#10881=LINE('',#63821,#15756);
#10882=LINE('',#63823,#15757);
#10883=LINE('',#63826,#15758);
#10884=LINE('',#63827,#15759);
#10885=LINE('',#63829,#15760);
#10886=LINE('',#63831,#15761);
#10887=LINE('',#63833,#15762);
#10888=LINE('',#63835,#15763);
#10889=LINE('',#63838,#15764);
#10890=LINE('',#63839,#15765);
#10891=LINE('',#63841,#15766);
#10892=LINE('',#63843,#15767);
#10893=LINE('',#63845,#15768);
#10894=LINE('',#63847,#15769);
#10895=LINE('',#63850,#15770);
#10896=LINE('',#63851,#15771);
#10897=LINE('',#63853,#15772);
#10898=LINE('',#63855,#15773);
#10899=LINE('',#63857,#15774);
#10900=LINE('',#63859,#15775);
#10901=LINE('',#63862,#15776);
#10902=LINE('',#63863,#15777);
#10903=LINE('',#63865,#15778);
#10904=LINE('',#63867,#15779);
#10905=LINE('',#63869,#15780);
#10906=LINE('',#63871,#15781);
#10907=LINE('',#63874,#15782);
#10908=LINE('',#63875,#15783);
#10909=LINE('',#63877,#15784);
#10910=LINE('',#63879,#15785);
#10911=LINE('',#63881,#15786);
#10912=LINE('',#63883,#15787);
#10913=LINE('',#63886,#15788);
#10914=LINE('',#63887,#15789);
#10915=LINE('',#63889,#15790);
#10916=LINE('',#63891,#15791);
#10917=LINE('',#63893,#15792);
#10918=LINE('',#63895,#15793);
#10919=LINE('',#63898,#15794);
#10920=LINE('',#63899,#15795);
#10921=LINE('',#63901,#15796);
#10922=LINE('',#63903,#15797);
#10923=LINE('',#63905,#15798);
#10924=LINE('',#63907,#15799);
#10925=LINE('',#63910,#15800);
#10926=LINE('',#63911,#15801);
#10927=LINE('',#63913,#15802);
#10928=LINE('',#63915,#15803);
#10929=LINE('',#63917,#15804);
#10930=LINE('',#63919,#15805);
#10931=LINE('',#63922,#15806);
#10932=LINE('',#63923,#15807);
#10933=LINE('',#63925,#15808);
#10934=LINE('',#63927,#15809);
#10935=LINE('',#63929,#15810);
#10936=LINE('',#63931,#15811);
#10937=LINE('',#63934,#15812);
#10938=LINE('',#63935,#15813);
#10939=LINE('',#63937,#15814);
#10940=LINE('',#63939,#15815);
#10941=LINE('',#63941,#15816);
#10942=LINE('',#63943,#15817);
#10943=LINE('',#63946,#15818);
#10944=LINE('',#63947,#15819);
#10945=LINE('',#63949,#15820);
#10946=LINE('',#63951,#15821);
#10947=LINE('',#63953,#15822);
#10948=LINE('',#63955,#15823);
#10949=LINE('',#63958,#15824);
#10950=LINE('',#63959,#15825);
#10951=LINE('',#63961,#15826);
#10952=LINE('',#63963,#15827);
#10953=LINE('',#63965,#15828);
#10954=LINE('',#63967,#15829);
#10955=LINE('',#63970,#15830);
#10956=LINE('',#63971,#15831);
#10957=LINE('',#63973,#15832);
#10958=LINE('',#63975,#15833);
#10959=LINE('',#63977,#15834);
#10960=LINE('',#63979,#15835);
#10961=LINE('',#63982,#15836);
#10962=LINE('',#63983,#15837);
#10963=LINE('',#63985,#15838);
#10964=LINE('',#63987,#15839);
#10965=LINE('',#63989,#15840);
#10966=LINE('',#63991,#15841);
#10967=LINE('',#63994,#15842);
#10968=LINE('',#63995,#15843);
#10969=LINE('',#63997,#15844);
#10970=LINE('',#63999,#15845);
#10971=LINE('',#64001,#15846);
#10972=LINE('',#64003,#15847);
#10973=LINE('',#64006,#15848);
#10974=LINE('',#64007,#15849);
#10975=LINE('',#64009,#15850);
#10976=LINE('',#64011,#15851);
#10977=LINE('',#64013,#15852);
#10978=LINE('',#64015,#15853);
#10979=LINE('',#64018,#15854);
#10980=LINE('',#64019,#15855);
#10981=LINE('',#64021,#15856);
#10982=LINE('',#64023,#15857);
#10983=LINE('',#64025,#15858);
#10984=LINE('',#64027,#15859);
#10985=LINE('',#64030,#15860);
#10986=LINE('',#64031,#15861);
#10987=LINE('',#64033,#15862);
#10988=LINE('',#64035,#15863);
#10989=LINE('',#64037,#15864);
#10990=LINE('',#64039,#15865);
#10991=LINE('',#64042,#15866);
#10992=LINE('',#64043,#15867);
#10993=LINE('',#64045,#15868);
#10994=LINE('',#64047,#15869);
#10995=LINE('',#64049,#15870);
#10996=LINE('',#64051,#15871);
#10997=LINE('',#64054,#15872);
#10998=LINE('',#64055,#15873);
#10999=LINE('',#64057,#15874);
#11000=LINE('',#64059,#15875);
#11001=LINE('',#64061,#15876);
#11002=LINE('',#64063,#15877);
#11003=LINE('',#64066,#15878);
#11004=LINE('',#64067,#15879);
#11005=LINE('',#64069,#15880);
#11006=LINE('',#64071,#15881);
#11007=LINE('',#64073,#15882);
#11008=LINE('',#64075,#15883);
#11009=LINE('',#64078,#15884);
#11010=LINE('',#64079,#15885);
#11011=LINE('',#64081,#15886);
#11012=LINE('',#64083,#15887);
#11013=LINE('',#64085,#15888);
#11014=LINE('',#64087,#15889);
#11015=LINE('',#64090,#15890);
#11016=LINE('',#64091,#15891);
#11017=LINE('',#64093,#15892);
#11018=LINE('',#64095,#15893);
#11019=LINE('',#64097,#15894);
#11020=LINE('',#64099,#15895);
#11021=LINE('',#64102,#15896);
#11022=LINE('',#64103,#15897);
#11023=LINE('',#64105,#15898);
#11024=LINE('',#64107,#15899);
#11025=LINE('',#64109,#15900);
#11026=LINE('',#64111,#15901);
#11027=LINE('',#64114,#15902);
#11028=LINE('',#64115,#15903);
#11029=LINE('',#64117,#15904);
#11030=LINE('',#64119,#15905);
#11031=LINE('',#64121,#15906);
#11032=LINE('',#64123,#15907);
#11033=LINE('',#64126,#15908);
#11034=LINE('',#64127,#15909);
#11035=LINE('',#64129,#15910);
#11036=LINE('',#64131,#15911);
#11037=LINE('',#64133,#15912);
#11038=LINE('',#64135,#15913);
#11039=LINE('',#64138,#15914);
#11040=LINE('',#64139,#15915);
#11041=LINE('',#64141,#15916);
#11042=LINE('',#64143,#15917);
#11043=LINE('',#64145,#15918);
#11044=LINE('',#64147,#15919);
#11045=LINE('',#64150,#15920);
#11046=LINE('',#64151,#15921);
#11047=LINE('',#64153,#15922);
#11048=LINE('',#64155,#15923);
#11049=LINE('',#64157,#15924);
#11050=LINE('',#64159,#15925);
#11051=LINE('',#64162,#15926);
#11052=LINE('',#64163,#15927);
#11053=LINE('',#64165,#15928);
#11054=LINE('',#64167,#15929);
#11055=LINE('',#64169,#15930);
#11056=LINE('',#64171,#15931);
#11057=LINE('',#64174,#15932);
#11058=LINE('',#64175,#15933);
#11059=LINE('',#64177,#15934);
#11060=LINE('',#64179,#15935);
#11061=LINE('',#64181,#15936);
#11062=LINE('',#64183,#15937);
#11063=LINE('',#64186,#15938);
#11064=LINE('',#64187,#15939);
#11065=LINE('',#64189,#15940);
#11066=LINE('',#64191,#15941);
#11067=LINE('',#64193,#15942);
#11068=LINE('',#64195,#15943);
#11069=LINE('',#64198,#15944);
#11070=LINE('',#64199,#15945);
#11071=LINE('',#64201,#15946);
#11072=LINE('',#64203,#15947);
#11073=LINE('',#64205,#15948);
#11074=LINE('',#64207,#15949);
#11075=LINE('',#64210,#15950);
#11076=LINE('',#64211,#15951);
#11077=LINE('',#64213,#15952);
#11078=LINE('',#64215,#15953);
#11079=LINE('',#64217,#15954);
#11080=LINE('',#64219,#15955);
#11081=LINE('',#64222,#15956);
#11082=LINE('',#64223,#15957);
#11083=LINE('',#64225,#15958);
#11084=LINE('',#64227,#15959);
#11085=LINE('',#64229,#15960);
#11086=LINE('',#64231,#15961);
#11087=LINE('',#64234,#15962);
#11088=LINE('',#64235,#15963);
#11089=LINE('',#64237,#15964);
#11090=LINE('',#64239,#15965);
#11091=LINE('',#64241,#15966);
#11092=LINE('',#64243,#15967);
#11093=LINE('',#64246,#15968);
#11094=LINE('',#64247,#15969);
#11095=LINE('',#64249,#15970);
#11096=LINE('',#64251,#15971);
#11097=LINE('',#64253,#15972);
#11098=LINE('',#64255,#15973);
#11099=LINE('',#64258,#15974);
#11100=LINE('',#64259,#15975);
#11101=LINE('',#64261,#15976);
#11102=LINE('',#64263,#15977);
#11103=LINE('',#64265,#15978);
#11104=LINE('',#64267,#15979);
#11105=LINE('',#64270,#15980);
#11106=LINE('',#64271,#15981);
#11107=LINE('',#64273,#15982);
#11108=LINE('',#64275,#15983);
#11109=LINE('',#64277,#15984);
#11110=LINE('',#64279,#15985);
#11111=LINE('',#64282,#15986);
#11112=LINE('',#64283,#15987);
#11113=LINE('',#64285,#15988);
#11114=LINE('',#64287,#15989);
#11115=LINE('',#64289,#15990);
#11116=LINE('',#64291,#15991);
#11117=LINE('',#64294,#15992);
#11118=LINE('',#64295,#15993);
#11119=LINE('',#64297,#15994);
#11120=LINE('',#64299,#15995);
#11121=LINE('',#64301,#15996);
#11122=LINE('',#64303,#15997);
#11123=LINE('',#64306,#15998);
#11124=LINE('',#64307,#15999);
#11125=LINE('',#64309,#16000);
#11126=LINE('',#64311,#16001);
#11127=LINE('',#64313,#16002);
#11128=LINE('',#64315,#16003);
#11129=LINE('',#64318,#16004);
#11130=LINE('',#64319,#16005);
#11131=LINE('',#64321,#16006);
#11132=LINE('',#64323,#16007);
#11133=LINE('',#64325,#16008);
#11134=LINE('',#64327,#16009);
#11135=LINE('',#64330,#16010);
#11136=LINE('',#64331,#16011);
#11137=LINE('',#64333,#16012);
#11138=LINE('',#64335,#16013);
#11139=LINE('',#64337,#16014);
#11140=LINE('',#64339,#16015);
#11141=LINE('',#64342,#16016);
#11142=LINE('',#64343,#16017);
#11143=LINE('',#64345,#16018);
#11144=LINE('',#64347,#16019);
#11145=LINE('',#64349,#16020);
#11146=LINE('',#64351,#16021);
#11147=LINE('',#64354,#16022);
#11148=LINE('',#64355,#16023);
#11149=LINE('',#64357,#16024);
#11150=LINE('',#64359,#16025);
#11151=LINE('',#64361,#16026);
#11152=LINE('',#64363,#16027);
#11153=LINE('',#64366,#16028);
#11154=LINE('',#64367,#16029);
#11155=LINE('',#64369,#16030);
#11156=LINE('',#64371,#16031);
#11157=LINE('',#64373,#16032);
#11158=LINE('',#64375,#16033);
#11159=LINE('',#64378,#16034);
#11160=LINE('',#64379,#16035);
#11161=LINE('',#64381,#16036);
#11162=LINE('',#64383,#16037);
#11163=LINE('',#64385,#16038);
#11164=LINE('',#64387,#16039);
#11165=LINE('',#64390,#16040);
#11166=LINE('',#64391,#16041);
#11167=LINE('',#64393,#16042);
#11168=LINE('',#64395,#16043);
#11169=LINE('',#64397,#16044);
#11170=LINE('',#64399,#16045);
#11171=LINE('',#64402,#16046);
#11172=LINE('',#64403,#16047);
#11173=LINE('',#64405,#16048);
#11174=LINE('',#64407,#16049);
#11175=LINE('',#64409,#16050);
#11176=LINE('',#64411,#16051);
#11177=LINE('',#64414,#16052);
#11178=LINE('',#64415,#16053);
#11179=LINE('',#64417,#16054);
#11180=LINE('',#64419,#16055);
#11181=LINE('',#64421,#16056);
#11182=LINE('',#64423,#16057);
#11183=LINE('',#64426,#16058);
#11184=LINE('',#64427,#16059);
#11185=LINE('',#64429,#16060);
#11186=LINE('',#64431,#16061);
#11187=LINE('',#64433,#16062);
#11188=LINE('',#64435,#16063);
#11189=LINE('',#64438,#16064);
#11190=LINE('',#64439,#16065);
#11191=LINE('',#64441,#16066);
#11192=LINE('',#64443,#16067);
#11193=LINE('',#64445,#16068);
#11194=LINE('',#64447,#16069);
#11195=LINE('',#64450,#16070);
#11196=LINE('',#64451,#16071);
#11197=LINE('',#64453,#16072);
#11198=LINE('',#64455,#16073);
#11199=LINE('',#64457,#16074);
#11200=LINE('',#64459,#16075);
#11201=LINE('',#64462,#16076);
#11202=LINE('',#64463,#16077);
#11203=LINE('',#64465,#16078);
#11204=LINE('',#64467,#16079);
#11205=LINE('',#64469,#16080);
#11206=LINE('',#64471,#16081);
#11207=LINE('',#64474,#16082);
#11208=LINE('',#64475,#16083);
#11209=LINE('',#64477,#16084);
#11210=LINE('',#64479,#16085);
#11211=LINE('',#64481,#16086);
#11212=LINE('',#64483,#16087);
#11213=LINE('',#64486,#16088);
#11214=LINE('',#64487,#16089);
#11215=LINE('',#64489,#16090);
#11216=LINE('',#64491,#16091);
#11217=LINE('',#64493,#16092);
#11218=LINE('',#64495,#16093);
#11219=LINE('',#64498,#16094);
#11220=LINE('',#64499,#16095);
#11221=LINE('',#64501,#16096);
#11222=LINE('',#64503,#16097);
#11223=LINE('',#64505,#16098);
#11224=LINE('',#64507,#16099);
#11225=LINE('',#64510,#16100);
#11226=LINE('',#64511,#16101);
#11227=LINE('',#64513,#16102);
#11228=LINE('',#64515,#16103);
#11229=LINE('',#64517,#16104);
#11230=LINE('',#64519,#16105);
#11231=LINE('',#64522,#16106);
#11232=LINE('',#64523,#16107);
#11233=LINE('',#64525,#16108);
#11234=LINE('',#64527,#16109);
#11235=LINE('',#64529,#16110);
#11236=LINE('',#64531,#16111);
#11237=LINE('',#64534,#16112);
#11238=LINE('',#64535,#16113);
#11239=LINE('',#64537,#16114);
#11240=LINE('',#64539,#16115);
#11241=LINE('',#64541,#16116);
#11242=LINE('',#64543,#16117);
#11243=LINE('',#64546,#16118);
#11244=LINE('',#64547,#16119);
#11245=LINE('',#64549,#16120);
#11246=LINE('',#64551,#16121);
#11247=LINE('',#64553,#16122);
#11248=LINE('',#64555,#16123);
#11249=LINE('',#64558,#16124);
#11250=LINE('',#64559,#16125);
#11251=LINE('',#64561,#16126);
#11252=LINE('',#64563,#16127);
#11253=LINE('',#64565,#16128);
#11254=LINE('',#64567,#16129);
#11255=LINE('',#64570,#16130);
#11256=LINE('',#64571,#16131);
#11257=LINE('',#64573,#16132);
#11258=LINE('',#64575,#16133);
#11259=LINE('',#64577,#16134);
#11260=LINE('',#64579,#16135);
#11261=LINE('',#64582,#16136);
#11262=LINE('',#64583,#16137);
#11263=LINE('',#64585,#16138);
#11264=LINE('',#64587,#16139);
#11265=LINE('',#64589,#16140);
#11266=LINE('',#64591,#16141);
#11267=LINE('',#64594,#16142);
#11268=LINE('',#64595,#16143);
#11269=LINE('',#64597,#16144);
#11270=LINE('',#64599,#16145);
#11271=LINE('',#64601,#16146);
#11272=LINE('',#64603,#16147);
#11273=LINE('',#64606,#16148);
#11274=LINE('',#64607,#16149);
#11275=LINE('',#64609,#16150);
#11276=LINE('',#64611,#16151);
#11277=LINE('',#64613,#16152);
#11278=LINE('',#64615,#16153);
#11279=LINE('',#64618,#16154);
#11280=LINE('',#64619,#16155);
#11281=LINE('',#64621,#16156);
#11282=LINE('',#64623,#16157);
#11283=LINE('',#64625,#16158);
#11284=LINE('',#64627,#16159);
#11285=LINE('',#64630,#16160);
#11286=LINE('',#64631,#16161);
#11287=LINE('',#64633,#16162);
#11288=LINE('',#64635,#16163);
#11289=LINE('',#64637,#16164);
#11290=LINE('',#64639,#16165);
#11291=LINE('',#64642,#16166);
#11292=LINE('',#64643,#16167);
#11293=LINE('',#64645,#16168);
#11294=LINE('',#64647,#16169);
#11295=LINE('',#64649,#16170);
#11296=LINE('',#64651,#16171);
#11297=LINE('',#64654,#16172);
#11298=LINE('',#64655,#16173);
#11299=LINE('',#64657,#16174);
#11300=LINE('',#64659,#16175);
#11301=LINE('',#64661,#16176);
#11302=LINE('',#64663,#16177);
#11303=LINE('',#64666,#16178);
#11304=LINE('',#64667,#16179);
#11305=LINE('',#64669,#16180);
#11306=LINE('',#64671,#16181);
#11307=LINE('',#64673,#16182);
#11308=LINE('',#64675,#16183);
#11309=LINE('',#64678,#16184);
#11310=LINE('',#64679,#16185);
#11311=LINE('',#64681,#16186);
#11312=LINE('',#64683,#16187);
#11313=LINE('',#64685,#16188);
#11314=LINE('',#64687,#16189);
#11315=LINE('',#64690,#16190);
#11316=LINE('',#64691,#16191);
#11317=LINE('',#64693,#16192);
#11318=LINE('',#64695,#16193);
#11319=LINE('',#64697,#16194);
#11320=LINE('',#64699,#16195);
#11321=LINE('',#64702,#16196);
#11322=LINE('',#64703,#16197);
#11323=LINE('',#64705,#16198);
#11324=LINE('',#64707,#16199);
#11325=LINE('',#64709,#16200);
#11326=LINE('',#64711,#16201);
#11327=LINE('',#64714,#16202);
#11328=LINE('',#64715,#16203);
#11329=LINE('',#64717,#16204);
#11330=LINE('',#64719,#16205);
#11331=LINE('',#64721,#16206);
#11332=LINE('',#64723,#16207);
#11333=LINE('',#64726,#16208);
#11334=LINE('',#64727,#16209);
#11335=LINE('',#64729,#16210);
#11336=LINE('',#64731,#16211);
#11337=LINE('',#64733,#16212);
#11338=LINE('',#64735,#16213);
#11339=LINE('',#64738,#16214);
#11340=LINE('',#64739,#16215);
#11341=LINE('',#64741,#16216);
#11342=LINE('',#64743,#16217);
#11343=LINE('',#64745,#16218);
#11344=LINE('',#64747,#16219);
#11345=LINE('',#64750,#16220);
#11346=LINE('',#64751,#16221);
#11347=LINE('',#64753,#16222);
#11348=LINE('',#64755,#16223);
#11349=LINE('',#64757,#16224);
#11350=LINE('',#64759,#16225);
#11351=LINE('',#64762,#16226);
#11352=LINE('',#64763,#16227);
#11353=LINE('',#64765,#16228);
#11354=LINE('',#64767,#16229);
#11355=LINE('',#64769,#16230);
#11356=LINE('',#64771,#16231);
#11357=LINE('',#64774,#16232);
#11358=LINE('',#64775,#16233);
#11359=LINE('',#64777,#16234);
#11360=LINE('',#64779,#16235);
#11361=LINE('',#64781,#16236);
#11362=LINE('',#64783,#16237);
#11363=LINE('',#64786,#16238);
#11364=LINE('',#64787,#16239);
#11365=LINE('',#64789,#16240);
#11366=LINE('',#64791,#16241);
#11367=LINE('',#64793,#16242);
#11368=LINE('',#64795,#16243);
#11369=LINE('',#64798,#16244);
#11370=LINE('',#64799,#16245);
#11371=LINE('',#64801,#16246);
#11372=LINE('',#64803,#16247);
#11373=LINE('',#64805,#16248);
#11374=LINE('',#64807,#16249);
#11375=LINE('',#64810,#16250);
#11376=LINE('',#64811,#16251);
#11377=LINE('',#64813,#16252);
#11378=LINE('',#64815,#16253);
#11379=LINE('',#64817,#16254);
#11380=LINE('',#64819,#16255);
#11381=LINE('',#64822,#16256);
#11382=LINE('',#64823,#16257);
#11383=LINE('',#64825,#16258);
#11384=LINE('',#64827,#16259);
#11385=LINE('',#64829,#16260);
#11386=LINE('',#64831,#16261);
#11387=LINE('',#64834,#16262);
#11388=LINE('',#64835,#16263);
#11389=LINE('',#64837,#16264);
#11390=LINE('',#64839,#16265);
#11391=LINE('',#64841,#16266);
#11392=LINE('',#64843,#16267);
#11393=LINE('',#64846,#16268);
#11394=LINE('',#64847,#16269);
#11395=LINE('',#64849,#16270);
#11396=LINE('',#64851,#16271);
#11397=LINE('',#64853,#16272);
#11398=LINE('',#64855,#16273);
#11399=LINE('',#64858,#16274);
#11400=LINE('',#64859,#16275);
#11401=LINE('',#64861,#16276);
#11402=LINE('',#64863,#16277);
#11403=LINE('',#64865,#16278);
#11404=LINE('',#64867,#16279);
#11405=LINE('',#64870,#16280);
#11406=LINE('',#64871,#16281);
#11407=LINE('',#64873,#16282);
#11408=LINE('',#64875,#16283);
#11409=LINE('',#64877,#16284);
#11410=LINE('',#64879,#16285);
#11411=LINE('',#64882,#16286);
#11412=LINE('',#64883,#16287);
#11413=LINE('',#64885,#16288);
#11414=LINE('',#64887,#16289);
#11415=LINE('',#64889,#16290);
#11416=LINE('',#64891,#16291);
#11417=LINE('',#64894,#16292);
#11418=LINE('',#64895,#16293);
#11419=LINE('',#64897,#16294);
#11420=LINE('',#64899,#16295);
#11421=LINE('',#64901,#16296);
#11422=LINE('',#64903,#16297);
#11423=LINE('',#64906,#16298);
#11424=LINE('',#64907,#16299);
#11425=LINE('',#64909,#16300);
#11426=LINE('',#64911,#16301);
#11427=LINE('',#64913,#16302);
#11428=LINE('',#64915,#16303);
#11429=LINE('',#64918,#16304);
#11430=LINE('',#64919,#16305);
#11431=LINE('',#64921,#16306);
#11432=LINE('',#64923,#16307);
#11433=LINE('',#64925,#16308);
#11434=LINE('',#64927,#16309);
#11435=LINE('',#64930,#16310);
#11436=LINE('',#64931,#16311);
#11437=LINE('',#64933,#16312);
#11438=LINE('',#64935,#16313);
#11439=LINE('',#64937,#16314);
#11440=LINE('',#64939,#16315);
#11441=LINE('',#64942,#16316);
#11442=LINE('',#64943,#16317);
#11443=LINE('',#64945,#16318);
#11444=LINE('',#64947,#16319);
#11445=LINE('',#64949,#16320);
#11446=LINE('',#64951,#16321);
#11447=LINE('',#64954,#16322);
#11448=LINE('',#64955,#16323);
#11449=LINE('',#64957,#16324);
#11450=LINE('',#64959,#16325);
#11451=LINE('',#64961,#16326);
#11452=LINE('',#64963,#16327);
#11453=LINE('',#64966,#16328);
#11454=LINE('',#64967,#16329);
#11455=LINE('',#64969,#16330);
#11456=LINE('',#64971,#16331);
#11457=LINE('',#64973,#16332);
#11458=LINE('',#64975,#16333);
#11459=LINE('',#64978,#16334);
#11460=LINE('',#64979,#16335);
#11461=LINE('',#64981,#16336);
#11462=LINE('',#64983,#16337);
#11463=LINE('',#64985,#16338);
#11464=LINE('',#64987,#16339);
#11465=LINE('',#64990,#16340);
#11466=LINE('',#64991,#16341);
#11467=LINE('',#64993,#16342);
#11468=LINE('',#64995,#16343);
#11469=LINE('',#64997,#16344);
#11470=LINE('',#64999,#16345);
#11471=LINE('',#65002,#16346);
#11472=LINE('',#65003,#16347);
#11473=LINE('',#65005,#16348);
#11474=LINE('',#65007,#16349);
#11475=LINE('',#65009,#16350);
#11476=LINE('',#65011,#16351);
#11477=LINE('',#65014,#16352);
#11478=LINE('',#65015,#16353);
#11479=LINE('',#65017,#16354);
#11480=LINE('',#65019,#16355);
#11481=LINE('',#65021,#16356);
#11482=LINE('',#65023,#16357);
#11483=LINE('',#65026,#16358);
#11484=LINE('',#65027,#16359);
#11485=LINE('',#65029,#16360);
#11486=LINE('',#65031,#16361);
#11487=LINE('',#65033,#16362);
#11488=LINE('',#65035,#16363);
#11489=LINE('',#65038,#16364);
#11490=LINE('',#65039,#16365);
#11491=LINE('',#65041,#16366);
#11492=LINE('',#65043,#16367);
#11493=LINE('',#65045,#16368);
#11494=LINE('',#65047,#16369);
#11495=LINE('',#65050,#16370);
#11496=LINE('',#65051,#16371);
#11497=LINE('',#65053,#16372);
#11498=LINE('',#65055,#16373);
#11499=LINE('',#65057,#16374);
#11500=LINE('',#65059,#16375);
#11501=LINE('',#65062,#16376);
#11502=LINE('',#65063,#16377);
#11503=LINE('',#65065,#16378);
#11504=LINE('',#65067,#16379);
#11505=LINE('',#65069,#16380);
#11506=LINE('',#65071,#16381);
#11507=LINE('',#65074,#16382);
#11508=LINE('',#65075,#16383);
#11509=LINE('',#65077,#16384);
#11510=LINE('',#65079,#16385);
#11511=LINE('',#65081,#16386);
#11512=LINE('',#65083,#16387);
#11513=LINE('',#65086,#16388);
#11514=LINE('',#65087,#16389);
#11515=LINE('',#65089,#16390);
#11516=LINE('',#65091,#16391);
#11517=LINE('',#65093,#16392);
#11518=LINE('',#65095,#16393);
#11519=LINE('',#65098,#16394);
#11520=LINE('',#65099,#16395);
#11521=LINE('',#65101,#16396);
#11522=LINE('',#65103,#16397);
#11523=LINE('',#65105,#16398);
#11524=LINE('',#65107,#16399);
#11525=LINE('',#65110,#16400);
#11526=LINE('',#65111,#16401);
#11527=LINE('',#65113,#16402);
#11528=LINE('',#65115,#16403);
#11529=LINE('',#65117,#16404);
#11530=LINE('',#65119,#16405);
#11531=LINE('',#65122,#16406);
#11532=LINE('',#65123,#16407);
#11533=LINE('',#65125,#16408);
#11534=LINE('',#65127,#16409);
#11535=LINE('',#65129,#16410);
#11536=LINE('',#65131,#16411);
#11537=LINE('',#65134,#16412);
#11538=LINE('',#65135,#16413);
#11539=LINE('',#65137,#16414);
#11540=LINE('',#65139,#16415);
#11541=LINE('',#65141,#16416);
#11542=LINE('',#65143,#16417);
#11543=LINE('',#65146,#16418);
#11544=LINE('',#65147,#16419);
#11545=LINE('',#65149,#16420);
#11546=LINE('',#65151,#16421);
#11547=LINE('',#65153,#16422);
#11548=LINE('',#65155,#16423);
#11549=LINE('',#65158,#16424);
#11550=LINE('',#65159,#16425);
#11551=LINE('',#65161,#16426);
#11552=LINE('',#65163,#16427);
#11553=LINE('',#65165,#16428);
#11554=LINE('',#65167,#16429);
#11555=LINE('',#65170,#16430);
#11556=LINE('',#65171,#16431);
#11557=LINE('',#65173,#16432);
#11558=LINE('',#65175,#16433);
#11559=LINE('',#65177,#16434);
#11560=LINE('',#65179,#16435);
#11561=LINE('',#65182,#16436);
#11562=LINE('',#65183,#16437);
#11563=LINE('',#65185,#16438);
#11564=LINE('',#65187,#16439);
#11565=LINE('',#65189,#16440);
#11566=LINE('',#65191,#16441);
#11567=LINE('',#65194,#16442);
#11568=LINE('',#65195,#16443);
#11569=LINE('',#65197,#16444);
#11570=LINE('',#65199,#16445);
#11571=LINE('',#65201,#16446);
#11572=LINE('',#65203,#16447);
#11573=LINE('',#65206,#16448);
#11574=LINE('',#65207,#16449);
#11575=LINE('',#65209,#16450);
#11576=LINE('',#65211,#16451);
#11577=LINE('',#65213,#16452);
#11578=LINE('',#65215,#16453);
#11579=LINE('',#65218,#16454);
#11580=LINE('',#65219,#16455);
#11581=LINE('',#65221,#16456);
#11582=LINE('',#65223,#16457);
#11583=LINE('',#65225,#16458);
#11584=LINE('',#65227,#16459);
#11585=LINE('',#65230,#16460);
#11586=LINE('',#65231,#16461);
#11587=LINE('',#65233,#16462);
#11588=LINE('',#65235,#16463);
#11589=LINE('',#65237,#16464);
#11590=LINE('',#65239,#16465);
#11591=LINE('',#65242,#16466);
#11592=LINE('',#65243,#16467);
#11593=LINE('',#65245,#16468);
#11594=LINE('',#65247,#16469);
#11595=LINE('',#65249,#16470);
#11596=LINE('',#65251,#16471);
#11597=LINE('',#65254,#16472);
#11598=LINE('',#65255,#16473);
#11599=LINE('',#65257,#16474);
#11600=LINE('',#65259,#16475);
#11601=LINE('',#65261,#16476);
#11602=LINE('',#65263,#16477);
#11603=LINE('',#65266,#16478);
#11604=LINE('',#65267,#16479);
#11605=LINE('',#65269,#16480);
#11606=LINE('',#65271,#16481);
#11607=LINE('',#65273,#16482);
#11608=LINE('',#65275,#16483);
#11609=LINE('',#65278,#16484);
#11610=LINE('',#65279,#16485);
#11611=LINE('',#65281,#16486);
#11612=LINE('',#65283,#16487);
#11613=LINE('',#65285,#16488);
#11614=LINE('',#65287,#16489);
#11615=VECTOR('',#42522,1.75);
#11616=VECTOR('',#42529,1.75);
#11617=VECTOR('',#42536,1.75);
#11618=VECTOR('',#42543,1.75);
#11619=VECTOR('',#42550,1.25);
#11620=VECTOR('',#42557,1.25);
#11621=VECTOR('',#42564,1000.);
#11622=VECTOR('',#42567,1000.);
#11623=VECTOR('',#42572,1000.);
#11624=VECTOR('',#42575,1000.);
#11625=VECTOR('',#42580,1000.);
#11626=VECTOR('',#42583,1000.);
#11627=VECTOR('',#42588,1000.);
#11628=VECTOR('',#42591,1000.);
#11629=VECTOR('',#42596,1000.);
#11630=VECTOR('',#42599,1000.);
#11631=VECTOR('',#42604,1000.);
#11632=VECTOR('',#42607,1000.);
#11633=VECTOR('',#42612,1000.);
#11634=VECTOR('',#42615,1000.);
#11635=VECTOR('',#42620,1000.);
#11636=VECTOR('',#42623,1000.);
#11637=VECTOR('',#42628,1000.);
#11638=VECTOR('',#42631,1000.);
#11639=VECTOR('',#42636,1000.);
#11640=VECTOR('',#42639,1000.);
#11641=VECTOR('',#42644,1000.);
#11642=VECTOR('',#42647,1000.);
#11643=VECTOR('',#42652,1000.);
#11644=VECTOR('',#42655,1000.);
#11645=VECTOR('',#42660,1000.);
#11646=VECTOR('',#42663,1000.);
#11647=VECTOR('',#42668,1000.);
#11648=VECTOR('',#42671,1000.);
#11649=VECTOR('',#42676,1000.);
#11650=VECTOR('',#42679,1000.);
#11651=VECTOR('',#42684,1000.);
#11652=VECTOR('',#42687,1000.);
#11653=VECTOR('',#42692,1000.);
#11654=VECTOR('',#42695,1000.);
#11655=VECTOR('',#42700,1000.);
#11656=VECTOR('',#42703,1000.);
#11657=VECTOR('',#42708,1000.);
#11658=VECTOR('',#42711,1000.);
#11659=VECTOR('',#42716,1000.);
#11660=VECTOR('',#42719,1000.);
#11661=VECTOR('',#42724,1000.);
#11662=VECTOR('',#42727,1000.);
#11663=VECTOR('',#42732,1000.);
#11664=VECTOR('',#42735,1000.);
#11665=VECTOR('',#42740,1000.);
#11666=VECTOR('',#42743,1000.);
#11667=VECTOR('',#42748,1000.);
#11668=VECTOR('',#42751,1000.);
#11669=VECTOR('',#42756,1000.);
#11670=VECTOR('',#42759,1000.);
#11671=VECTOR('',#42764,1000.);
#11672=VECTOR('',#42767,1000.);
#11673=VECTOR('',#42772,1000.);
#11674=VECTOR('',#42775,1000.);
#11675=VECTOR('',#42780,1000.);
#11676=VECTOR('',#42783,1000.);
#11677=VECTOR('',#42788,1000.);
#11678=VECTOR('',#42791,1000.);
#11679=VECTOR('',#42796,1000.);
#11680=VECTOR('',#42799,1000.);
#11681=VECTOR('',#42804,1000.);
#11682=VECTOR('',#42807,1000.);
#11683=VECTOR('',#42812,1000.);
#11684=VECTOR('',#42815,1000.);
#11685=VECTOR('',#42820,1000.);
#11686=VECTOR('',#42823,1000.);
#11687=VECTOR('',#42828,1000.);
#11688=VECTOR('',#42831,1000.);
#11689=VECTOR('',#42836,1000.);
#11690=VECTOR('',#42839,1000.);
#11691=VECTOR('',#42844,1000.);
#11692=VECTOR('',#42847,1000.);
#11693=VECTOR('',#42852,1000.);
#11694=VECTOR('',#42855,1000.);
#11695=VECTOR('',#42860,1000.);
#11696=VECTOR('',#42863,1000.);
#11697=VECTOR('',#42868,1000.);
#11698=VECTOR('',#42871,1000.);
#11699=VECTOR('',#42876,1000.);
#11700=VECTOR('',#42879,1000.);
#11701=VECTOR('',#42884,1000.);
#11702=VECTOR('',#42887,1000.);
#11703=VECTOR('',#42892,1000.);
#11704=VECTOR('',#42895,1000.);
#11705=VECTOR('',#42900,1000.);
#11706=VECTOR('',#42903,1000.);
#11707=VECTOR('',#42908,1000.);
#11708=VECTOR('',#42911,1000.);
#11709=VECTOR('',#42916,1000.);
#11710=VECTOR('',#42919,1000.);
#11711=VECTOR('',#42924,1000.);
#11712=VECTOR('',#42927,1000.);
#11713=VECTOR('',#42932,1000.);
#11714=VECTOR('',#42935,1000.);
#11715=VECTOR('',#42940,1000.);
#11716=VECTOR('',#42943,1000.);
#11717=VECTOR('',#42948,1000.);
#11718=VECTOR('',#42951,1000.);
#11719=VECTOR('',#42956,1000.);
#11720=VECTOR('',#42959,1000.);
#11721=VECTOR('',#42964,1000.);
#11722=VECTOR('',#42967,1000.);
#11723=VECTOR('',#42972,1000.);
#11724=VECTOR('',#42975,1000.);
#11725=VECTOR('',#42980,1000.);
#11726=VECTOR('',#42983,1000.);
#11727=VECTOR('',#42988,1000.);
#11728=VECTOR('',#42991,1000.);
#11729=VECTOR('',#42996,1000.);
#11730=VECTOR('',#42999,1000.);
#11731=VECTOR('',#43004,1000.);
#11732=VECTOR('',#43007,1000.);
#11733=VECTOR('',#43012,1000.);
#11734=VECTOR('',#43015,1000.);
#11735=VECTOR('',#43020,1000.);
#11736=VECTOR('',#43023,1000.);
#11737=VECTOR('',#43028,1000.);
#11738=VECTOR('',#43031,1000.);
#11739=VECTOR('',#43036,1000.);
#11740=VECTOR('',#43039,1000.);
#11741=VECTOR('',#43044,1000.);
#11742=VECTOR('',#43047,1000.);
#11743=VECTOR('',#43052,1000.);
#11744=VECTOR('',#43055,1000.);
#11745=VECTOR('',#43060,1000.);
#11746=VECTOR('',#43063,1000.);
#11747=VECTOR('',#43068,1000.);
#11748=VECTOR('',#43071,1000.);
#11749=VECTOR('',#43076,1000.);
#11750=VECTOR('',#43079,1000.);
#11751=VECTOR('',#43084,1000.);
#11752=VECTOR('',#43087,1000.);
#11753=VECTOR('',#43088,1000.);
#11754=VECTOR('',#43089,1000.);
#11755=VECTOR('',#43090,1000.);
#11756=VECTOR('',#43091,1000.);
#11757=VECTOR('',#43092,1000.);
#11758=VECTOR('',#43093,1000.);
#11759=VECTOR('',#43094,1000.);
#11760=VECTOR('',#43095,1000.);
#11761=VECTOR('',#43096,1000.);
#11762=VECTOR('',#43097,1000.);
#11763=VECTOR('',#43102,1.74999999999999);
#11764=VECTOR('',#43109,1.74999999999998);
#11765=VECTOR('',#43116,1.75);
#11766=VECTOR('',#43123,1.75);
#11767=VECTOR('',#43158,1.25);
#11768=VECTOR('',#43165,1.25);
#11769=VECTOR('',#43172,1.25);
#11770=VECTOR('',#43179,1.25);
#11771=VECTOR('',#43182,1000.);
#11772=VECTOR('',#43183,1000.);
#11773=VECTOR('',#43186,1000.);
#11774=VECTOR('',#43187,1000.);
#11775=VECTOR('',#43188,1000.);
#11776=VECTOR('',#43191,1000.);
#11777=VECTOR('',#43194,1000.);
#11778=VECTOR('',#43195,1000.);
#11779=VECTOR('',#43196,1000.);
#11780=VECTOR('',#43197,1000.);
#11781=VECTOR('',#43198,1000.);
#11782=VECTOR('',#43199,1000.);
#11783=VECTOR('',#43200,1000.);
#11784=VECTOR('',#43201,1000.);
#11785=VECTOR('',#43202,1000.);
#11786=VECTOR('',#43203,1000.);
#11787=VECTOR('',#43204,1000.);
#11788=VECTOR('',#43207,1000.);
#11789=VECTOR('',#43210,1000.);
#11790=VECTOR('',#43211,1000.);
#11791=VECTOR('',#43212,1000.);
#11792=VECTOR('',#43213,1000.);
#11793=VECTOR('',#43214,1000.);
#11794=VECTOR('',#43215,1000.);
#11795=VECTOR('',#43216,1000.);
#11796=VECTOR('',#43217,1000.);
#11797=VECTOR('',#43218,1000.);
#11798=VECTOR('',#43219,1000.);
#11799=VECTOR('',#43220,1000.);
#11800=VECTOR('',#43221,1000.);
#11801=VECTOR('',#43222,1000.);
#11802=VECTOR('',#43223,1000.);
#11803=VECTOR('',#43224,1000.);
#11804=VECTOR('',#43225,1000.);
#11805=VECTOR('',#43226,1000.);
#11806=VECTOR('',#43227,1000.);
#11807=VECTOR('',#43228,1000.);
#11808=VECTOR('',#43229,1000.);
#11809=VECTOR('',#43230,1000.);
#11810=VECTOR('',#43231,1000.);
#11811=VECTOR('',#43232,1000.);
#11812=VECTOR('',#43233,1000.);
#11813=VECTOR('',#43234,1000.);
#11814=VECTOR('',#43235,1000.);
#11815=VECTOR('',#43236,1000.);
#11816=VECTOR('',#43237,1000.);
#11817=VECTOR('',#43238,1000.);
#11818=VECTOR('',#43239,1000.);
#11819=VECTOR('',#43240,1000.);
#11820=VECTOR('',#43241,1000.);
#11821=VECTOR('',#43242,1000.);
#11822=VECTOR('',#43243,1000.);
#11823=VECTOR('',#43244,1000.);
#11824=VECTOR('',#43245,1000.);
#11825=VECTOR('',#43246,1000.);
#11826=VECTOR('',#43247,1000.);
#11827=VECTOR('',#43248,1000.);
#11828=VECTOR('',#43249,1000.);
#11829=VECTOR('',#43252,1000.);
#11830=VECTOR('',#43253,1000.);
#11831=VECTOR('',#43254,1000.);
#11832=VECTOR('',#43255,1000.);
#11833=VECTOR('',#43256,1000.);
#11834=VECTOR('',#43257,1000.);
#11835=VECTOR('',#43258,1000.);
#11836=VECTOR('',#43259,1000.);
#11837=VECTOR('',#43260,1000.);
#11838=VECTOR('',#43261,1000.);
#11839=VECTOR('',#43264,1000.);
#11840=VECTOR('',#43267,1000.);
#11841=VECTOR('',#43268,1000.);
#11842=VECTOR('',#43269,1000.);
#11843=VECTOR('',#43270,1000.);
#11844=VECTOR('',#43271,1000.);
#11845=VECTOR('',#43272,1000.);
#11846=VECTOR('',#43273,1000.);
#11847=VECTOR('',#43274,1000.);
#11848=VECTOR('',#43275,1000.);
#11849=VECTOR('',#43276,1000.);
#11850=VECTOR('',#43277,1000.);
#11851=VECTOR('',#43280,1000.);
#11852=VECTOR('',#43283,1000.);
#11853=VECTOR('',#43284,1000.);
#11854=VECTOR('',#43285,1000.);
#11855=VECTOR('',#43286,1000.);
#11856=VECTOR('',#43287,1000.);
#11857=VECTOR('',#43288,1000.);
#11858=VECTOR('',#43289,1000.);
#11859=VECTOR('',#43290,1000.);
#11860=VECTOR('',#43291,1000.);
#11861=VECTOR('',#43292,1000.);
#11862=VECTOR('',#43293,1000.);
#11863=VECTOR('',#43294,1000.);
#11864=VECTOR('',#43295,1000.);
#11865=VECTOR('',#43296,1000.);
#11866=VECTOR('',#43297,1000.);
#11867=VECTOR('',#43298,1000.);
#11868=VECTOR('',#43299,1000.);
#11869=VECTOR('',#43302,1000.);
#11870=VECTOR('',#43303,1000.);
#11871=VECTOR('',#43306,1000.);
#11872=VECTOR('',#43307,1000.);
#11873=VECTOR('',#43310,1000.);
#11874=VECTOR('',#43311,1000.);
#11875=VECTOR('',#43312,1000.);
#11876=VECTOR('',#43315,1000.);
#11877=VECTOR('',#43318,1000.);
#11878=VECTOR('',#43319,1000.);
#11879=VECTOR('',#43320,1000.);
#11880=VECTOR('',#43321,1000.);
#11881=VECTOR('',#43322,1000.);
#11882=VECTOR('',#43323,1000.);
#11883=VECTOR('',#43324,1000.);
#11884=VECTOR('',#43325,1000.);
#11885=VECTOR('',#43326,1000.);
#11886=VECTOR('',#43327,1000.);
#11887=VECTOR('',#43328,1000.);
#11888=VECTOR('',#43329,1000.);
#11889=VECTOR('',#43330,1000.);
#11890=VECTOR('',#43331,1000.);
#11891=VECTOR('',#43332,1000.);
#11892=VECTOR('',#43333,1000.);
#11893=VECTOR('',#43336,1000.);
#11894=VECTOR('',#43337,1000.);
#11895=VECTOR('',#43340,1000.);
#11896=VECTOR('',#43343,1000.);
#11897=VECTOR('',#43344,1000.);
#11898=VECTOR('',#43345,1000.);
#11899=VECTOR('',#43346,1000.);
#11900=VECTOR('',#43347,1000.);
#11901=VECTOR('',#43348,1000.);
#11902=VECTOR('',#43349,1000.);
#11903=VECTOR('',#43350,1000.);
#11904=VECTOR('',#43351,1000.);
#11905=VECTOR('',#43354,1000.);
#11906=VECTOR('',#43355,1000.);
#11907=VECTOR('',#43358,1000.);
#11908=VECTOR('',#43359,1000.);
#11909=VECTOR('',#43362,1000.);
#11910=VECTOR('',#43363,1000.);
#11911=VECTOR('',#43364,1000.);
#11912=VECTOR('',#43365,1000.);
#11913=VECTOR('',#43366,1000.);
#11914=VECTOR('',#43367,1000.);
#11915=VECTOR('',#43370,1000.);
#11916=VECTOR('',#43373,1000.);
#11917=VECTOR('',#43374,1000.);
#11918=VECTOR('',#43375,1000.);
#11919=VECTOR('',#43378,1000.);
#11920=VECTOR('',#43379,1000.);
#11921=VECTOR('',#43382,1000.);
#11922=VECTOR('',#43383,1000.);
#11923=VECTOR('',#43386,1000.);
#11924=VECTOR('',#43387,1000.);
#11925=VECTOR('',#43390,1000.);
#11926=VECTOR('',#43391,1000.);
#11927=VECTOR('',#43394,1000.);
#11928=VECTOR('',#43395,1000.);
#11929=VECTOR('',#43398,1000.);
#11930=VECTOR('',#43399,1000.);
#11931=VECTOR('',#43402,1000.);
#11932=VECTOR('',#43403,1000.);
#11933=VECTOR('',#43406,1000.);
#11934=VECTOR('',#43407,1000.);
#11935=VECTOR('',#43410,1000.);
#11936=VECTOR('',#43411,1000.);
#11937=VECTOR('',#43414,1000.);
#11938=VECTOR('',#43415,1000.);
#11939=VECTOR('',#43418,1000.);
#11940=VECTOR('',#43419,1000.);
#11941=VECTOR('',#43422,1000.);
#11942=VECTOR('',#43425,1000.);
#11943=VECTOR('',#43426,1000.);
#11944=VECTOR('',#43429,1000.);
#11945=VECTOR('',#43430,1000.);
#11946=VECTOR('',#43433,1000.);
#11947=VECTOR('',#43434,1000.);
#11948=VECTOR('',#43437,1000.);
#11949=VECTOR('',#43438,1000.);
#11950=VECTOR('',#43441,1000.);
#11951=VECTOR('',#43442,1000.);
#11952=VECTOR('',#43445,1000.);
#11953=VECTOR('',#43446,1000.);
#11954=VECTOR('',#43449,1000.);
#11955=VECTOR('',#43450,1000.);
#11956=VECTOR('',#43453,1000.);
#11957=VECTOR('',#43454,1000.);
#11958=VECTOR('',#43457,1000.);
#11959=VECTOR('',#43458,1000.);
#11960=VECTOR('',#43461,1000.);
#11961=VECTOR('',#43462,1000.);
#11962=VECTOR('',#43465,1000.);
#11963=VECTOR('',#43466,1000.);
#11964=VECTOR('',#43469,1000.);
#11965=VECTOR('',#43470,1000.);
#11966=VECTOR('',#43473,1000.);
#11967=VECTOR('',#43474,1000.);
#11968=VECTOR('',#43477,1000.);
#11969=VECTOR('',#43478,1000.);
#11970=VECTOR('',#43481,1000.);
#11971=VECTOR('',#43482,1000.);
#11972=VECTOR('',#43485,1000.);
#11973=VECTOR('',#43486,1000.);
#11974=VECTOR('',#43489,1000.);
#11975=VECTOR('',#43490,1000.);
#11976=VECTOR('',#43493,1000.);
#11977=VECTOR('',#43494,1000.);
#11978=VECTOR('',#43497,1000.);
#11979=VECTOR('',#43498,1000.);
#11980=VECTOR('',#43501,1000.);
#11981=VECTOR('',#43502,1000.);
#11982=VECTOR('',#43505,1000.);
#11983=VECTOR('',#43506,1000.);
#11984=VECTOR('',#43509,1000.);
#11985=VECTOR('',#43510,1000.);
#11986=VECTOR('',#43513,1000.);
#11987=VECTOR('',#43514,1000.);
#11988=VECTOR('',#43517,1000.);
#11989=VECTOR('',#43518,1000.);
#11990=VECTOR('',#43519,1000.);
#11991=VECTOR('',#43522,1000.);
#11992=VECTOR('',#43523,1000.);
#11993=VECTOR('',#43526,1000.);
#11994=VECTOR('',#43527,1000.);
#11995=VECTOR('',#43530,1000.);
#11996=VECTOR('',#43531,1000.);
#11997=VECTOR('',#43534,1000.);
#11998=VECTOR('',#43535,1000.);
#11999=VECTOR('',#43538,1000.);
#12000=VECTOR('',#43539,1000.);
#12001=VECTOR('',#43542,1000.);
#12002=VECTOR('',#43543,1000.);
#12003=VECTOR('',#43546,1000.);
#12004=VECTOR('',#43547,1000.);
#12005=VECTOR('',#43550,1000.);
#12006=VECTOR('',#43551,1000.);
#12007=VECTOR('',#43554,1000.);
#12008=VECTOR('',#43555,1000.);
#12009=VECTOR('',#43558,1000.);
#12010=VECTOR('',#43559,1000.);
#12011=VECTOR('',#43562,1000.);
#12012=VECTOR('',#43563,1000.);
#12013=VECTOR('',#43568,1000.);
#12014=VECTOR('',#43569,1000.);
#12015=VECTOR('',#43570,1000.);
#12016=VECTOR('',#43571,1000.);
#12017=VECTOR('',#43574,1000.);
#12018=VECTOR('',#43577,1000.);
#12019=VECTOR('',#43578,1000.);
#12020=VECTOR('',#43579,1000.);
#12021=VECTOR('',#43580,1000.);
#12022=VECTOR('',#43583,1000.);
#12023=VECTOR('',#43584,1000.);
#12024=VECTOR('',#43587,1000.);
#12025=VECTOR('',#43588,1000.);
#12026=VECTOR('',#43591,1000.);
#12027=VECTOR('',#43592,1000.);
#12028=VECTOR('',#43595,1000.);
#12029=VECTOR('',#43596,1000.);
#12030=VECTOR('',#43599,1000.);
#12031=VECTOR('',#43600,1000.);
#12032=VECTOR('',#43603,1000.);
#12033=VECTOR('',#43604,1000.);
#12034=VECTOR('',#43607,1000.);
#12035=VECTOR('',#43608,1000.);
#12036=VECTOR('',#43611,1000.);
#12037=VECTOR('',#43612,1000.);
#12038=VECTOR('',#43615,1000.);
#12039=VECTOR('',#43616,1000.);
#12040=VECTOR('',#43619,1000.);
#12041=VECTOR('',#43620,1000.);
#12042=VECTOR('',#43623,1000.);
#12043=VECTOR('',#43624,1000.);
#12044=VECTOR('',#43627,1000.);
#12045=VECTOR('',#43628,1000.);
#12046=VECTOR('',#43631,1000.);
#12047=VECTOR('',#43632,1000.);
#12048=VECTOR('',#43633,1000.);
#12049=VECTOR('',#43636,1000.);
#12050=VECTOR('',#43637,1000.);
#12051=VECTOR('',#43640,1000.);
#12052=VECTOR('',#43641,1000.);
#12053=VECTOR('',#43644,1000.);
#12054=VECTOR('',#43645,1000.);
#12055=VECTOR('',#43648,1000.);
#12056=VECTOR('',#43649,1000.);
#12057=VECTOR('',#43652,1000.);
#12058=VECTOR('',#43653,1000.);
#12059=VECTOR('',#43656,1000.);
#12060=VECTOR('',#43657,1000.);
#12061=VECTOR('',#43660,1000.);
#12062=VECTOR('',#43661,1000.);
#12063=VECTOR('',#43664,1000.);
#12064=VECTOR('',#43665,1000.);
#12065=VECTOR('',#43668,1000.);
#12066=VECTOR('',#43669,1000.);
#12067=VECTOR('',#43672,1000.);
#12068=VECTOR('',#43673,1000.);
#12069=VECTOR('',#43676,1000.);
#12070=VECTOR('',#43677,1000.);
#12071=VECTOR('',#43680,1000.);
#12072=VECTOR('',#43681,1000.);
#12073=VECTOR('',#43684,1000.);
#12074=VECTOR('',#43685,1000.);
#12075=VECTOR('',#43688,1000.);
#12076=VECTOR('',#43689,1000.);
#12077=VECTOR('',#43692,1000.);
#12078=VECTOR('',#43693,1000.);
#12079=VECTOR('',#43696,1000.);
#12080=VECTOR('',#43697,1000.);
#12081=VECTOR('',#43700,1000.);
#12082=VECTOR('',#43701,1000.);
#12083=VECTOR('',#43704,1000.);
#12084=VECTOR('',#43705,1000.);
#12085=VECTOR('',#43708,1000.);
#12086=VECTOR('',#43709,1000.);
#12087=VECTOR('',#43712,1000.);
#12088=VECTOR('',#43713,1000.);
#12089=VECTOR('',#43716,1000.);
#12090=VECTOR('',#43717,1000.);
#12091=VECTOR('',#43720,1000.);
#12092=VECTOR('',#43721,1000.);
#12093=VECTOR('',#43724,1000.);
#12094=VECTOR('',#43725,1000.);
#12095=VECTOR('',#43728,1000.);
#12096=VECTOR('',#43731,1000.);
#12097=VECTOR('',#43732,1000.);
#12098=VECTOR('',#43735,1000.);
#12099=VECTOR('',#43736,1000.);
#12100=VECTOR('',#43739,1000.);
#12101=VECTOR('',#43740,1000.);
#12102=VECTOR('',#43743,1000.);
#12103=VECTOR('',#43744,1000.);
#12104=VECTOR('',#43747,1000.);
#12105=VECTOR('',#43748,1000.);
#12106=VECTOR('',#43751,1000.);
#12107=VECTOR('',#43752,1000.);
#12108=VECTOR('',#43755,1000.);
#12109=VECTOR('',#43756,1000.);
#12110=VECTOR('',#43759,1000.);
#12111=VECTOR('',#43760,1000.);
#12112=VECTOR('',#43763,1000.);
#12113=VECTOR('',#43764,1000.);
#12114=VECTOR('',#43767,1000.);
#12115=VECTOR('',#43768,1000.);
#12116=VECTOR('',#43771,1000.);
#12117=VECTOR('',#43774,1000.);
#12118=VECTOR('',#43775,1000.);
#12119=VECTOR('',#43776,1000.);
#12120=VECTOR('',#43779,1000.);
#12121=VECTOR('',#43780,1000.);
#12122=VECTOR('',#43781,1000.);
#12123=VECTOR('',#43784,1000.);
#12124=VECTOR('',#43785,1000.);
#12125=VECTOR('',#43786,1000.);
#12126=VECTOR('',#43787,1000.);
#12127=VECTOR('',#43790,1000.);
#12128=VECTOR('',#43791,1000.);
#12129=VECTOR('',#43792,1000.);
#12130=VECTOR('',#43795,1000.);
#12131=VECTOR('',#43796,1000.);
#12132=VECTOR('',#43797,1000.);
#12133=VECTOR('',#43798,1000.);
#12134=VECTOR('',#43801,1000.);
#12135=VECTOR('',#43802,1000.);
#12136=VECTOR('',#43803,1000.);
#12137=VECTOR('',#43806,1000.);
#12138=VECTOR('',#43807,1000.);
#12139=VECTOR('',#43808,1000.);
#12140=VECTOR('',#43811,1000.);
#12141=VECTOR('',#43812,1000.);
#12142=VECTOR('',#43813,1000.);
#12143=VECTOR('',#43814,1000.);
#12144=VECTOR('',#43817,1000.);
#12145=VECTOR('',#43818,1000.);
#12146=VECTOR('',#43819,1000.);
#12147=VECTOR('',#43820,1000.);
#12148=VECTOR('',#43823,1000.);
#12149=VECTOR('',#43824,1000.);
#12150=VECTOR('',#43825,1000.);
#12151=VECTOR('',#43828,1000.);
#12152=VECTOR('',#43829,1000.);
#12153=VECTOR('',#43830,1000.);
#12154=VECTOR('',#43831,1000.);
#12155=VECTOR('',#43834,1000.);
#12156=VECTOR('',#43835,1000.);
#12157=VECTOR('',#43836,1000.);
#12158=VECTOR('',#43837,1000.);
#12159=VECTOR('',#43840,1000.);
#12160=VECTOR('',#43841,1000.);
#12161=VECTOR('',#43842,1000.);
#12162=VECTOR('',#43845,1000.);
#12163=VECTOR('',#43846,1000.);
#12164=VECTOR('',#43847,1000.);
#12165=VECTOR('',#43850,1000.);
#12166=VECTOR('',#43851,1000.);
#12167=VECTOR('',#43852,1000.);
#12168=VECTOR('',#43853,1000.);
#12169=VECTOR('',#43856,1000.);
#12170=VECTOR('',#43857,1000.);
#12171=VECTOR('',#43858,1000.);
#12172=VECTOR('',#43861,1000.);
#12173=VECTOR('',#43862,1000.);
#12174=VECTOR('',#43863,1000.);
#12175=VECTOR('',#43864,1000.);
#12176=VECTOR('',#43867,1000.);
#12177=VECTOR('',#43868,1000.);
#12178=VECTOR('',#43869,1000.);
#12179=VECTOR('',#43872,1000.);
#12180=VECTOR('',#43873,1000.);
#12181=VECTOR('',#43874,1000.);
#12182=VECTOR('',#43877,1000.);
#12183=VECTOR('',#43878,1000.);
#12184=VECTOR('',#43879,1000.);
#12185=VECTOR('',#43880,1000.);
#12186=VECTOR('',#43883,1000.);
#12187=VECTOR('',#43884,1000.);
#12188=VECTOR('',#43885,1000.);
#12189=VECTOR('',#43886,1000.);
#12190=VECTOR('',#43889,1000.);
#12191=VECTOR('',#43890,1000.);
#12192=VECTOR('',#43891,1000.);
#12193=VECTOR('',#43894,1000.);
#12194=VECTOR('',#43895,1000.);
#12195=VECTOR('',#43896,1000.);
#12196=VECTOR('',#43897,1000.);
#12197=VECTOR('',#43900,1000.);
#12198=VECTOR('',#43901,1000.);
#12199=VECTOR('',#43902,1000.);
#12200=VECTOR('',#43903,1000.);
#12201=VECTOR('',#43904,1000.);
#12202=VECTOR('',#43905,1000.);
#12203=VECTOR('',#43916,1000.);
#12204=VECTOR('',#43921,1000.);
#12205=VECTOR('',#43922,1000.);
#12206=VECTOR('',#43925,1000.);
#12207=VECTOR('',#43930,1000.);
#12208=VECTOR('',#43933,1000.);
#12209=VECTOR('',#43938,1000.);
#12210=VECTOR('',#43943,1000.);
#12211=VECTOR('',#43946,1000.);
#12212=VECTOR('',#43951,1000.);
#12213=VECTOR('',#43954,1000.);
#12214=VECTOR('',#43959,1000.);
#12215=VECTOR('',#44030,1000.);
#12216=VECTOR('',#44031,1000.);
#12217=VECTOR('',#44032,1000.);
#12218=VECTOR('',#44033,1000.);
#12219=VECTOR('',#44034,1000.);
#12220=VECTOR('',#44037,1000.);
#12221=VECTOR('',#44038,1000.);
#12222=VECTOR('',#44039,1000.);
#12223=VECTOR('',#44040,1000.);
#12224=VECTOR('',#44043,1000.);
#12225=VECTOR('',#44046,1000.);
#12226=VECTOR('',#44047,1000.);
#12227=VECTOR('',#44048,1000.);
#12228=VECTOR('',#44049,1000.);
#12229=VECTOR('',#44050,1000.);
#12230=VECTOR('',#44051,1000.);
#12231=VECTOR('',#44052,1000.);
#12232=VECTOR('',#44055,1000.);
#12233=VECTOR('',#44058,1000.);
#12234=VECTOR('',#44061,1000.);
#12235=VECTOR('',#44064,1000.);
#12236=VECTOR('',#44067,1000.);
#12237=VECTOR('',#44070,1000.);
#12238=VECTOR('',#44073,1000.);
#12239=VECTOR('',#44074,1000.);
#12240=VECTOR('',#44075,1000.);
#12241=VECTOR('',#44076,1000.);
#12242=VECTOR('',#44077,1000.);
#12243=VECTOR('',#44078,1000.);
#12244=VECTOR('',#44081,1000.);
#12245=VECTOR('',#44084,1000.);
#12246=VECTOR('',#44085,1000.);
#12247=VECTOR('',#44086,1000.);
#12248=VECTOR('',#44087,1000.);
#12249=VECTOR('',#44088,1000.);
#12250=VECTOR('',#44089,1000.);
#12251=VECTOR('',#44092,1000.);
#12252=VECTOR('',#44095,1000.);
#12253=VECTOR('',#44098,1000.);
#12254=VECTOR('',#44101,1000.);
#12255=VECTOR('',#44104,1000.);
#12256=VECTOR('',#44109,10.);
#12257=VECTOR('',#44110,1000.);
#12258=VECTOR('',#44111,10.);
#12259=VECTOR('',#44116,10.);
#12260=VECTOR('',#44117,1000.);
#12261=VECTOR('',#44118,10.);
#12262=VECTOR('',#44123,10.);
#12263=VECTOR('',#44124,1000.);
#12264=VECTOR('',#44125,10.);
#12265=VECTOR('',#44130,10.);
#12266=VECTOR('',#44131,1000.);
#12267=VECTOR('',#44132,10.);
#12268=VECTOR('',#44135,10.);
#12269=VECTOR('',#44136,10.);
#12270=VECTOR('',#44137,10.);
#12271=VECTOR('',#44138,10.);
#12272=VECTOR('',#44145,1000.);
#12273=VECTOR('',#44146,1000.);
#12274=VECTOR('',#44149,1000.);
#12275=VECTOR('',#44152,1000.);
#12276=VECTOR('',#44153,1000.);
#12277=VECTOR('',#44156,1000.);
#12278=VECTOR('',#44157,1000.);
#12279=VECTOR('',#44160,1000.);
#12280=VECTOR('',#44165,10.);
#12281=VECTOR('',#44166,10.);
#12282=VECTOR('',#44167,10.);
#12283=VECTOR('',#44168,10.);
#12284=VECTOR('',#44175,1000.);
#12285=VECTOR('',#44176,1000.);
#12286=VECTOR('',#44179,1000.);
#12287=VECTOR('',#44182,1000.);
#12288=VECTOR('',#44183,1000.);
#12289=VECTOR('',#44186,1000.);
#12290=VECTOR('',#44187,1000.);
#12291=VECTOR('',#44190,1000.);
#12292=VECTOR('',#44211,1000.);
#12293=VECTOR('',#44218,1000.);
#12294=VECTOR('',#44225,1000.);
#12295=VECTOR('',#44228,1000.);
#12296=VECTOR('',#44231,1000.);
#12297=VECTOR('',#44234,1000.);
#12298=VECTOR('',#44237,1000.);
#12299=VECTOR('',#44240,1000.);
#12300=VECTOR('',#44245,1000.);
#12301=VECTOR('',#44248,1000.);
#12302=VECTOR('',#44251,1000.);
#12303=VECTOR('',#44254,1000.);
#12304=VECTOR('',#44257,1000.);
#12305=VECTOR('',#44260,1000.);
#12306=VECTOR('',#44263,1000.);
#12307=VECTOR('',#44264,1000.);
#12308=VECTOR('',#44267,1000.);
#12309=VECTOR('',#44268,1000.);
#12310=VECTOR('',#44277,1000.);
#12311=VECTOR('',#44278,1000.);
#12312=VECTOR('',#44281,1000.);
#12313=VECTOR('',#44282,1000.);
#12314=VECTOR('',#44285,1000.);
#12315=VECTOR('',#44288,1000.);
#12316=VECTOR('',#44311,1000.);
#12317=VECTOR('',#44318,1000.);
#12318=VECTOR('',#44325,1000.);
#12319=VECTOR('',#44328,1000.);
#12320=VECTOR('',#44331,1000.);
#12321=VECTOR('',#44334,1000.);
#12322=VECTOR('',#44337,1000.);
#12323=VECTOR('',#44340,1000.);
#12324=VECTOR('',#44345,1000.);
#12325=VECTOR('',#44348,1000.);
#12326=VECTOR('',#44351,1000.);
#12327=VECTOR('',#44354,1000.);
#12328=VECTOR('',#44357,1000.);
#12329=VECTOR('',#44360,1000.);
#12330=VECTOR('',#44363,1000.);
#12331=VECTOR('',#44364,1000.);
#12332=VECTOR('',#44367,1000.);
#12333=VECTOR('',#44368,1000.);
#12334=VECTOR('',#44377,1000.);
#12335=VECTOR('',#44378,1000.);
#12336=VECTOR('',#44381,1000.);
#12337=VECTOR('',#44382,1000.);
#12338=VECTOR('',#44385,1000.);
#12339=VECTOR('',#44388,1000.);
#12340=VECTOR('',#44411,1000.);
#12341=VECTOR('',#44418,1000.);
#12342=VECTOR('',#44425,1000.);
#12343=VECTOR('',#44428,1000.);
#12344=VECTOR('',#44431,1000.);
#12345=VECTOR('',#44434,1000.);
#12346=VECTOR('',#44437,1000.);
#12347=VECTOR('',#44440,1000.);
#12348=VECTOR('',#44445,1000.);
#12349=VECTOR('',#44448,1000.);
#12350=VECTOR('',#44451,1000.);
#12351=VECTOR('',#44454,1000.);
#12352=VECTOR('',#44457,1000.);
#12353=VECTOR('',#44460,1000.);
#12354=VECTOR('',#44463,1000.);
#12355=VECTOR('',#44464,1000.);
#12356=VECTOR('',#44467,1000.);
#12357=VECTOR('',#44468,1000.);
#12358=VECTOR('',#44477,1000.);
#12359=VECTOR('',#44478,1000.);
#12360=VECTOR('',#44481,1000.);
#12361=VECTOR('',#44482,1000.);
#12362=VECTOR('',#44485,1000.);
#12363=VECTOR('',#44488,1000.);
#12364=VECTOR('',#44511,1000.);
#12365=VECTOR('',#44518,1000.);
#12366=VECTOR('',#44525,1000.);
#12367=VECTOR('',#44528,1000.);
#12368=VECTOR('',#44531,1000.);
#12369=VECTOR('',#44534,1000.);
#12370=VECTOR('',#44537,1000.);
#12371=VECTOR('',#44540,1000.);
#12372=VECTOR('',#44545,1000.);
#12373=VECTOR('',#44548,1000.);
#12374=VECTOR('',#44551,1000.);
#12375=VECTOR('',#44554,1000.);
#12376=VECTOR('',#44557,1000.);
#12377=VECTOR('',#44560,1000.);
#12378=VECTOR('',#44563,1000.);
#12379=VECTOR('',#44564,1000.);
#12380=VECTOR('',#44567,1000.);
#12381=VECTOR('',#44568,1000.);
#12382=VECTOR('',#44577,1000.);
#12383=VECTOR('',#44578,1000.);
#12384=VECTOR('',#44581,1000.);
#12385=VECTOR('',#44582,1000.);
#12386=VECTOR('',#44585,1000.);
#12387=VECTOR('',#44588,1000.);
#12388=VECTOR('',#44601,1000.);
#12389=VECTOR('',#44606,1000.);
#12390=VECTOR('',#44609,1000.);
#12391=VECTOR('',#44614,1000.);
#12392=VECTOR('',#44617,1000.);
#12393=VECTOR('',#44622,1000.);
#12394=VECTOR('',#44627,1000.);
#12395=VECTOR('',#44630,1000.);
#12396=VECTOR('',#44635,1000.);
#12397=VECTOR('',#44636,1000.);
#12398=VECTOR('',#44641,1000.);
#12399=VECTOR('',#44716,1000.);
#12400=VECTOR('',#44717,1000.);
#12401=VECTOR('',#44720,1000.);
#12402=VECTOR('',#44723,1000.);
#12403=VECTOR('',#44724,1000.);
#12404=VECTOR('',#44727,1000.);
#12405=VECTOR('',#44730,1000.);
#12406=VECTOR('',#44731,1000.);
#12407=VECTOR('',#44734,1000.);
#12408=VECTOR('',#44737,1000.);
#12409=VECTOR('',#44740,1000.);
#12410=VECTOR('',#44741,1000.);
#12411=VECTOR('',#44744,1000.);
#12412=VECTOR('',#44745,1000.);
#12413=VECTOR('',#44748,1000.);
#12414=VECTOR('',#44751,1000.);
#12415=VECTOR('',#44752,1000.);
#12416=VECTOR('',#44755,1000.);
#12417=VECTOR('',#44756,1000.);
#12418=VECTOR('',#44757,1000.);
#12419=VECTOR('',#44758,1000.);
#12420=VECTOR('',#44759,1000.);
#12421=VECTOR('',#44760,1000.);
#12422=VECTOR('',#44761,1000.);
#12423=VECTOR('',#44762,1000.);
#12424=VECTOR('',#44763,1000.);
#12425=VECTOR('',#44764,1000.);
#12426=VECTOR('',#44765,1000.);
#12427=VECTOR('',#44766,1000.);
#12428=VECTOR('',#44767,1000.);
#12429=VECTOR('',#44768,1000.);
#12430=VECTOR('',#44769,1000.);
#12431=VECTOR('',#44770,1000.);
#12432=VECTOR('',#44771,1000.);
#12433=VECTOR('',#44772,1000.);
#12434=VECTOR('',#44773,1000.);
#12435=VECTOR('',#44774,1000.);
#12436=VECTOR('',#44775,1000.);
#12437=VECTOR('',#44776,1000.);
#12438=VECTOR('',#44777,1000.);
#12439=VECTOR('',#44778,1000.);
#12440=VECTOR('',#44779,1000.);
#12441=VECTOR('',#44780,1000.);
#12442=VECTOR('',#44781,1000.);
#12443=VECTOR('',#44782,1000.);
#12444=VECTOR('',#44783,1000.);
#12445=VECTOR('',#44784,1000.);
#12446=VECTOR('',#44785,1000.);
#12447=VECTOR('',#44786,1000.);
#12448=VECTOR('',#44787,1000.);
#12449=VECTOR('',#44788,1000.);
#12450=VECTOR('',#44789,1000.);
#12451=VECTOR('',#44790,1000.);
#12452=VECTOR('',#44791,1000.);
#12453=VECTOR('',#44792,1000.);
#12454=VECTOR('',#44793,1000.);
#12455=VECTOR('',#44794,1000.);
#12456=VECTOR('',#44795,1000.);
#12457=VECTOR('',#44796,1000.);
#12458=VECTOR('',#44797,1000.);
#12459=VECTOR('',#44908,1000.);
#12460=VECTOR('',#44909,1000.);
#12461=VECTOR('',#44912,1000.);
#12462=VECTOR('',#44915,1000.);
#12463=VECTOR('',#44918,1000.);
#12464=VECTOR('',#44921,1000.);
#12465=VECTOR('',#44924,1000.);
#12466=VECTOR('',#44927,1000.);
#12467=VECTOR('',#44930,1000.);
#12468=VECTOR('',#44933,1000.);
#12469=VECTOR('',#44936,1000.);
#12470=VECTOR('',#44939,1000.);
#12471=VECTOR('',#44944,1000.);
#12472=VECTOR('',#44945,1000.);
#12473=VECTOR('',#44948,1000.);
#12474=VECTOR('',#44951,1000.);
#12475=VECTOR('',#44964,1000.);
#12476=VECTOR('',#44967,1000.);
#12477=VECTOR('',#44972,1000.);
#12478=VECTOR('',#44975,1000.);
#12479=VECTOR('',#44980,1000.);
#12480=VECTOR('',#44983,1000.);
#12481=VECTOR('',#44988,1000.);
#12482=VECTOR('',#44991,1000.);
#12483=VECTOR('',#44996,1000.);
#12484=VECTOR('',#44999,1000.);
#12485=VECTOR('',#45004,1000.);
#12486=VECTOR('',#45007,1000.);
#12487=VECTOR('',#45012,1000.);
#12488=VECTOR('',#45015,1000.);
#12489=VECTOR('',#45020,1000.);
#12490=VECTOR('',#45023,1000.);
#12491=VECTOR('',#45028,1000.);
#12492=VECTOR('',#45031,1000.);
#12493=VECTOR('',#45036,1000.);
#12494=VECTOR('',#45039,1000.);
#12495=VECTOR('',#45044,1000.);
#12496=VECTOR('',#45047,1000.);
#12497=VECTOR('',#45052,1000.);
#12498=VECTOR('',#45055,1000.);
#12499=VECTOR('',#45060,1000.);
#12500=VECTOR('',#45063,1000.);
#12501=VECTOR('',#45068,1000.);
#12502=VECTOR('',#45071,1000.);
#12503=VECTOR('',#45076,1000.);
#12504=VECTOR('',#45079,1000.);
#12505=VECTOR('',#45084,1000.);
#12506=VECTOR('',#45087,1000.);
#12507=VECTOR('',#45092,1000.);
#12508=VECTOR('',#45095,1000.);
#12509=VECTOR('',#45100,1000.);
#12510=VECTOR('',#45103,1000.);
#12511=VECTOR('',#45108,1000.);
#12512=VECTOR('',#45111,1000.);
#12513=VECTOR('',#45116,1000.);
#12514=VECTOR('',#45119,1000.);
#12515=VECTOR('',#45124,1000.);
#12516=VECTOR('',#45127,1000.);
#12517=VECTOR('',#45132,1000.);
#12518=VECTOR('',#45135,1000.);
#12519=VECTOR('',#45140,1000.);
#12520=VECTOR('',#45143,1000.);
#12521=VECTOR('',#45148,1000.);
#12522=VECTOR('',#45151,1000.);
#12523=VECTOR('',#45156,1000.);
#12524=VECTOR('',#45159,1000.);
#12525=VECTOR('',#45164,1000.);
#12526=VECTOR('',#45167,1000.);
#12527=VECTOR('',#45172,1000.);
#12528=VECTOR('',#45175,1000.);
#12529=VECTOR('',#45180,1000.);
#12530=VECTOR('',#45183,1000.);
#12531=VECTOR('',#45188,1000.);
#12532=VECTOR('',#45191,1000.);
#12533=VECTOR('',#45196,1000.);
#12534=VECTOR('',#45199,1000.);
#12535=VECTOR('',#45204,1000.);
#12536=VECTOR('',#45207,1000.);
#12537=VECTOR('',#45212,1000.);
#12538=VECTOR('',#45215,1000.);
#12539=VECTOR('',#45220,1000.);
#12540=VECTOR('',#45223,1000.);
#12541=VECTOR('',#45228,1000.);
#12542=VECTOR('',#45231,1000.);
#12543=VECTOR('',#45236,1000.);
#12544=VECTOR('',#45239,1000.);
#12545=VECTOR('',#45244,1000.);
#12546=VECTOR('',#45247,1000.);
#12547=VECTOR('',#45252,1000.);
#12548=VECTOR('',#45255,1000.);
#12549=VECTOR('',#45260,1000.);
#12550=VECTOR('',#45263,1000.);
#12551=VECTOR('',#45268,1000.);
#12552=VECTOR('',#45271,1000.);
#12553=VECTOR('',#45276,1000.);
#12554=VECTOR('',#45279,1000.);
#12555=VECTOR('',#45284,1000.);
#12556=VECTOR('',#45287,1000.);
#12557=VECTOR('',#45292,1000.);
#12558=VECTOR('',#45295,1000.);
#12559=VECTOR('',#45300,1000.);
#12560=VECTOR('',#45303,1000.);
#12561=VECTOR('',#45308,1000.);
#12562=VECTOR('',#45311,1000.);
#12563=VECTOR('',#45316,1000.);
#12564=VECTOR('',#45319,1000.);
#12565=VECTOR('',#45324,1000.);
#12566=VECTOR('',#45327,1000.);
#12567=VECTOR('',#45332,1000.);
#12568=VECTOR('',#45335,1000.);
#12569=VECTOR('',#45340,1000.);
#12570=VECTOR('',#45343,1000.);
#12571=VECTOR('',#45348,1000.);
#12572=VECTOR('',#45351,1000.);
#12573=VECTOR('',#45354,1000.);
#12574=VECTOR('',#45357,1000.);
#12575=VECTOR('',#45358,1000.);
#12576=VECTOR('',#45361,1000.);
#12577=VECTOR('',#45366,1000.);
#12578=VECTOR('',#45375,1000.);
#12579=VECTOR('',#45384,1000.);
#12580=VECTOR('',#45387,1000.);
#12581=VECTOR('',#45390,1000.);
#12582=VECTOR('',#45393,1000.);
#12583=VECTOR('',#45412,1000.);
#12584=VECTOR('',#45419,1000.);
#12585=VECTOR('',#45426,1000.);
#12586=VECTOR('',#45429,1000.);
#12587=VECTOR('',#45432,1000.);
#12588=VECTOR('',#45435,1000.);
#12589=VECTOR('',#45438,1000.);
#12590=VECTOR('',#45441,1000.);
#12591=VECTOR('',#45446,1000.);
#12592=VECTOR('',#45449,1000.);
#12593=VECTOR('',#45452,1000.);
#12594=VECTOR('',#45455,1000.);
#12595=VECTOR('',#45458,1000.);
#12596=VECTOR('',#45461,1000.);
#12597=VECTOR('',#45464,1000.);
#12598=VECTOR('',#45465,1000.);
#12599=VECTOR('',#45468,1000.);
#12600=VECTOR('',#45469,1000.);
#12601=VECTOR('',#45478,1000.);
#12602=VECTOR('',#45479,1000.);
#12603=VECTOR('',#45482,1000.);
#12604=VECTOR('',#45483,1000.);
#12605=VECTOR('',#45486,1000.);
#12606=VECTOR('',#45489,1000.);
#12607=VECTOR('',#45512,1000.);
#12608=VECTOR('',#45519,1000.);
#12609=VECTOR('',#45526,1000.);
#12610=VECTOR('',#45529,1000.);
#12611=VECTOR('',#45532,1000.);
#12612=VECTOR('',#45535,1000.);
#12613=VECTOR('',#45538,1000.);
#12614=VECTOR('',#45541,1000.);
#12615=VECTOR('',#45546,1000.);
#12616=VECTOR('',#45549,1000.);
#12617=VECTOR('',#45552,1000.);
#12618=VECTOR('',#45555,1000.);
#12619=VECTOR('',#45558,1000.);
#12620=VECTOR('',#45561,1000.);
#12621=VECTOR('',#45564,1000.);
#12622=VECTOR('',#45565,1000.);
#12623=VECTOR('',#45568,1000.);
#12624=VECTOR('',#45569,1000.);
#12625=VECTOR('',#45578,1000.);
#12626=VECTOR('',#45579,1000.);
#12627=VECTOR('',#45582,1000.);
#12628=VECTOR('',#45583,1000.);
#12629=VECTOR('',#45586,1000.);
#12630=VECTOR('',#45589,1000.);
#12631=VECTOR('',#45598,1000.);
#12632=VECTOR('',#45601,1000.);
#12633=VECTOR('',#45604,1000.);
#12634=VECTOR('',#45607,1000.);
#12635=VECTOR('',#45608,1000.);
#12636=VECTOR('',#45611,1000.);
#12637=VECTOR('',#45616,1000.);
#12638=VECTOR('',#45625,1000.);
#12639=VECTOR('',#45630,1000.);
#12640=VECTOR('',#45633,1000.);
#12641=VECTOR('',#45636,1000.);
#12642=VECTOR('',#45637,1000.);
#12643=VECTOR('',#45638,1000.);
#12644=VECTOR('',#45641,1000.);
#12645=VECTOR('',#45642,1000.);
#12646=VECTOR('',#45643,1000.);
#12647=VECTOR('',#45648,1000.);
#12648=VECTOR('',#45655,1000.);
#12649=VECTOR('',#45660,1000.);
#12650=VECTOR('',#45663,1000.);
#12651=VECTOR('',#45672,0.800100000000001);
#12652=VECTOR('',#45679,0.800100000000001);
#12653=VECTOR('',#45686,0.800100000000001);
#12654=VECTOR('',#45695,1.97294590991864);
#12655=VECTOR('',#45704,1.97294590991864);
#12656=VECTOR('',#45709,1.20015);
#12657=VECTOR('',#45716,1000.);
#12658=VECTOR('',#45719,1000.);
#12659=VECTOR('',#45722,1.20015);
#12660=VECTOR('',#45729,1000.);
#12661=VECTOR('',#45732,1000.);
#12662=VECTOR('',#45735,1000.);
#12663=VECTOR('',#45738,1000.);
#12664=VECTOR('',#45741,1000.);
#12665=VECTOR('',#45744,1000.);
#12666=VECTOR('',#45745,1000.);
#12667=VECTOR('',#45746,1000.);
#12668=VECTOR('',#45747,1000.);
#12669=VECTOR('',#45748,1000.);
#12670=VECTOR('',#45749,1000.);
#12671=VECTOR('',#45750,1000.);
#12672=VECTOR('',#45751,1000.);
#12673=VECTOR('',#45752,1000.);
#12674=VECTOR('',#45753,1000.);
#12675=VECTOR('',#45754,1000.);
#12676=VECTOR('',#45755,1000.);
#12677=VECTOR('',#45756,1000.);
#12678=VECTOR('',#45759,1000.);
#12679=VECTOR('',#45760,1000.);
#12680=VECTOR('',#45761,1000.);
#12681=VECTOR('',#45762,1000.);
#12682=VECTOR('',#45765,1000.);
#12683=VECTOR('',#45766,1000.);
#12684=VECTOR('',#45767,1000.);
#12685=VECTOR('',#45768,1000.);
#12686=VECTOR('',#45769,1000.);
#12687=VECTOR('',#45772,1000.);
#12688=VECTOR('',#45773,1000.);
#12689=VECTOR('',#45774,1000.);
#12690=VECTOR('',#45775,1000.);
#12691=VECTOR('',#45776,1000.);
#12692=VECTOR('',#45779,1000.);
#12693=VECTOR('',#45780,1000.);
#12694=VECTOR('',#45783,1000.);
#12695=VECTOR('',#45784,1000.);
#12696=VECTOR('',#45785,1000.);
#12697=VECTOR('',#45786,1000.);
#12698=VECTOR('',#45787,1000.);
#12699=VECTOR('',#45788,1000.);
#12700=VECTOR('',#45791,1000.);
#12701=VECTOR('',#45792,1000.);
#12702=VECTOR('',#45793,1000.);
#12703=VECTOR('',#45796,1000.);
#12704=VECTOR('',#45797,1000.);
#12705=VECTOR('',#45798,1000.);
#12706=VECTOR('',#45799,1000.);
#12707=VECTOR('',#45800,1000.);
#12708=VECTOR('',#45803,1000.);
#12709=VECTOR('',#45804,1000.);
#12710=VECTOR('',#45807,1000.);
#12711=VECTOR('',#45808,1000.);
#12712=VECTOR('',#45809,1000.);
#12713=VECTOR('',#45810,1000.);
#12714=VECTOR('',#45813,1000.);
#12715=VECTOR('',#45814,1000.);
#12716=VECTOR('',#45815,1000.);
#12717=VECTOR('',#45816,1000.);
#12718=VECTOR('',#45817,1000.);
#12719=VECTOR('',#45820,1000.);
#12720=VECTOR('',#45821,1000.);
#12721=VECTOR('',#45822,1000.);
#12722=VECTOR('',#45823,1000.);
#12723=VECTOR('',#45824,1000.);
#12724=VECTOR('',#45827,1000.);
#12725=VECTOR('',#45828,1000.);
#12726=VECTOR('',#45833,1000.);
#12727=VECTOR('',#45836,1000.);
#12728=VECTOR('',#45839,1000.);
#12729=VECTOR('',#45842,1000.);
#12730=VECTOR('',#45845,1000.);
#12731=VECTOR('',#45848,1000.);
#12732=VECTOR('',#45849,1000.);
#12733=VECTOR('',#45850,1000.);
#12734=VECTOR('',#45851,1000.);
#12735=VECTOR('',#45854,1000.);
#12736=VECTOR('',#45857,1000.);
#12737=VECTOR('',#45860,1000.);
#12738=VECTOR('',#45863,1000.);
#12739=VECTOR('',#45868,1000.);
#12740=VECTOR('',#45871,1000.);
#12741=VECTOR('',#45874,1000.);
#12742=VECTOR('',#45877,1000.);
#12743=VECTOR('',#45880,1000.);
#12744=VECTOR('',#45883,1000.);
#12745=VECTOR('',#45886,1000.);
#12746=VECTOR('',#45889,1000.);
#12747=VECTOR('',#45892,1000.);
#12748=VECTOR('',#45895,1000.);
#12749=VECTOR('',#45898,1000.);
#12750=VECTOR('',#45901,1000.);
#12751=VECTOR('',#45902,1000.);
#12752=VECTOR('',#45905,1000.);
#12753=VECTOR('',#45908,1000.);
#12754=VECTOR('',#45911,1000.);
#12755=VECTOR('',#45914,1000.);
#12756=VECTOR('',#45917,1000.);
#12757=VECTOR('',#45922,1000.);
#12758=VECTOR('',#45925,1000.);
#12759=VECTOR('',#45926,1000.);
#12760=VECTOR('',#45931,1000.);
#12761=VECTOR('',#45932,1000.);
#12762=VECTOR('',#45933,1000.);
#12763=VECTOR('',#45936,1000.);
#12764=VECTOR('',#45939,1000.);
#12765=VECTOR('',#45940,1000.);
#12766=VECTOR('',#45945,1000.);
#12767=VECTOR('',#45946,1000.);
#12768=VECTOR('',#45947,1000.);
#12769=VECTOR('',#45950,1000.);
#12770=VECTOR('',#45955,1000.);
#12771=VECTOR('',#45958,1000.);
#12772=VECTOR('',#45961,1000.);
#12773=VECTOR('',#45966,1000.);
#12774=VECTOR('',#45969,1000.);
#12775=VECTOR('',#45972,1000.);
#12776=VECTOR('',#45973,1000.);
#12777=VECTOR('',#45976,1000.);
#12778=VECTOR('',#45981,1000.);
#12779=VECTOR('',#45986,1000.);
#12780=VECTOR('',#45989,1000.);
#12781=VECTOR('',#46026,1000.);
#12782=VECTOR('',#46027,1000.);
#12783=VECTOR('',#46030,1000.);
#12784=VECTOR('',#46033,1000.);
#12785=VECTOR('',#46036,1000.);
#12786=VECTOR('',#46039,1000.);
#12787=VECTOR('',#46042,1000.);
#12788=VECTOR('',#46045,1000.);
#12789=VECTOR('',#46048,1000.);
#12790=VECTOR('',#46051,1000.);
#12791=VECTOR('',#46054,1000.);
#12792=VECTOR('',#46057,1000.);
#12793=VECTOR('',#46062,1000.);
#12794=VECTOR('',#46063,1000.);
#12795=VECTOR('',#46066,1000.);
#12796=VECTOR('',#46069,1000.);
#12797=VECTOR('',#46072,1000.);
#12798=VECTOR('',#46075,1000.);
#12799=VECTOR('',#46078,1000.);
#12800=VECTOR('',#46081,1000.);
#12801=VECTOR('',#46084,1000.);
#12802=VECTOR('',#46087,1000.);
#12803=VECTOR('',#46090,1000.);
#12804=VECTOR('',#46093,1000.);
#12805=VECTOR('',#46098,1000.);
#12806=VECTOR('',#46101,1000.);
#12807=VECTOR('',#46104,1000.);
#12808=VECTOR('',#46119,1000.);
#12809=VECTOR('',#46120,1000.);
#12810=VECTOR('',#46121,1000.);
#12811=VECTOR('',#46122,1000.);
#12812=VECTOR('',#46123,1000.);
#12813=VECTOR('',#46124,1000.);
#12814=VECTOR('',#46125,1000.);
#12815=VECTOR('',#46126,1000.);
#12816=VECTOR('',#46129,1000.);
#12817=VECTOR('',#46130,1000.);
#12818=VECTOR('',#46133,1000.);
#12819=VECTOR('',#46136,1000.);
#12820=VECTOR('',#46141,1000.);
#12821=VECTOR('',#46142,1000.);
#12822=VECTOR('',#46143,1000.);
#12823=VECTOR('',#46144,1000.);
#12824=VECTOR('',#46147,1000.);
#12825=VECTOR('',#46148,1000.);
#12826=VECTOR('',#46149,1000.);
#12827=VECTOR('',#46152,1000.);
#12828=VECTOR('',#46153,1000.);
#12829=VECTOR('',#46154,1000.);
#12830=VECTOR('',#46157,1000.);
#12831=VECTOR('',#46158,1000.);
#12832=VECTOR('',#46161,1000.);
#12833=VECTOR('',#46164,1000.);
#12834=VECTOR('',#46169,1000.);
#12835=VECTOR('',#46170,1000.);
#12836=VECTOR('',#46171,1000.);
#12837=VECTOR('',#46174,1000.);
#12838=VECTOR('',#46175,1000.);
#12839=VECTOR('',#46178,1000.);
#12840=VECTOR('',#46179,1000.);
#12841=VECTOR('',#46182,1000.);
#12842=VECTOR('',#46185,1000.);
#12843=VECTOR('',#46186,1000.);
#12844=VECTOR('',#46187,1000.);
#12845=VECTOR('',#46188,1000.);
#12846=VECTOR('',#46191,1000.);
#12847=VECTOR('',#46192,1000.);
#12848=VECTOR('',#46193,1000.);
#12849=VECTOR('',#46194,1000.);
#12850=VECTOR('',#46197,1000.);
#12851=VECTOR('',#46198,1000.);
#12852=VECTOR('',#46199,1000.);
#12853=VECTOR('',#46202,1000.);
#12854=VECTOR('',#46203,1000.);
#12855=VECTOR('',#46204,1000.);
#12856=VECTOR('',#46207,1000.);
#12857=VECTOR('',#46208,1000.);
#12858=VECTOR('',#46211,1000.);
#12859=VECTOR('',#46212,1000.);
#12860=VECTOR('',#46219,1000.);
#12861=VECTOR('',#46220,1000.);
#12862=VECTOR('',#46221,1000.);
#12863=VECTOR('',#46222,1000.);
#12864=VECTOR('',#46223,1000.);
#12865=VECTOR('',#46224,1000.);
#12866=VECTOR('',#46225,1000.);
#12867=VECTOR('',#46226,1000.);
#12868=VECTOR('',#46229,1000.);
#12869=VECTOR('',#46230,1000.);
#12870=VECTOR('',#46233,1000.);
#12871=VECTOR('',#46236,1000.);
#12872=VECTOR('',#46241,1000.);
#12873=VECTOR('',#46242,1000.);
#12874=VECTOR('',#46243,1000.);
#12875=VECTOR('',#46244,1000.);
#12876=VECTOR('',#46247,1000.);
#12877=VECTOR('',#46248,1000.);
#12878=VECTOR('',#46249,1000.);
#12879=VECTOR('',#46252,1000.);
#12880=VECTOR('',#46253,1000.);
#12881=VECTOR('',#46254,1000.);
#12882=VECTOR('',#46257,1000.);
#12883=VECTOR('',#46258,1000.);
#12884=VECTOR('',#46261,1000.);
#12885=VECTOR('',#46262,1000.);
#12886=VECTOR('',#46271,1000.);
#12887=VECTOR('',#46272,1000.);
#12888=VECTOR('',#46273,1000.);
#12889=VECTOR('',#46274,1000.);
#12890=VECTOR('',#46277,1000.);
#12891=VECTOR('',#46278,1000.);
#12892=VECTOR('',#46279,1000.);
#12893=VECTOR('',#46280,1000.);
#12894=VECTOR('',#46283,1000.);
#12895=VECTOR('',#46284,1000.);
#12896=VECTOR('',#46287,1000.);
#12897=VECTOR('',#46290,1000.);
#12898=VECTOR('',#46297,1.);
#12899=VECTOR('',#46304,1.);
#12900=VECTOR('',#46311,1000.);
#12901=VECTOR('',#46314,1000.);
#12902=VECTOR('',#46317,1000.);
#12903=VECTOR('',#46318,1000.);
#12904=VECTOR('',#46319,1000.);
#12905=VECTOR('',#46320,1000.);
#12906=VECTOR('',#46323,1000.);
#12907=VECTOR('',#46324,1000.);
#12908=VECTOR('',#46325,1000.);
#12909=VECTOR('',#46326,1000.);
#12910=VECTOR('',#46329,1000.);
#12911=VECTOR('',#46330,1000.);
#12912=VECTOR('',#46331,1000.);
#12913=VECTOR('',#46332,1000.);
#12914=VECTOR('',#46333,1000.);
#12915=VECTOR('',#46336,1000.);
#12916=VECTOR('',#46337,1000.);
#12917=VECTOR('',#46338,1000.);
#12918=VECTOR('',#46339,1000.);
#12919=VECTOR('',#46340,1000.);
#12920=VECTOR('',#46343,1000.);
#12921=VECTOR('',#46344,1000.);
#12922=VECTOR('',#46345,1000.);
#12923=VECTOR('',#46346,1000.);
#12924=VECTOR('',#46349,1000.);
#12925=VECTOR('',#46350,1000.);
#12926=VECTOR('',#46351,1000.);
#12927=VECTOR('',#46352,1000.);
#12928=VECTOR('',#46355,1000.);
#12929=VECTOR('',#46356,1000.);
#12930=VECTOR('',#46357,1000.);
#12931=VECTOR('',#46358,1000.);
#12932=VECTOR('',#46359,1000.);
#12933=VECTOR('',#46362,1000.);
#12934=VECTOR('',#46363,1000.);
#12935=VECTOR('',#46364,1000.);
#12936=VECTOR('',#46365,1000.);
#12937=VECTOR('',#46366,1000.);
#12938=VECTOR('',#46369,1000.);
#12939=VECTOR('',#46370,1000.);
#12940=VECTOR('',#46371,1000.);
#12941=VECTOR('',#46372,1000.);
#12942=VECTOR('',#46373,1000.);
#12943=VECTOR('',#46374,1000.);
#12944=VECTOR('',#46375,1000.);
#12945=VECTOR('',#46376,1000.);
#12946=VECTOR('',#46377,1000.);
#12947=VECTOR('',#46378,1000.);
#12948=VECTOR('',#46379,1000.);
#12949=VECTOR('',#46380,1000.);
#12950=VECTOR('',#46383,1000.);
#12951=VECTOR('',#46384,1000.);
#12952=VECTOR('',#46385,1000.);
#12953=VECTOR('',#46386,1000.);
#12954=VECTOR('',#46387,1000.);
#12955=VECTOR('',#46388,1000.);
#12956=VECTOR('',#46389,1000.);
#12957=VECTOR('',#46390,1000.);
#12958=VECTOR('',#46391,1000.);
#12959=VECTOR('',#46392,1000.);
#12960=VECTOR('',#46393,1000.);
#12961=VECTOR('',#46394,1000.);
#12962=VECTOR('',#46395,1000.);
#12963=VECTOR('',#46396,1000.);
#12964=VECTOR('',#46399,1000.);
#12965=VECTOR('',#46400,1000.);
#12966=VECTOR('',#46401,1000.);
#12967=VECTOR('',#46404,1000.);
#12968=VECTOR('',#46405,1000.);
#12969=VECTOR('',#46408,1000.);
#12970=VECTOR('',#46409,1000.);
#12971=VECTOR('',#46412,1000.);
#12972=VECTOR('',#46415,1000.);
#12973=VECTOR('',#46416,1000.);
#12974=VECTOR('',#46417,1000.);
#12975=VECTOR('',#46418,1000.);
#12976=VECTOR('',#46425,1000.);
#12977=VECTOR('',#46426,1000.);
#12978=VECTOR('',#46427,1000.);
#12979=VECTOR('',#46428,1000.);
#12980=VECTOR('',#46429,1000.);
#12981=VECTOR('',#46430,1000.);
#12982=VECTOR('',#46431,1000.);
#12983=VECTOR('',#46432,1000.);
#12984=VECTOR('',#46433,1000.);
#12985=VECTOR('',#46434,1000.);
#12986=VECTOR('',#46435,1000.);
#12987=VECTOR('',#46436,1000.);
#12988=VECTOR('',#46439,1000.);
#12989=VECTOR('',#46440,1000.);
#12990=VECTOR('',#46447,1000.);
#12991=VECTOR('',#46448,1000.);
#12992=VECTOR('',#46449,1000.);
#12993=VECTOR('',#46450,1000.);
#12994=VECTOR('',#46451,1000.);
#12995=VECTOR('',#46452,1000.);
#12996=VECTOR('',#46453,1000.);
#12997=VECTOR('',#46454,1000.);
#12998=VECTOR('',#46455,1000.);
#12999=VECTOR('',#46456,1000.);
#13000=VECTOR('',#46457,1000.);
#13001=VECTOR('',#46460,1000.);
#13002=VECTOR('',#46463,1000.);
#13003=VECTOR('',#46466,1000.);
#13004=VECTOR('',#46467,1000.);
#13005=VECTOR('',#46470,1000.);
#13006=VECTOR('',#46471,1000.);
#13007=VECTOR('',#46474,1000.);
#13008=VECTOR('',#46475,1000.);
#13009=VECTOR('',#46476,1000.);
#13010=VECTOR('',#46477,1000.);
#13011=VECTOR('',#46478,1000.);
#13012=VECTOR('',#46479,1000.);
#13013=VECTOR('',#46480,1000.);
#13014=VECTOR('',#46485,1000.);
#13015=VECTOR('',#46488,1000.);
#13016=VECTOR('',#46489,1000.);
#13017=VECTOR('',#46492,1000.);
#13018=VECTOR('',#46493,1000.);
#13019=VECTOR('',#46496,1000.);
#13020=VECTOR('',#46497,1000.);
#13021=VECTOR('',#46498,1000.);
#13022=VECTOR('',#46499,1000.);
#13023=VECTOR('',#46500,1000.);
#13024=VECTOR('',#46501,1000.);
#13025=VECTOR('',#46502,1000.);
#13026=VECTOR('',#46509,1000.);
#13027=VECTOR('',#46510,1000.);
#13028=VECTOR('',#46511,1000.);
#13029=VECTOR('',#46516,1000.);
#13030=VECTOR('',#46517,1000.);
#13031=VECTOR('',#46518,1000.);
#13032=VECTOR('',#46521,1000.);
#13033=VECTOR('',#46522,1000.);
#13034=VECTOR('',#46527,1000.);
#13035=VECTOR('',#46528,1000.);
#13036=VECTOR('',#46529,1000.);
#13037=VECTOR('',#46534,1000.);
#13038=VECTOR('',#46535,1000.);
#13039=VECTOR('',#46536,1000.);
#13040=VECTOR('',#46539,1000.);
#13041=VECTOR('',#46540,1000.);
#13042=VECTOR('',#46555,1000.);
#13043=VECTOR('',#46556,1000.);
#13044=VECTOR('',#46559,1000.);
#13045=VECTOR('',#46560,1000.);
#13046=VECTOR('',#46563,1000.);
#13047=VECTOR('',#46568,1000.);
#13048=VECTOR('',#46573,1000.);
#13049=VECTOR('',#46578,1000.);
#13050=VECTOR('',#46583,1000.);
#13051=VECTOR('',#46584,1000.);
#13052=VECTOR('',#46587,1000.);
#13053=VECTOR('',#46590,1000.);
#13054=VECTOR('',#46633,1000.);
#13055=VECTOR('',#46634,1000.);
#13056=VECTOR('',#46635,1000.);
#13057=VECTOR('',#46636,1000.);
#13058=VECTOR('',#46637,1000.);
#13059=VECTOR('',#46638,1000.);
#13060=VECTOR('',#46639,1000.);
#13061=VECTOR('',#46640,1000.);
#13062=VECTOR('',#46641,1000.);
#13063=VECTOR('',#46642,1000.);
#13064=VECTOR('',#46643,1000.);
#13065=VECTOR('',#46644,1000.);
#13066=VECTOR('',#46647,1000.);
#13067=VECTOR('',#46648,1000.);
#13068=VECTOR('',#46649,1000.);
#13069=VECTOR('',#46650,1000.);
#13070=VECTOR('',#46651,1000.);
#13071=VECTOR('',#46652,1000.);
#13072=VECTOR('',#46653,1000.);
#13073=VECTOR('',#46654,1000.);
#13074=VECTOR('',#46655,1000.);
#13075=VECTOR('',#46656,1000.);
#13076=VECTOR('',#46657,1000.);
#13077=VECTOR('',#46658,1000.);
#13078=VECTOR('',#46661,1000.);
#13079=VECTOR('',#46662,1000.);
#13080=VECTOR('',#46665,1000.);
#13081=VECTOR('',#46666,1000.);
#13082=VECTOR('',#46669,1000.);
#13083=VECTOR('',#46670,1000.);
#13084=VECTOR('',#46673,1000.);
#13085=VECTOR('',#46674,1000.);
#13086=VECTOR('',#46679,1000.);
#13087=VECTOR('',#46680,1000.);
#13088=VECTOR('',#46683,1000.);
#13089=VECTOR('',#46686,1000.);
#13090=VECTOR('',#46689,1000.);
#13091=VECTOR('',#46698,1000.);
#13092=VECTOR('',#46703,1000.);
#13093=VECTOR('',#46706,1000.);
#13094=VECTOR('',#46711,1000.);
#13095=VECTOR('',#46716,1000.);
#13096=VECTOR('',#46723,1000.);
#13097=VECTOR('',#46726,1000.);
#13098=VECTOR('',#46731,1000.);
#13099=VECTOR('',#46734,1000.);
#13100=VECTOR('',#46737,1000.);
#13101=VECTOR('',#46738,1000.);
#13102=VECTOR('',#46739,1000.);
#13103=VECTOR('',#46740,1000.);
#13104=VECTOR('',#46745,1000.);
#13105=VECTOR('',#46748,1000.);
#13106=VECTOR('',#46751,1000.);
#13107=VECTOR('',#46752,1000.);
#13108=VECTOR('',#46755,1000.);
#13109=VECTOR('',#46756,1000.);
#13110=VECTOR('',#46757,1000.);
#13111=VECTOR('',#46758,1000.);
#13112=VECTOR('',#46761,1000.);
#13113=VECTOR('',#46764,1000.);
#13114=VECTOR('',#46765,1000.);
#13115=VECTOR('',#46766,1000.);
#13116=VECTOR('',#46775,1000.);
#13117=VECTOR('',#46784,1000.);
#13118=VECTOR('',#46789,1000.);
#13119=VECTOR('',#46792,1000.);
#13120=VECTOR('',#46797,1000.);
#13121=VECTOR('',#46802,1000.);
#13122=VECTOR('',#46809,1000.);
#13123=VECTOR('',#46812,1000.);
#13124=VECTOR('',#46817,1000.);
#13125=VECTOR('',#46820,1000.);
#13126=VECTOR('',#46823,1000.);
#13127=VECTOR('',#46824,1000.);
#13128=VECTOR('',#46825,1000.);
#13129=VECTOR('',#46826,1000.);
#13130=VECTOR('',#46831,1000.);
#13131=VECTOR('',#46834,1000.);
#13132=VECTOR('',#46837,1000.);
#13133=VECTOR('',#46838,1000.);
#13134=VECTOR('',#46841,1000.);
#13135=VECTOR('',#46842,1000.);
#13136=VECTOR('',#46843,1000.);
#13137=VECTOR('',#46844,1000.);
#13138=VECTOR('',#46847,1000.);
#13139=VECTOR('',#46850,1000.);
#13140=VECTOR('',#46851,1000.);
#13141=VECTOR('',#46852,1000.);
#13142=VECTOR('',#46861,1000.);
#13143=VECTOR('',#46862,1000.);
#13144=VECTOR('',#46863,1000.);
#13145=VECTOR('',#46864,1000.);
#13146=VECTOR('',#46865,1000.);
#13147=VECTOR('',#46866,1000.);
#13148=VECTOR('',#46867,1000.);
#13149=VECTOR('',#46868,1000.);
#13150=VECTOR('',#46869,1000.);
#13151=VECTOR('',#46870,1000.);
#13152=VECTOR('',#46871,1000.);
#13153=VECTOR('',#46872,1000.);
#13154=VECTOR('',#46873,1000.);
#13155=VECTOR('',#46874,1000.);
#13156=VECTOR('',#46875,1000.);
#13157=VECTOR('',#46876,1000.);
#13158=VECTOR('',#46877,1000.);
#13159=VECTOR('',#46878,1000.);
#13160=VECTOR('',#46879,1000.);
#13161=VECTOR('',#46880,1000.);
#13162=VECTOR('',#46881,1000.);
#13163=VECTOR('',#46882,1000.);
#13164=VECTOR('',#46883,1000.);
#13165=VECTOR('',#46884,1000.);
#13166=VECTOR('',#46885,1000.);
#13167=VECTOR('',#46886,1000.);
#13168=VECTOR('',#46887,1000.);
#13169=VECTOR('',#46888,1000.);
#13170=VECTOR('',#46889,1000.);
#13171=VECTOR('',#46890,1000.);
#13172=VECTOR('',#46891,1000.);
#13173=VECTOR('',#46892,1000.);
#13174=VECTOR('',#46893,1000.);
#13175=VECTOR('',#46894,1000.);
#13176=VECTOR('',#46895,1000.);
#13177=VECTOR('',#46896,1000.);
#13178=VECTOR('',#46897,1000.);
#13179=VECTOR('',#46898,1000.);
#13180=VECTOR('',#46899,1000.);
#13181=VECTOR('',#46900,1000.);
#13182=VECTOR('',#46901,1000.);
#13183=VECTOR('',#46902,1000.);
#13184=VECTOR('',#46903,1000.);
#13185=VECTOR('',#46904,1000.);
#13186=VECTOR('',#46905,1000.);
#13187=VECTOR('',#46906,1000.);
#13188=VECTOR('',#46907,1000.);
#13189=VECTOR('',#46908,1000.);
#13190=VECTOR('',#46909,1000.);
#13191=VECTOR('',#46910,1000.);
#13192=VECTOR('',#46911,1000.);
#13193=VECTOR('',#46912,1000.);
#13194=VECTOR('',#46913,1000.);
#13195=VECTOR('',#46914,1000.);
#13196=VECTOR('',#46915,1000.);
#13197=VECTOR('',#46916,1000.);
#13198=VECTOR('',#46917,1000.);
#13199=VECTOR('',#46918,1000.);
#13200=VECTOR('',#46919,1000.);
#13201=VECTOR('',#46920,1000.);
#13202=VECTOR('',#46921,1000.);
#13203=VECTOR('',#46922,1000.);
#13204=VECTOR('',#46923,1000.);
#13205=VECTOR('',#46924,1000.);
#13206=VECTOR('',#46925,1000.);
#13207=VECTOR('',#46926,1000.);
#13208=VECTOR('',#46927,1000.);
#13209=VECTOR('',#46928,1000.);
#13210=VECTOR('',#46929,1000.);
#13211=VECTOR('',#46930,1000.);
#13212=VECTOR('',#46931,1000.);
#13213=VECTOR('',#46932,1000.);
#13214=VECTOR('',#46933,1000.);
#13215=VECTOR('',#46934,1000.);
#13216=VECTOR('',#46935,1000.);
#13217=VECTOR('',#46936,1000.);
#13218=VECTOR('',#46937,1000.);
#13219=VECTOR('',#46938,1000.);
#13220=VECTOR('',#46939,1000.);
#13221=VECTOR('',#46940,1000.);
#13222=VECTOR('',#46941,1000.);
#13223=VECTOR('',#46942,1000.);
#13224=VECTOR('',#46943,1000.);
#13225=VECTOR('',#46944,1000.);
#13226=VECTOR('',#46945,1000.);
#13227=VECTOR('',#46946,1000.);
#13228=VECTOR('',#46947,1000.);
#13229=VECTOR('',#46948,1000.);
#13230=VECTOR('',#46949,1000.);
#13231=VECTOR('',#46950,1000.);
#13232=VECTOR('',#46951,1000.);
#13233=VECTOR('',#46952,1000.);
#13234=VECTOR('',#46953,1000.);
#13235=VECTOR('',#46954,1000.);
#13236=VECTOR('',#46955,1000.);
#13237=VECTOR('',#46956,1000.);
#13238=VECTOR('',#46957,1000.);
#13239=VECTOR('',#46958,1000.);
#13240=VECTOR('',#46959,1000.);
#13241=VECTOR('',#46960,1000.);
#13242=VECTOR('',#46961,1000.);
#13243=VECTOR('',#46962,1000.);
#13244=VECTOR('',#46963,1000.);
#13245=VECTOR('',#46964,1000.);
#13246=VECTOR('',#46965,1000.);
#13247=VECTOR('',#46966,1000.);
#13248=VECTOR('',#46967,1000.);
#13249=VECTOR('',#46968,1000.);
#13250=VECTOR('',#46969,1000.);
#13251=VECTOR('',#46970,1000.);
#13252=VECTOR('',#46971,1000.);
#13253=VECTOR('',#46972,1000.);
#13254=VECTOR('',#46973,1000.);
#13255=VECTOR('',#46974,1000.);
#13256=VECTOR('',#46975,1000.);
#13257=VECTOR('',#46976,1000.);
#13258=VECTOR('',#46977,1000.);
#13259=VECTOR('',#46978,1000.);
#13260=VECTOR('',#46979,1000.);
#13261=VECTOR('',#46980,1000.);
#13262=VECTOR('',#46981,1000.);
#13263=VECTOR('',#46982,1000.);
#13264=VECTOR('',#46983,1000.);
#13265=VECTOR('',#46984,1000.);
#13266=VECTOR('',#46985,1000.);
#13267=VECTOR('',#46986,1000.);
#13268=VECTOR('',#46987,1000.);
#13269=VECTOR('',#46988,1000.);
#13270=VECTOR('',#46989,1000.);
#13271=VECTOR('',#46990,1000.);
#13272=VECTOR('',#46991,1000.);
#13273=VECTOR('',#46992,1000.);
#13274=VECTOR('',#46993,1000.);
#13275=VECTOR('',#46994,1000.);
#13276=VECTOR('',#46995,1000.);
#13277=VECTOR('',#46996,1000.);
#13278=VECTOR('',#46997,1000.);
#13279=VECTOR('',#46998,1000.);
#13280=VECTOR('',#46999,1000.);
#13281=VECTOR('',#47000,1000.);
#13282=VECTOR('',#47001,1000.);
#13283=VECTOR('',#47002,1000.);
#13284=VECTOR('',#47003,1000.);
#13285=VECTOR('',#47004,1000.);
#13286=VECTOR('',#47005,1000.);
#13287=VECTOR('',#47006,1000.);
#13288=VECTOR('',#47007,1000.);
#13289=VECTOR('',#47008,1000.);
#13290=VECTOR('',#47009,1000.);
#13291=VECTOR('',#47010,1000.);
#13292=VECTOR('',#47011,1000.);
#13293=VECTOR('',#47012,1000.);
#13294=VECTOR('',#47013,1000.);
#13295=VECTOR('',#47014,1000.);
#13296=VECTOR('',#47015,1000.);
#13297=VECTOR('',#47016,1000.);
#13298=VECTOR('',#47017,1000.);
#13299=VECTOR('',#47018,1000.);
#13300=VECTOR('',#47019,1000.);
#13301=VECTOR('',#47020,1000.);
#13302=VECTOR('',#47021,1000.);
#13303=VECTOR('',#47022,1000.);
#13304=VECTOR('',#47023,1000.);
#13305=VECTOR('',#47024,1000.);
#13306=VECTOR('',#47025,1000.);
#13307=VECTOR('',#47026,1000.);
#13308=VECTOR('',#47027,1000.);
#13309=VECTOR('',#47028,1000.);
#13310=VECTOR('',#47029,1000.);
#13311=VECTOR('',#47030,1000.);
#13312=VECTOR('',#47031,1000.);
#13313=VECTOR('',#47032,1000.);
#13314=VECTOR('',#47033,1000.);
#13315=VECTOR('',#47034,1000.);
#13316=VECTOR('',#47035,1000.);
#13317=VECTOR('',#47036,1000.);
#13318=VECTOR('',#47037,1000.);
#13319=VECTOR('',#47038,1000.);
#13320=VECTOR('',#47039,1000.);
#13321=VECTOR('',#47040,1000.);
#13322=VECTOR('',#47041,1000.);
#13323=VECTOR('',#47042,1000.);
#13324=VECTOR('',#47043,1000.);
#13325=VECTOR('',#47044,1000.);
#13326=VECTOR('',#47045,1000.);
#13327=VECTOR('',#47046,1000.);
#13328=VECTOR('',#47047,1000.);
#13329=VECTOR('',#47048,1000.);
#13330=VECTOR('',#47049,1000.);
#13331=VECTOR('',#47050,1000.);
#13332=VECTOR('',#47051,1000.);
#13333=VECTOR('',#47052,1000.);
#13334=VECTOR('',#47053,1000.);
#13335=VECTOR('',#47054,1000.);
#13336=VECTOR('',#47055,1000.);
#13337=VECTOR('',#47056,1000.);
#13338=VECTOR('',#47057,1000.);
#13339=VECTOR('',#47058,1000.);
#13340=VECTOR('',#47059,1000.);
#13341=VECTOR('',#47060,1000.);
#13342=VECTOR('',#47061,1000.);
#13343=VECTOR('',#47062,1000.);
#13344=VECTOR('',#47063,1000.);
#13345=VECTOR('',#47064,1000.);
#13346=VECTOR('',#47065,1000.);
#13347=VECTOR('',#47066,1000.);
#13348=VECTOR('',#47067,1000.);
#13349=VECTOR('',#47068,1000.);
#13350=VECTOR('',#47069,1000.);
#13351=VECTOR('',#47070,1000.);
#13352=VECTOR('',#47071,1000.);
#13353=VECTOR('',#47072,1000.);
#13354=VECTOR('',#47073,1000.);
#13355=VECTOR('',#47074,1000.);
#13356=VECTOR('',#47075,1000.);
#13357=VECTOR('',#47076,1000.);
#13358=VECTOR('',#47077,1000.);
#13359=VECTOR('',#47078,1000.);
#13360=VECTOR('',#47079,1000.);
#13361=VECTOR('',#47080,1000.);
#13362=VECTOR('',#47081,1000.);
#13363=VECTOR('',#47082,1000.);
#13364=VECTOR('',#47083,1000.);
#13365=VECTOR('',#47084,1000.);
#13366=VECTOR('',#47085,1000.);
#13367=VECTOR('',#47086,1000.);
#13368=VECTOR('',#47087,1000.);
#13369=VECTOR('',#47088,1000.);
#13370=VECTOR('',#47089,1000.);
#13371=VECTOR('',#47090,1000.);
#13372=VECTOR('',#47091,1000.);
#13373=VECTOR('',#47092,1000.);
#13374=VECTOR('',#47093,1000.);
#13375=VECTOR('',#47094,1000.);
#13376=VECTOR('',#47095,1000.);
#13377=VECTOR('',#47096,1000.);
#13378=VECTOR('',#47097,1000.);
#13379=VECTOR('',#47098,1000.);
#13380=VECTOR('',#47099,1000.);
#13381=VECTOR('',#47100,1000.);
#13382=VECTOR('',#47101,1000.);
#13383=VECTOR('',#47102,1000.);
#13384=VECTOR('',#47103,1000.);
#13385=VECTOR('',#47104,1000.);
#13386=VECTOR('',#47105,1000.);
#13387=VECTOR('',#47106,1000.);
#13388=VECTOR('',#47107,1000.);
#13389=VECTOR('',#47108,1000.);
#13390=VECTOR('',#47109,1000.);
#13391=VECTOR('',#47110,1000.);
#13392=VECTOR('',#47111,1000.);
#13393=VECTOR('',#47112,1000.);
#13394=VECTOR('',#47113,1000.);
#13395=VECTOR('',#47114,1000.);
#13396=VECTOR('',#47115,1000.);
#13397=VECTOR('',#47116,1000.);
#13398=VECTOR('',#47117,1000.);
#13399=VECTOR('',#47118,1000.);
#13400=VECTOR('',#47119,1000.);
#13401=VECTOR('',#47120,1000.);
#13402=VECTOR('',#47121,1000.);
#13403=VECTOR('',#47122,1000.);
#13404=VECTOR('',#47123,1000.);
#13405=VECTOR('',#47124,1000.);
#13406=VECTOR('',#47125,1000.);
#13407=VECTOR('',#47126,1000.);
#13408=VECTOR('',#47127,1000.);
#13409=VECTOR('',#47128,1000.);
#13410=VECTOR('',#47129,1000.);
#13411=VECTOR('',#47130,1000.);
#13412=VECTOR('',#47131,1000.);
#13413=VECTOR('',#47132,1000.);
#13414=VECTOR('',#47133,1000.);
#13415=VECTOR('',#47134,1000.);
#13416=VECTOR('',#47135,1000.);
#13417=VECTOR('',#47136,1000.);
#13418=VECTOR('',#47137,1000.);
#13419=VECTOR('',#47138,1000.);
#13420=VECTOR('',#47139,1000.);
#13421=VECTOR('',#47140,1000.);
#13422=VECTOR('',#47141,1000.);
#13423=VECTOR('',#47142,1000.);
#13424=VECTOR('',#47143,1000.);
#13425=VECTOR('',#47144,1000.);
#13426=VECTOR('',#47145,1000.);
#13427=VECTOR('',#47146,1000.);
#13428=VECTOR('',#47147,1000.);
#13429=VECTOR('',#47148,1000.);
#13430=VECTOR('',#47149,1000.);
#13431=VECTOR('',#47150,1000.);
#13432=VECTOR('',#47151,1000.);
#13433=VECTOR('',#47152,1000.);
#13434=VECTOR('',#47153,1000.);
#13435=VECTOR('',#47154,1000.);
#13436=VECTOR('',#47155,1000.);
#13437=VECTOR('',#47156,1000.);
#13438=VECTOR('',#47157,1000.);
#13439=VECTOR('',#47158,1000.);
#13440=VECTOR('',#47159,1000.);
#13441=VECTOR('',#47160,1000.);
#13442=VECTOR('',#47161,1000.);
#13443=VECTOR('',#47162,1000.);
#13444=VECTOR('',#47163,1000.);
#13445=VECTOR('',#47164,1000.);
#13446=VECTOR('',#47165,1000.);
#13447=VECTOR('',#47166,1000.);
#13448=VECTOR('',#47167,1000.);
#13449=VECTOR('',#47168,1000.);
#13450=VECTOR('',#47169,1000.);
#13451=VECTOR('',#47170,1000.);
#13452=VECTOR('',#47171,1000.);
#13453=VECTOR('',#47172,1000.);
#13454=VECTOR('',#47173,1000.);
#13455=VECTOR('',#47174,1000.);
#13456=VECTOR('',#47175,1000.);
#13457=VECTOR('',#47176,1000.);
#13458=VECTOR('',#47177,1000.);
#13459=VECTOR('',#47178,1000.);
#13460=VECTOR('',#47179,1000.);
#13461=VECTOR('',#47180,1000.);
#13462=VECTOR('',#47181,1000.);
#13463=VECTOR('',#47182,1000.);
#13464=VECTOR('',#47183,1000.);
#13465=VECTOR('',#47184,1000.);
#13466=VECTOR('',#47185,1000.);
#13467=VECTOR('',#47186,1000.);
#13468=VECTOR('',#47187,1000.);
#13469=VECTOR('',#47188,1000.);
#13470=VECTOR('',#47189,1000.);
#13471=VECTOR('',#47190,1000.);
#13472=VECTOR('',#47191,1000.);
#13473=VECTOR('',#47192,1000.);
#13474=VECTOR('',#47193,1000.);
#13475=VECTOR('',#47194,1000.);
#13476=VECTOR('',#47195,1000.);
#13477=VECTOR('',#47196,1000.);
#13478=VECTOR('',#47197,1000.);
#13479=VECTOR('',#47198,1000.);
#13480=VECTOR('',#47199,1000.);
#13481=VECTOR('',#47200,1000.);
#13482=VECTOR('',#47201,1000.);
#13483=VECTOR('',#47202,1000.);
#13484=VECTOR('',#47203,1000.);
#13485=VECTOR('',#47204,1000.);
#13486=VECTOR('',#47205,1000.);
#13487=VECTOR('',#47206,1000.);
#13488=VECTOR('',#47207,1000.);
#13489=VECTOR('',#47208,1000.);
#13490=VECTOR('',#47209,1000.);
#13491=VECTOR('',#47210,1000.);
#13492=VECTOR('',#47211,1000.);
#13493=VECTOR('',#47212,1000.);
#13494=VECTOR('',#47213,1000.);
#13495=VECTOR('',#47214,1000.);
#13496=VECTOR('',#47215,1000.);
#13497=VECTOR('',#47216,1000.);
#13498=VECTOR('',#47217,1000.);
#13499=VECTOR('',#47218,1000.);
#13500=VECTOR('',#47219,1000.);
#13501=VECTOR('',#47220,1000.);
#13502=VECTOR('',#47221,1000.);
#13503=VECTOR('',#47222,1000.);
#13504=VECTOR('',#47223,1000.);
#13505=VECTOR('',#47224,1000.);
#13506=VECTOR('',#47225,1000.);
#13507=VECTOR('',#47226,1000.);
#13508=VECTOR('',#47227,1000.);
#13509=VECTOR('',#47228,1000.);
#13510=VECTOR('',#47229,1000.);
#13511=VECTOR('',#47230,1000.);
#13512=VECTOR('',#47231,1000.);
#13513=VECTOR('',#47232,1000.);
#13514=VECTOR('',#47233,1000.);
#13515=VECTOR('',#47234,1000.);
#13516=VECTOR('',#47235,1000.);
#13517=VECTOR('',#47236,1000.);
#13518=VECTOR('',#47237,1000.);
#13519=VECTOR('',#47238,1000.);
#13520=VECTOR('',#47239,1000.);
#13521=VECTOR('',#47240,1000.);
#13522=VECTOR('',#47241,1000.);
#13523=VECTOR('',#47242,1000.);
#13524=VECTOR('',#47243,1000.);
#13525=VECTOR('',#47244,1000.);
#13526=VECTOR('',#47245,1000.);
#13527=VECTOR('',#47246,1000.);
#13528=VECTOR('',#47247,1000.);
#13529=VECTOR('',#47248,1000.);
#13530=VECTOR('',#47249,1000.);
#13531=VECTOR('',#47250,1000.);
#13532=VECTOR('',#47251,1000.);
#13533=VECTOR('',#47252,1000.);
#13534=VECTOR('',#47253,1000.);
#13535=VECTOR('',#47254,1000.);
#13536=VECTOR('',#47255,1000.);
#13537=VECTOR('',#47256,1000.);
#13538=VECTOR('',#47257,1000.);
#13539=VECTOR('',#47258,1000.);
#13540=VECTOR('',#47259,1000.);
#13541=VECTOR('',#47260,1000.);
#13542=VECTOR('',#47261,1000.);
#13543=VECTOR('',#47262,1000.);
#13544=VECTOR('',#47263,1000.);
#13545=VECTOR('',#47264,1000.);
#13546=VECTOR('',#47265,1000.);
#13547=VECTOR('',#47266,1000.);
#13548=VECTOR('',#47267,1000.);
#13549=VECTOR('',#47268,1000.);
#13550=VECTOR('',#47269,1000.);
#13551=VECTOR('',#47270,1000.);
#13552=VECTOR('',#47271,1000.);
#13553=VECTOR('',#47272,1000.);
#13554=VECTOR('',#47273,1000.);
#13555=VECTOR('',#47274,1000.);
#13556=VECTOR('',#47275,1000.);
#13557=VECTOR('',#47276,1000.);
#13558=VECTOR('',#47277,1000.);
#13559=VECTOR('',#47278,1000.);
#13560=VECTOR('',#47279,1000.);
#13561=VECTOR('',#47280,1000.);
#13562=VECTOR('',#47281,1000.);
#13563=VECTOR('',#47282,1000.);
#13564=VECTOR('',#47283,1000.);
#13565=VECTOR('',#47284,1000.);
#13566=VECTOR('',#47285,1000.);
#13567=VECTOR('',#47286,1000.);
#13568=VECTOR('',#47287,1000.);
#13569=VECTOR('',#47288,1000.);
#13570=VECTOR('',#47289,1000.);
#13571=VECTOR('',#47290,1000.);
#13572=VECTOR('',#47291,1000.);
#13573=VECTOR('',#47292,1000.);
#13574=VECTOR('',#47293,1000.);
#13575=VECTOR('',#47294,1000.);
#13576=VECTOR('',#47295,1000.);
#13577=VECTOR('',#47296,1000.);
#13578=VECTOR('',#47297,1000.);
#13579=VECTOR('',#47298,1000.);
#13580=VECTOR('',#47299,1000.);
#13581=VECTOR('',#47300,1000.);
#13582=VECTOR('',#47301,1000.);
#13583=VECTOR('',#47302,1000.);
#13584=VECTOR('',#47303,1000.);
#13585=VECTOR('',#47304,1000.);
#13586=VECTOR('',#47305,1000.);
#13587=VECTOR('',#47306,1000.);
#13588=VECTOR('',#47307,1000.);
#13589=VECTOR('',#47308,1000.);
#13590=VECTOR('',#47309,1000.);
#13591=VECTOR('',#47310,1000.);
#13592=VECTOR('',#47311,1000.);
#13593=VECTOR('',#47312,1000.);
#13594=VECTOR('',#47313,1000.);
#13595=VECTOR('',#47314,1000.);
#13596=VECTOR('',#47315,1000.);
#13597=VECTOR('',#47316,1000.);
#13598=VECTOR('',#47317,1000.);
#13599=VECTOR('',#47318,1000.);
#13600=VECTOR('',#47319,1000.);
#13601=VECTOR('',#47320,1000.);
#13602=VECTOR('',#47321,1000.);
#13603=VECTOR('',#47322,1000.);
#13604=VECTOR('',#47323,1000.);
#13605=VECTOR('',#47324,1000.);
#13606=VECTOR('',#47325,1000.);
#13607=VECTOR('',#47326,1000.);
#13608=VECTOR('',#47327,1000.);
#13609=VECTOR('',#47328,1000.);
#13610=VECTOR('',#47329,1000.);
#13611=VECTOR('',#47330,1000.);
#13612=VECTOR('',#47331,1000.);
#13613=VECTOR('',#47332,1000.);
#13614=VECTOR('',#47333,1000.);
#13615=VECTOR('',#47334,1000.);
#13616=VECTOR('',#47335,1000.);
#13617=VECTOR('',#47336,1000.);
#13618=VECTOR('',#47337,1000.);
#13619=VECTOR('',#47338,1000.);
#13620=VECTOR('',#47339,1000.);
#13621=VECTOR('',#47340,1000.);
#13622=VECTOR('',#47341,1000.);
#13623=VECTOR('',#47342,1000.);
#13624=VECTOR('',#47343,1000.);
#13625=VECTOR('',#47344,1000.);
#13626=VECTOR('',#47345,1000.);
#13627=VECTOR('',#47346,1000.);
#13628=VECTOR('',#47347,1000.);
#13629=VECTOR('',#47348,1000.);
#13630=VECTOR('',#47349,1000.);
#13631=VECTOR('',#47350,1000.);
#13632=VECTOR('',#47351,1000.);
#13633=VECTOR('',#47352,1000.);
#13634=VECTOR('',#47353,1000.);
#13635=VECTOR('',#47354,1000.);
#13636=VECTOR('',#47355,1000.);
#13637=VECTOR('',#47356,1000.);
#13638=VECTOR('',#47357,1000.);
#13639=VECTOR('',#47358,1000.);
#13640=VECTOR('',#47359,1000.);
#13641=VECTOR('',#47360,1000.);
#13642=VECTOR('',#47361,1000.);
#13643=VECTOR('',#47362,1000.);
#13644=VECTOR('',#47363,1000.);
#13645=VECTOR('',#47364,1000.);
#13646=VECTOR('',#47365,1000.);
#13647=VECTOR('',#47366,1000.);
#13648=VECTOR('',#47367,1000.);
#13649=VECTOR('',#47368,1000.);
#13650=VECTOR('',#47369,1000.);
#13651=VECTOR('',#47370,1000.);
#13652=VECTOR('',#47371,1000.);
#13653=VECTOR('',#47372,1000.);
#13654=VECTOR('',#47373,1000.);
#13655=VECTOR('',#47374,1000.);
#13656=VECTOR('',#47375,1000.);
#13657=VECTOR('',#47376,1000.);
#13658=VECTOR('',#47377,1000.);
#13659=VECTOR('',#47378,1000.);
#13660=VECTOR('',#47379,1000.);
#13661=VECTOR('',#47380,1000.);
#13662=VECTOR('',#47381,1000.);
#13663=VECTOR('',#47382,1000.);
#13664=VECTOR('',#47383,1000.);
#13665=VECTOR('',#47384,1000.);
#13666=VECTOR('',#47385,1000.);
#13667=VECTOR('',#47386,1000.);
#13668=VECTOR('',#47387,1000.);
#13669=VECTOR('',#47388,1000.);
#13670=VECTOR('',#47389,1000.);
#13671=VECTOR('',#47390,1000.);
#13672=VECTOR('',#47391,1000.);
#13673=VECTOR('',#47392,1000.);
#13674=VECTOR('',#47393,1000.);
#13675=VECTOR('',#47394,1000.);
#13676=VECTOR('',#47395,1000.);
#13677=VECTOR('',#47396,1000.);
#13678=VECTOR('',#47397,1000.);
#13679=VECTOR('',#47398,1000.);
#13680=VECTOR('',#47399,1000.);
#13681=VECTOR('',#47400,1000.);
#13682=VECTOR('',#47401,1000.);
#13683=VECTOR('',#47402,1000.);
#13684=VECTOR('',#47403,1000.);
#13685=VECTOR('',#47404,1000.);
#13686=VECTOR('',#47405,1000.);
#13687=VECTOR('',#47406,1000.);
#13688=VECTOR('',#47407,1000.);
#13689=VECTOR('',#47408,1000.);
#13690=VECTOR('',#47409,1000.);
#13691=VECTOR('',#47410,1000.);
#13692=VECTOR('',#47411,1000.);
#13693=VECTOR('',#47412,1000.);
#13694=VECTOR('',#47413,1000.);
#13695=VECTOR('',#47414,1000.);
#13696=VECTOR('',#47415,1000.);
#13697=VECTOR('',#47416,1000.);
#13698=VECTOR('',#47417,1000.);
#13699=VECTOR('',#47418,1000.);
#13700=VECTOR('',#47419,1000.);
#13701=VECTOR('',#47420,1000.);
#13702=VECTOR('',#47421,1000.);
#13703=VECTOR('',#47422,1000.);
#13704=VECTOR('',#47423,1000.);
#13705=VECTOR('',#47424,1000.);
#13706=VECTOR('',#47425,1000.);
#13707=VECTOR('',#47426,1000.);
#13708=VECTOR('',#47427,1000.);
#13709=VECTOR('',#47428,1000.);
#13710=VECTOR('',#47429,1000.);
#13711=VECTOR('',#47430,1000.);
#13712=VECTOR('',#47431,1000.);
#13713=VECTOR('',#47432,1000.);
#13714=VECTOR('',#47433,1000.);
#13715=VECTOR('',#47434,1000.);
#13716=VECTOR('',#47435,1000.);
#13717=VECTOR('',#47436,1000.);
#13718=VECTOR('',#47437,1000.);
#13719=VECTOR('',#47438,1000.);
#13720=VECTOR('',#47439,1000.);
#13721=VECTOR('',#47440,1000.);
#13722=VECTOR('',#47441,1000.);
#13723=VECTOR('',#47442,1000.);
#13724=VECTOR('',#47443,1000.);
#13725=VECTOR('',#47444,1000.);
#13726=VECTOR('',#47445,1000.);
#13727=VECTOR('',#47446,1000.);
#13728=VECTOR('',#47447,1000.);
#13729=VECTOR('',#47448,1000.);
#13730=VECTOR('',#47449,1000.);
#13731=VECTOR('',#47450,1000.);
#13732=VECTOR('',#47451,1000.);
#13733=VECTOR('',#47452,1000.);
#13734=VECTOR('',#47453,1000.);
#13735=VECTOR('',#47454,1000.);
#13736=VECTOR('',#47455,1000.);
#13737=VECTOR('',#47456,1000.);
#13738=VECTOR('',#47457,1000.);
#13739=VECTOR('',#47458,1000.);
#13740=VECTOR('',#47459,1000.);
#13741=VECTOR('',#47460,1000.);
#13742=VECTOR('',#47461,1000.);
#13743=VECTOR('',#47462,1000.);
#13744=VECTOR('',#47463,1000.);
#13745=VECTOR('',#47464,1000.);
#13746=VECTOR('',#47465,1000.);
#13747=VECTOR('',#47466,1000.);
#13748=VECTOR('',#47467,1000.);
#13749=VECTOR('',#47468,1000.);
#13750=VECTOR('',#47469,1000.);
#13751=VECTOR('',#47470,1000.);
#13752=VECTOR('',#47471,1000.);
#13753=VECTOR('',#47472,1000.);
#13754=VECTOR('',#47473,1000.);
#13755=VECTOR('',#47474,1000.);
#13756=VECTOR('',#47475,1000.);
#13757=VECTOR('',#47476,1000.);
#13758=VECTOR('',#47477,1000.);
#13759=VECTOR('',#47478,1000.);
#13760=VECTOR('',#47479,1000.);
#13761=VECTOR('',#47480,1000.);
#13762=VECTOR('',#47481,1000.);
#13763=VECTOR('',#47482,1000.);
#13764=VECTOR('',#47483,1000.);
#13765=VECTOR('',#47484,1000.);
#13766=VECTOR('',#47485,1000.);
#13767=VECTOR('',#47486,1000.);
#13768=VECTOR('',#47487,1000.);
#13769=VECTOR('',#47488,1000.);
#13770=VECTOR('',#47489,1000.);
#13771=VECTOR('',#47490,1000.);
#13772=VECTOR('',#47491,1000.);
#13773=VECTOR('',#47492,1000.);
#13774=VECTOR('',#47493,1000.);
#13775=VECTOR('',#47494,1000.);
#13776=VECTOR('',#47495,1000.);
#13777=VECTOR('',#47496,1000.);
#13778=VECTOR('',#47497,1000.);
#13779=VECTOR('',#47498,1000.);
#13780=VECTOR('',#47499,1000.);
#13781=VECTOR('',#47500,1000.);
#13782=VECTOR('',#47501,1000.);
#13783=VECTOR('',#47502,1000.);
#13784=VECTOR('',#47503,1000.);
#13785=VECTOR('',#47504,1000.);
#13786=VECTOR('',#47505,1000.);
#13787=VECTOR('',#47506,1000.);
#13788=VECTOR('',#47507,1000.);
#13789=VECTOR('',#47508,1000.);
#13790=VECTOR('',#47509,1000.);
#13791=VECTOR('',#47510,1000.);
#13792=VECTOR('',#47511,1000.);
#13793=VECTOR('',#47512,1000.);
#13794=VECTOR('',#47513,1000.);
#13795=VECTOR('',#47514,1000.);
#13796=VECTOR('',#47515,1000.);
#13797=VECTOR('',#47516,1000.);
#13798=VECTOR('',#47517,1000.);
#13799=VECTOR('',#47518,1000.);
#13800=VECTOR('',#47519,1000.);
#13801=VECTOR('',#47520,1000.);
#13802=VECTOR('',#47521,1000.);
#13803=VECTOR('',#47522,1000.);
#13804=VECTOR('',#47523,1000.);
#13805=VECTOR('',#47524,1000.);
#13806=VECTOR('',#47525,1000.);
#13807=VECTOR('',#47526,1000.);
#13808=VECTOR('',#47527,1000.);
#13809=VECTOR('',#47528,1000.);
#13810=VECTOR('',#47529,1000.);
#13811=VECTOR('',#47530,1000.);
#13812=VECTOR('',#47531,1000.);
#13813=VECTOR('',#47532,1000.);
#13814=VECTOR('',#47533,1000.);
#13815=VECTOR('',#47534,1000.);
#13816=VECTOR('',#47535,1000.);
#13817=VECTOR('',#47536,1000.);
#13818=VECTOR('',#47537,1000.);
#13819=VECTOR('',#47538,1000.);
#13820=VECTOR('',#47539,1000.);
#13821=VECTOR('',#47540,1000.);
#13822=VECTOR('',#47541,1000.);
#13823=VECTOR('',#47542,1000.);
#13824=VECTOR('',#47543,1000.);
#13825=VECTOR('',#47544,1000.);
#13826=VECTOR('',#47545,1000.);
#13827=VECTOR('',#47546,1000.);
#13828=VECTOR('',#47547,1000.);
#13829=VECTOR('',#47548,1000.);
#13830=VECTOR('',#47549,1000.);
#13831=VECTOR('',#47550,1000.);
#13832=VECTOR('',#47551,1000.);
#13833=VECTOR('',#47552,1000.);
#13834=VECTOR('',#47553,1000.);
#13835=VECTOR('',#47554,1000.);
#13836=VECTOR('',#47555,1000.);
#13837=VECTOR('',#47556,1000.);
#13838=VECTOR('',#47557,1000.);
#13839=VECTOR('',#47558,1000.);
#13840=VECTOR('',#47559,1000.);
#13841=VECTOR('',#47560,1000.);
#13842=VECTOR('',#47561,1000.);
#13843=VECTOR('',#47562,1000.);
#13844=VECTOR('',#47563,1000.);
#13845=VECTOR('',#47564,1000.);
#13846=VECTOR('',#47565,1000.);
#13847=VECTOR('',#47566,1000.);
#13848=VECTOR('',#47567,1000.);
#13849=VECTOR('',#47568,1000.);
#13850=VECTOR('',#47569,1000.);
#13851=VECTOR('',#47570,1000.);
#13852=VECTOR('',#47571,1000.);
#13853=VECTOR('',#47572,1000.);
#13854=VECTOR('',#47573,1000.);
#13855=VECTOR('',#47574,1000.);
#13856=VECTOR('',#47575,1000.);
#13857=VECTOR('',#47576,1000.);
#13858=VECTOR('',#47577,1000.);
#13859=VECTOR('',#47578,1000.);
#13860=VECTOR('',#47579,1000.);
#13861=VECTOR('',#47580,1000.);
#13862=VECTOR('',#47581,1000.);
#13863=VECTOR('',#47582,1000.);
#13864=VECTOR('',#47583,1000.);
#13865=VECTOR('',#47584,1000.);
#13866=VECTOR('',#47585,1000.);
#13867=VECTOR('',#47586,1000.);
#13868=VECTOR('',#47587,1000.);
#13869=VECTOR('',#47588,1000.);
#13870=VECTOR('',#47589,1000.);
#13871=VECTOR('',#47590,1000.);
#13872=VECTOR('',#47591,1000.);
#13873=VECTOR('',#47592,1000.);
#13874=VECTOR('',#47593,1000.);
#13875=VECTOR('',#47594,1000.);
#13876=VECTOR('',#47595,1000.);
#13877=VECTOR('',#47596,1000.);
#13878=VECTOR('',#47597,1000.);
#13879=VECTOR('',#47598,1000.);
#13880=VECTOR('',#47599,1000.);
#13881=VECTOR('',#47600,1000.);
#13882=VECTOR('',#47601,1000.);
#13883=VECTOR('',#47602,1000.);
#13884=VECTOR('',#47603,1000.);
#13885=VECTOR('',#47604,1000.);
#13886=VECTOR('',#47605,1000.);
#13887=VECTOR('',#47606,1000.);
#13888=VECTOR('',#47607,1000.);
#13889=VECTOR('',#47608,1000.);
#13890=VECTOR('',#47609,1000.);
#13891=VECTOR('',#47610,1000.);
#13892=VECTOR('',#47611,1000.);
#13893=VECTOR('',#47612,1000.);
#13894=VECTOR('',#47613,1000.);
#13895=VECTOR('',#47614,1000.);
#13896=VECTOR('',#47615,1000.);
#13897=VECTOR('',#47616,1000.);
#13898=VECTOR('',#47617,1000.);
#13899=VECTOR('',#47618,1000.);
#13900=VECTOR('',#47619,1000.);
#13901=VECTOR('',#47620,1000.);
#13902=VECTOR('',#47621,1000.);
#13903=VECTOR('',#47622,1000.);
#13904=VECTOR('',#47623,1000.);
#13905=VECTOR('',#47624,1000.);
#13906=VECTOR('',#47625,1000.);
#13907=VECTOR('',#47626,1000.);
#13908=VECTOR('',#47627,1000.);
#13909=VECTOR('',#47628,1000.);
#13910=VECTOR('',#47629,1000.);
#13911=VECTOR('',#47630,1000.);
#13912=VECTOR('',#47631,1000.);
#13913=VECTOR('',#47632,1000.);
#13914=VECTOR('',#47633,1000.);
#13915=VECTOR('',#47634,1000.);
#13916=VECTOR('',#47635,1000.);
#13917=VECTOR('',#47636,1000.);
#13918=VECTOR('',#47637,1000.);
#13919=VECTOR('',#47638,1000.);
#13920=VECTOR('',#47639,1000.);
#13921=VECTOR('',#47640,1000.);
#13922=VECTOR('',#47641,1000.);
#13923=VECTOR('',#47642,1000.);
#13924=VECTOR('',#47643,1000.);
#13925=VECTOR('',#47644,1000.);
#13926=VECTOR('',#47645,1000.);
#13927=VECTOR('',#47646,1000.);
#13928=VECTOR('',#47647,1000.);
#13929=VECTOR('',#47648,1000.);
#13930=VECTOR('',#47649,1000.);
#13931=VECTOR('',#47650,1000.);
#13932=VECTOR('',#47651,1000.);
#13933=VECTOR('',#47652,1000.);
#13934=VECTOR('',#47653,1000.);
#13935=VECTOR('',#47654,1000.);
#13936=VECTOR('',#47655,1000.);
#13937=VECTOR('',#47656,1000.);
#13938=VECTOR('',#47657,1000.);
#13939=VECTOR('',#47658,1000.);
#13940=VECTOR('',#47659,1000.);
#13941=VECTOR('',#47660,1000.);
#13942=VECTOR('',#47661,1000.);
#13943=VECTOR('',#47662,1000.);
#13944=VECTOR('',#47663,1000.);
#13945=VECTOR('',#47664,1000.);
#13946=VECTOR('',#47665,1000.);
#13947=VECTOR('',#47666,1000.);
#13948=VECTOR('',#47667,1000.);
#13949=VECTOR('',#47668,1000.);
#13950=VECTOR('',#47669,1000.);
#13951=VECTOR('',#47670,1000.);
#13952=VECTOR('',#47671,1000.);
#13953=VECTOR('',#47672,1000.);
#13954=VECTOR('',#47673,1000.);
#13955=VECTOR('',#47674,1000.);
#13956=VECTOR('',#47675,1000.);
#13957=VECTOR('',#47676,1000.);
#13958=VECTOR('',#47677,1000.);
#13959=VECTOR('',#47678,1000.);
#13960=VECTOR('',#47679,1000.);
#13961=VECTOR('',#47680,1000.);
#13962=VECTOR('',#47681,1000.);
#13963=VECTOR('',#47682,1000.);
#13964=VECTOR('',#47683,1000.);
#13965=VECTOR('',#47684,1000.);
#13966=VECTOR('',#47685,1000.);
#13967=VECTOR('',#47686,1000.);
#13968=VECTOR('',#47687,1000.);
#13969=VECTOR('',#47688,1000.);
#13970=VECTOR('',#47689,1000.);
#13971=VECTOR('',#47690,1000.);
#13972=VECTOR('',#47691,1000.);
#13973=VECTOR('',#47692,1000.);
#13974=VECTOR('',#47693,1000.);
#13975=VECTOR('',#47694,1000.);
#13976=VECTOR('',#47695,1000.);
#13977=VECTOR('',#47696,1000.);
#13978=VECTOR('',#47697,1000.);
#13979=VECTOR('',#47698,1000.);
#13980=VECTOR('',#47699,1000.);
#13981=VECTOR('',#47700,1000.);
#13982=VECTOR('',#47701,1000.);
#13983=VECTOR('',#47702,1000.);
#13984=VECTOR('',#47703,1000.);
#13985=VECTOR('',#47704,1000.);
#13986=VECTOR('',#47705,1000.);
#13987=VECTOR('',#47706,1000.);
#13988=VECTOR('',#47707,1000.);
#13989=VECTOR('',#47708,1000.);
#13990=VECTOR('',#47709,1000.);
#13991=VECTOR('',#47710,1000.);
#13992=VECTOR('',#47711,1000.);
#13993=VECTOR('',#47712,1000.);
#13994=VECTOR('',#47713,1000.);
#13995=VECTOR('',#47714,1000.);
#13996=VECTOR('',#47715,1000.);
#13997=VECTOR('',#47716,1000.);
#13998=VECTOR('',#47717,1000.);
#13999=VECTOR('',#47718,1000.);
#14000=VECTOR('',#47719,1000.);
#14001=VECTOR('',#47720,1000.);
#14002=VECTOR('',#47721,1000.);
#14003=VECTOR('',#47722,1000.);
#14004=VECTOR('',#47723,1000.);
#14005=VECTOR('',#47724,1000.);
#14006=VECTOR('',#47725,1000.);
#14007=VECTOR('',#47726,1000.);
#14008=VECTOR('',#47727,1000.);
#14009=VECTOR('',#47728,1000.);
#14010=VECTOR('',#47729,1000.);
#14011=VECTOR('',#47730,1000.);
#14012=VECTOR('',#47731,1000.);
#14013=VECTOR('',#47732,1000.);
#14014=VECTOR('',#47733,1000.);
#14015=VECTOR('',#47734,1000.);
#14016=VECTOR('',#47735,1000.);
#14017=VECTOR('',#47736,1000.);
#14018=VECTOR('',#47737,1000.);
#14019=VECTOR('',#47738,1000.);
#14020=VECTOR('',#47739,1000.);
#14021=VECTOR('',#47740,1000.);
#14022=VECTOR('',#47741,1000.);
#14023=VECTOR('',#47742,1000.);
#14024=VECTOR('',#47743,1000.);
#14025=VECTOR('',#47744,1000.);
#14026=VECTOR('',#47745,1000.);
#14027=VECTOR('',#47746,1000.);
#14028=VECTOR('',#47747,1000.);
#14029=VECTOR('',#47748,1000.);
#14030=VECTOR('',#47749,1000.);
#14031=VECTOR('',#47750,1000.);
#14032=VECTOR('',#47751,1000.);
#14033=VECTOR('',#47752,1000.);
#14034=VECTOR('',#47753,1000.);
#14035=VECTOR('',#47754,1000.);
#14036=VECTOR('',#47755,1000.);
#14037=VECTOR('',#47756,1000.);
#14038=VECTOR('',#47757,1000.);
#14039=VECTOR('',#47758,1000.);
#14040=VECTOR('',#47759,1000.);
#14041=VECTOR('',#47760,1000.);
#14042=VECTOR('',#47761,1000.);
#14043=VECTOR('',#47762,1000.);
#14044=VECTOR('',#47763,1000.);
#14045=VECTOR('',#47764,1000.);
#14046=VECTOR('',#47765,1000.);
#14047=VECTOR('',#47766,1000.);
#14048=VECTOR('',#47767,1000.);
#14049=VECTOR('',#47768,1000.);
#14050=VECTOR('',#47769,1000.);
#14051=VECTOR('',#47770,1000.);
#14052=VECTOR('',#47771,1000.);
#14053=VECTOR('',#47772,1000.);
#14054=VECTOR('',#47773,1000.);
#14055=VECTOR('',#47774,1000.);
#14056=VECTOR('',#47775,1000.);
#14057=VECTOR('',#47776,1000.);
#14058=VECTOR('',#47777,1000.);
#14059=VECTOR('',#47778,1000.);
#14060=VECTOR('',#47779,1000.);
#14061=VECTOR('',#47780,1000.);
#14062=VECTOR('',#47781,1000.);
#14063=VECTOR('',#47782,1000.);
#14064=VECTOR('',#47783,1000.);
#14065=VECTOR('',#47784,1000.);
#14066=VECTOR('',#47785,1000.);
#14067=VECTOR('',#47786,1000.);
#14068=VECTOR('',#47787,1000.);
#14069=VECTOR('',#47788,1000.);
#14070=VECTOR('',#47789,1000.);
#14071=VECTOR('',#47790,1000.);
#14072=VECTOR('',#47791,1000.);
#14073=VECTOR('',#47792,1000.);
#14074=VECTOR('',#47793,1000.);
#14075=VECTOR('',#47794,1000.);
#14076=VECTOR('',#47795,1000.);
#14077=VECTOR('',#47796,1000.);
#14078=VECTOR('',#47797,1000.);
#14079=VECTOR('',#47798,1000.);
#14080=VECTOR('',#47799,1000.);
#14081=VECTOR('',#47800,1000.);
#14082=VECTOR('',#47801,1000.);
#14083=VECTOR('',#47802,1000.);
#14084=VECTOR('',#47803,1000.);
#14085=VECTOR('',#47804,1000.);
#14086=VECTOR('',#47805,1000.);
#14087=VECTOR('',#47806,1000.);
#14088=VECTOR('',#47807,1000.);
#14089=VECTOR('',#47808,1000.);
#14090=VECTOR('',#47809,1000.);
#14091=VECTOR('',#47810,1000.);
#14092=VECTOR('',#47811,1000.);
#14093=VECTOR('',#47812,1000.);
#14094=VECTOR('',#47813,1000.);
#14095=VECTOR('',#47814,1000.);
#14096=VECTOR('',#47815,1000.);
#14097=VECTOR('',#47816,1000.);
#14098=VECTOR('',#47817,1000.);
#14099=VECTOR('',#47818,1000.);
#14100=VECTOR('',#47819,1000.);
#14101=VECTOR('',#47820,1000.);
#14102=VECTOR('',#47821,1000.);
#14103=VECTOR('',#47822,1000.);
#14104=VECTOR('',#47823,1000.);
#14105=VECTOR('',#47824,1000.);
#14106=VECTOR('',#47825,1000.);
#14107=VECTOR('',#47826,1000.);
#14108=VECTOR('',#47827,1000.);
#14109=VECTOR('',#47828,1000.);
#14110=VECTOR('',#47829,1000.);
#14111=VECTOR('',#47830,1000.);
#14112=VECTOR('',#47831,1000.);
#14113=VECTOR('',#47832,1000.);
#14114=VECTOR('',#47833,1000.);
#14115=VECTOR('',#47834,1000.);
#14116=VECTOR('',#47835,1000.);
#14117=VECTOR('',#47836,1000.);
#14118=VECTOR('',#47837,1000.);
#14119=VECTOR('',#47838,1000.);
#14120=VECTOR('',#47839,1000.);
#14121=VECTOR('',#47840,1000.);
#14122=VECTOR('',#47841,1000.);
#14123=VECTOR('',#47842,1000.);
#14124=VECTOR('',#47843,1000.);
#14125=VECTOR('',#47844,1000.);
#14126=VECTOR('',#47845,1000.);
#14127=VECTOR('',#47846,1000.);
#14128=VECTOR('',#47847,1000.);
#14129=VECTOR('',#47848,1000.);
#14130=VECTOR('',#47849,1000.);
#14131=VECTOR('',#47850,1000.);
#14132=VECTOR('',#47851,1000.);
#14133=VECTOR('',#47852,1000.);
#14134=VECTOR('',#47853,1000.);
#14135=VECTOR('',#47854,1000.);
#14136=VECTOR('',#47855,1000.);
#14137=VECTOR('',#47856,1000.);
#14138=VECTOR('',#47857,1000.);
#14139=VECTOR('',#47858,1000.);
#14140=VECTOR('',#47859,1000.);
#14141=VECTOR('',#47860,1000.);
#14142=VECTOR('',#47861,1000.);
#14143=VECTOR('',#47862,1000.);
#14144=VECTOR('',#47863,1000.);
#14145=VECTOR('',#47864,1000.);
#14146=VECTOR('',#47865,1000.);
#14147=VECTOR('',#47866,1000.);
#14148=VECTOR('',#47867,1000.);
#14149=VECTOR('',#47868,1000.);
#14150=VECTOR('',#47869,1000.);
#14151=VECTOR('',#47870,1000.);
#14152=VECTOR('',#47871,1000.);
#14153=VECTOR('',#47872,1000.);
#14154=VECTOR('',#47873,1000.);
#14155=VECTOR('',#47874,1000.);
#14156=VECTOR('',#47875,1000.);
#14157=VECTOR('',#47876,1000.);
#14158=VECTOR('',#47877,1000.);
#14159=VECTOR('',#47878,1000.);
#14160=VECTOR('',#47879,1000.);
#14161=VECTOR('',#47880,1000.);
#14162=VECTOR('',#47881,1000.);
#14163=VECTOR('',#47882,1000.);
#14164=VECTOR('',#47883,1000.);
#14165=VECTOR('',#47884,1000.);
#14166=VECTOR('',#47885,1000.);
#14167=VECTOR('',#47886,1000.);
#14168=VECTOR('',#47887,1000.);
#14169=VECTOR('',#47888,1000.);
#14170=VECTOR('',#47889,1000.);
#14171=VECTOR('',#47890,1000.);
#14172=VECTOR('',#47891,1000.);
#14173=VECTOR('',#47892,1000.);
#14174=VECTOR('',#47893,1000.);
#14175=VECTOR('',#47894,1000.);
#14176=VECTOR('',#47895,1000.);
#14177=VECTOR('',#47896,1000.);
#14178=VECTOR('',#47897,1000.);
#14179=VECTOR('',#47898,1000.);
#14180=VECTOR('',#47899,1000.);
#14181=VECTOR('',#47900,1000.);
#14182=VECTOR('',#47901,1000.);
#14183=VECTOR('',#47902,1000.);
#14184=VECTOR('',#47903,1000.);
#14185=VECTOR('',#47904,1000.);
#14186=VECTOR('',#47905,1000.);
#14187=VECTOR('',#47906,1000.);
#14188=VECTOR('',#47907,1000.);
#14189=VECTOR('',#47908,1000.);
#14190=VECTOR('',#47909,1000.);
#14191=VECTOR('',#47910,1000.);
#14192=VECTOR('',#47911,1000.);
#14193=VECTOR('',#47912,1000.);
#14194=VECTOR('',#47913,1000.);
#14195=VECTOR('',#47914,1000.);
#14196=VECTOR('',#47915,1000.);
#14197=VECTOR('',#47916,1000.);
#14198=VECTOR('',#47917,1000.);
#14199=VECTOR('',#47918,1000.);
#14200=VECTOR('',#47919,1000.);
#14201=VECTOR('',#47920,1000.);
#14202=VECTOR('',#47921,1000.);
#14203=VECTOR('',#47922,1000.);
#14204=VECTOR('',#47923,1000.);
#14205=VECTOR('',#47924,1000.);
#14206=VECTOR('',#47925,1000.);
#14207=VECTOR('',#47926,1000.);
#14208=VECTOR('',#47927,1000.);
#14209=VECTOR('',#47928,1000.);
#14210=VECTOR('',#47929,1000.);
#14211=VECTOR('',#47930,1000.);
#14212=VECTOR('',#47931,1000.);
#14213=VECTOR('',#47932,1000.);
#14214=VECTOR('',#47933,1000.);
#14215=VECTOR('',#47934,1000.);
#14216=VECTOR('',#47935,1000.);
#14217=VECTOR('',#47936,1000.);
#14218=VECTOR('',#47937,1000.);
#14219=VECTOR('',#47938,1000.);
#14220=VECTOR('',#47939,1000.);
#14221=VECTOR('',#47940,1000.);
#14222=VECTOR('',#47941,1000.);
#14223=VECTOR('',#47942,1000.);
#14224=VECTOR('',#47943,1000.);
#14225=VECTOR('',#47944,1000.);
#14226=VECTOR('',#47945,1000.);
#14227=VECTOR('',#47946,1000.);
#14228=VECTOR('',#47947,1000.);
#14229=VECTOR('',#47948,1000.);
#14230=VECTOR('',#47949,1000.);
#14231=VECTOR('',#47950,1000.);
#14232=VECTOR('',#47951,1000.);
#14233=VECTOR('',#47952,1000.);
#14234=VECTOR('',#47953,1000.);
#14235=VECTOR('',#47954,1000.);
#14236=VECTOR('',#47955,1000.);
#14237=VECTOR('',#47956,1000.);
#14238=VECTOR('',#47957,1000.);
#14239=VECTOR('',#47958,1000.);
#14240=VECTOR('',#47959,1000.);
#14241=VECTOR('',#47960,1000.);
#14242=VECTOR('',#47961,1000.);
#14243=VECTOR('',#47962,1000.);
#14244=VECTOR('',#47963,1000.);
#14245=VECTOR('',#47964,1000.);
#14246=VECTOR('',#47965,1000.);
#14247=VECTOR('',#47966,1000.);
#14248=VECTOR('',#47967,1000.);
#14249=VECTOR('',#47968,1000.);
#14250=VECTOR('',#47969,1000.);
#14251=VECTOR('',#47970,1000.);
#14252=VECTOR('',#47971,1000.);
#14253=VECTOR('',#47972,1000.);
#14254=VECTOR('',#47973,1000.);
#14255=VECTOR('',#47974,1000.);
#14256=VECTOR('',#47975,1000.);
#14257=VECTOR('',#47976,1000.);
#14258=VECTOR('',#47979,1000.);
#14259=VECTOR('',#47980,1000.);
#14260=VECTOR('',#47981,1000.);
#14261=VECTOR('',#47982,1000.);
#14262=VECTOR('',#47983,1000.);
#14263=VECTOR('',#47984,1000.);
#14264=VECTOR('',#47985,1000.);
#14265=VECTOR('',#47986,1000.);
#14266=VECTOR('',#47987,1000.);
#14267=VECTOR('',#47988,1000.);
#14268=VECTOR('',#47989,1000.);
#14269=VECTOR('',#47990,1000.);
#14270=VECTOR('',#47991,1000.);
#14271=VECTOR('',#47992,1000.);
#14272=VECTOR('',#47993,1000.);
#14273=VECTOR('',#47994,1000.);
#14274=VECTOR('',#47995,1000.);
#14275=VECTOR('',#47996,1000.);
#14276=VECTOR('',#47997,1000.);
#14277=VECTOR('',#47998,1000.);
#14278=VECTOR('',#47999,1000.);
#14279=VECTOR('',#48000,1000.);
#14280=VECTOR('',#48001,1000.);
#14281=VECTOR('',#48002,1000.);
#14282=VECTOR('',#48003,1000.);
#14283=VECTOR('',#48004,1000.);
#14284=VECTOR('',#48005,1000.);
#14285=VECTOR('',#48006,1000.);
#14286=VECTOR('',#48007,1000.);
#14287=VECTOR('',#48008,1000.);
#14288=VECTOR('',#48009,1000.);
#14289=VECTOR('',#48010,1000.);
#14290=VECTOR('',#48011,1000.);
#14291=VECTOR('',#48012,1000.);
#14292=VECTOR('',#48013,1000.);
#14293=VECTOR('',#48014,1000.);
#14294=VECTOR('',#48015,1000.);
#14295=VECTOR('',#48016,1000.);
#14296=VECTOR('',#48017,1000.);
#14297=VECTOR('',#48018,1000.);
#14298=VECTOR('',#48019,1000.);
#14299=VECTOR('',#48020,1000.);
#14300=VECTOR('',#48021,1000.);
#14301=VECTOR('',#48022,1000.);
#14302=VECTOR('',#48023,1000.);
#14303=VECTOR('',#48024,1000.);
#14304=VECTOR('',#48025,1000.);
#14305=VECTOR('',#48026,1000.);
#14306=VECTOR('',#48027,1000.);
#14307=VECTOR('',#48028,1000.);
#14308=VECTOR('',#48029,1000.);
#14309=VECTOR('',#48030,1000.);
#14310=VECTOR('',#48031,1000.);
#14311=VECTOR('',#48032,1000.);
#14312=VECTOR('',#48033,1000.);
#14313=VECTOR('',#48034,1000.);
#14314=VECTOR('',#48035,1000.);
#14315=VECTOR('',#48036,1000.);
#14316=VECTOR('',#48037,1000.);
#14317=VECTOR('',#48038,1000.);
#14318=VECTOR('',#48039,1000.);
#14319=VECTOR('',#48040,1000.);
#14320=VECTOR('',#48041,1000.);
#14321=VECTOR('',#48042,1000.);
#14322=VECTOR('',#48043,1000.);
#14323=VECTOR('',#48044,1000.);
#14324=VECTOR('',#48045,1000.);
#14325=VECTOR('',#48046,1000.);
#14326=VECTOR('',#48047,1000.);
#14327=VECTOR('',#48048,1000.);
#14328=VECTOR('',#48049,1000.);
#14329=VECTOR('',#48050,1000.);
#14330=VECTOR('',#48051,1000.);
#14331=VECTOR('',#48052,1000.);
#14332=VECTOR('',#48053,1000.);
#14333=VECTOR('',#48054,1000.);
#14334=VECTOR('',#48055,1000.);
#14335=VECTOR('',#48056,1000.);
#14336=VECTOR('',#48057,1000.);
#14337=VECTOR('',#48058,1000.);
#14338=VECTOR('',#48059,1000.);
#14339=VECTOR('',#48060,1000.);
#14340=VECTOR('',#48061,1000.);
#14341=VECTOR('',#48062,1000.);
#14342=VECTOR('',#48063,1000.);
#14343=VECTOR('',#48064,1000.);
#14344=VECTOR('',#48065,1000.);
#14345=VECTOR('',#48066,1000.);
#14346=VECTOR('',#48067,1000.);
#14347=VECTOR('',#48068,1000.);
#14348=VECTOR('',#48069,1000.);
#14349=VECTOR('',#48070,1000.);
#14350=VECTOR('',#48071,1000.);
#14351=VECTOR('',#48072,1000.);
#14352=VECTOR('',#48073,1000.);
#14353=VECTOR('',#48074,1000.);
#14354=VECTOR('',#48075,1000.);
#14355=VECTOR('',#48076,1000.);
#14356=VECTOR('',#48077,1000.);
#14357=VECTOR('',#48078,1000.);
#14358=VECTOR('',#48079,1000.);
#14359=VECTOR('',#48080,1000.);
#14360=VECTOR('',#48081,1000.);
#14361=VECTOR('',#48082,1000.);
#14362=VECTOR('',#48083,1000.);
#14363=VECTOR('',#48084,1000.);
#14364=VECTOR('',#48085,1000.);
#14365=VECTOR('',#48086,1000.);
#14366=VECTOR('',#48087,1000.);
#14367=VECTOR('',#48088,1000.);
#14368=VECTOR('',#48089,1000.);
#14369=VECTOR('',#48090,1000.);
#14370=VECTOR('',#48091,1000.);
#14371=VECTOR('',#48092,1000.);
#14372=VECTOR('',#48093,1000.);
#14373=VECTOR('',#48094,1000.);
#14374=VECTOR('',#48095,1000.);
#14375=VECTOR('',#48096,1000.);
#14376=VECTOR('',#48097,1000.);
#14377=VECTOR('',#48098,1000.);
#14378=VECTOR('',#48099,1000.);
#14379=VECTOR('',#48100,1000.);
#14380=VECTOR('',#48101,1000.);
#14381=VECTOR('',#48102,1000.);
#14382=VECTOR('',#48103,1000.);
#14383=VECTOR('',#48104,1000.);
#14384=VECTOR('',#48105,1000.);
#14385=VECTOR('',#48106,1000.);
#14386=VECTOR('',#48107,1000.);
#14387=VECTOR('',#48108,1000.);
#14388=VECTOR('',#48109,1000.);
#14389=VECTOR('',#48110,1000.);
#14390=VECTOR('',#48111,1000.);
#14391=VECTOR('',#48112,1000.);
#14392=VECTOR('',#48113,1000.);
#14393=VECTOR('',#48114,1000.);
#14394=VECTOR('',#48115,1000.);
#14395=VECTOR('',#48116,1000.);
#14396=VECTOR('',#48117,1000.);
#14397=VECTOR('',#48118,1000.);
#14398=VECTOR('',#48119,1000.);
#14399=VECTOR('',#48120,1000.);
#14400=VECTOR('',#48121,1000.);
#14401=VECTOR('',#48122,1000.);
#14402=VECTOR('',#48123,1000.);
#14403=VECTOR('',#48124,1000.);
#14404=VECTOR('',#48125,1000.);
#14405=VECTOR('',#48126,1000.);
#14406=VECTOR('',#48127,1000.);
#14407=VECTOR('',#48128,1000.);
#14408=VECTOR('',#48129,1000.);
#14409=VECTOR('',#48130,1000.);
#14410=VECTOR('',#48131,1000.);
#14411=VECTOR('',#48132,1000.);
#14412=VECTOR('',#48133,1000.);
#14413=VECTOR('',#48134,1000.);
#14414=VECTOR('',#48135,1000.);
#14415=VECTOR('',#48136,1000.);
#14416=VECTOR('',#48137,1000.);
#14417=VECTOR('',#48138,1000.);
#14418=VECTOR('',#48139,1000.);
#14419=VECTOR('',#48140,1000.);
#14420=VECTOR('',#48141,1000.);
#14421=VECTOR('',#48142,1000.);
#14422=VECTOR('',#48143,1000.);
#14423=VECTOR('',#48144,1000.);
#14424=VECTOR('',#48145,1000.);
#14425=VECTOR('',#48146,1000.);
#14426=VECTOR('',#48147,1000.);
#14427=VECTOR('',#48148,1000.);
#14428=VECTOR('',#48149,1000.);
#14429=VECTOR('',#48150,1000.);
#14430=VECTOR('',#48151,1000.);
#14431=VECTOR('',#48152,1000.);
#14432=VECTOR('',#48153,1000.);
#14433=VECTOR('',#48154,1000.);
#14434=VECTOR('',#48155,1000.);
#14435=VECTOR('',#48156,1000.);
#14436=VECTOR('',#48157,1000.);
#14437=VECTOR('',#48158,1000.);
#14438=VECTOR('',#48159,1000.);
#14439=VECTOR('',#48160,1000.);
#14440=VECTOR('',#48161,1000.);
#14441=VECTOR('',#48162,1000.);
#14442=VECTOR('',#48163,1000.);
#14443=VECTOR('',#48164,1000.);
#14444=VECTOR('',#48165,1000.);
#14445=VECTOR('',#48166,1000.);
#14446=VECTOR('',#48167,1000.);
#14447=VECTOR('',#48168,1000.);
#14448=VECTOR('',#48169,1000.);
#14449=VECTOR('',#48170,1000.);
#14450=VECTOR('',#48171,1000.);
#14451=VECTOR('',#48172,1000.);
#14452=VECTOR('',#48173,1000.);
#14453=VECTOR('',#48174,1000.);
#14454=VECTOR('',#48175,1000.);
#14455=VECTOR('',#48176,1000.);
#14456=VECTOR('',#48177,1000.);
#14457=VECTOR('',#48178,1000.);
#14458=VECTOR('',#48179,1000.);
#14459=VECTOR('',#48180,1000.);
#14460=VECTOR('',#48181,1000.);
#14461=VECTOR('',#48182,1000.);
#14462=VECTOR('',#48183,1000.);
#14463=VECTOR('',#48184,1000.);
#14464=VECTOR('',#48185,1000.);
#14465=VECTOR('',#48186,1000.);
#14466=VECTOR('',#48187,1000.);
#14467=VECTOR('',#48188,1000.);
#14468=VECTOR('',#48189,1000.);
#14469=VECTOR('',#48190,1000.);
#14470=VECTOR('',#48191,1000.);
#14471=VECTOR('',#48192,1000.);
#14472=VECTOR('',#48193,1000.);
#14473=VECTOR('',#48194,1000.);
#14474=VECTOR('',#48195,1000.);
#14475=VECTOR('',#48196,1000.);
#14476=VECTOR('',#48197,1000.);
#14477=VECTOR('',#48198,1000.);
#14478=VECTOR('',#48199,1000.);
#14479=VECTOR('',#48200,1000.);
#14480=VECTOR('',#48201,1000.);
#14481=VECTOR('',#48202,1000.);
#14482=VECTOR('',#48203,1000.);
#14483=VECTOR('',#48204,1000.);
#14484=VECTOR('',#48205,1000.);
#14485=VECTOR('',#48206,1000.);
#14486=VECTOR('',#48207,1000.);
#14487=VECTOR('',#48208,1000.);
#14488=VECTOR('',#48209,1000.);
#14489=VECTOR('',#48210,1000.);
#14490=VECTOR('',#48211,1000.);
#14491=VECTOR('',#48212,1000.);
#14492=VECTOR('',#48213,1000.);
#14493=VECTOR('',#48214,1000.);
#14494=VECTOR('',#48215,1000.);
#14495=VECTOR('',#48216,1000.);
#14496=VECTOR('',#48217,1000.);
#14497=VECTOR('',#48218,1000.);
#14498=VECTOR('',#48219,1000.);
#14499=VECTOR('',#48220,1000.);
#14500=VECTOR('',#48221,1000.);
#14501=VECTOR('',#48222,1000.);
#14502=VECTOR('',#48223,1000.);
#14503=VECTOR('',#48224,1000.);
#14504=VECTOR('',#48225,1000.);
#14505=VECTOR('',#48226,1000.);
#14506=VECTOR('',#48227,1000.);
#14507=VECTOR('',#48228,1000.);
#14508=VECTOR('',#48229,1000.);
#14509=VECTOR('',#48230,1000.);
#14510=VECTOR('',#48231,1000.);
#14511=VECTOR('',#48232,1000.);
#14512=VECTOR('',#48233,1000.);
#14513=VECTOR('',#48234,1000.);
#14514=VECTOR('',#48235,1000.);
#14515=VECTOR('',#48236,1000.);
#14516=VECTOR('',#48237,1000.);
#14517=VECTOR('',#48238,1000.);
#14518=VECTOR('',#48239,1000.);
#14519=VECTOR('',#48240,1000.);
#14520=VECTOR('',#48241,1000.);
#14521=VECTOR('',#48242,1000.);
#14522=VECTOR('',#48243,1000.);
#14523=VECTOR('',#48244,1000.);
#14524=VECTOR('',#48245,1000.);
#14525=VECTOR('',#48246,1000.);
#14526=VECTOR('',#48247,1000.);
#14527=VECTOR('',#48248,1000.);
#14528=VECTOR('',#48249,1000.);
#14529=VECTOR('',#48250,1000.);
#14530=VECTOR('',#48251,1000.);
#14531=VECTOR('',#48252,1000.);
#14532=VECTOR('',#48253,1000.);
#14533=VECTOR('',#48254,1000.);
#14534=VECTOR('',#48255,1000.);
#14535=VECTOR('',#48256,1000.);
#14536=VECTOR('',#48257,1000.);
#14537=VECTOR('',#48258,1000.);
#14538=VECTOR('',#48259,1000.);
#14539=VECTOR('',#48260,1000.);
#14540=VECTOR('',#48261,1000.);
#14541=VECTOR('',#48262,1000.);
#14542=VECTOR('',#48263,1000.);
#14543=VECTOR('',#48264,1000.);
#14544=VECTOR('',#48265,1000.);
#14545=VECTOR('',#48266,1000.);
#14546=VECTOR('',#48267,1000.);
#14547=VECTOR('',#48268,1000.);
#14548=VECTOR('',#48269,1000.);
#14549=VECTOR('',#48270,1000.);
#14550=VECTOR('',#48271,1000.);
#14551=VECTOR('',#48272,1000.);
#14552=VECTOR('',#48273,1000.);
#14553=VECTOR('',#48274,1000.);
#14554=VECTOR('',#48275,1000.);
#14555=VECTOR('',#48276,1000.);
#14556=VECTOR('',#48277,1000.);
#14557=VECTOR('',#48278,1000.);
#14558=VECTOR('',#48279,1000.);
#14559=VECTOR('',#48280,1000.);
#14560=VECTOR('',#48281,1000.);
#14561=VECTOR('',#48282,1000.);
#14562=VECTOR('',#48283,1000.);
#14563=VECTOR('',#48284,1000.);
#14564=VECTOR('',#48285,1000.);
#14565=VECTOR('',#48286,1000.);
#14566=VECTOR('',#48287,1000.);
#14567=VECTOR('',#48288,1000.);
#14568=VECTOR('',#48289,1000.);
#14569=VECTOR('',#48290,1000.);
#14570=VECTOR('',#48291,1000.);
#14571=VECTOR('',#48292,1000.);
#14572=VECTOR('',#48293,1000.);
#14573=VECTOR('',#48294,1000.);
#14574=VECTOR('',#48295,1000.);
#14575=VECTOR('',#48296,1000.);
#14576=VECTOR('',#48297,1000.);
#14577=VECTOR('',#48298,1000.);
#14578=VECTOR('',#48299,1000.);
#14579=VECTOR('',#48300,1000.);
#14580=VECTOR('',#48301,1000.);
#14581=VECTOR('',#48302,1000.);
#14582=VECTOR('',#48303,1000.);
#14583=VECTOR('',#48304,1000.);
#14584=VECTOR('',#48305,1000.);
#14585=VECTOR('',#48306,1000.);
#14586=VECTOR('',#48307,1000.);
#14587=VECTOR('',#48308,1000.);
#14588=VECTOR('',#48309,1000.);
#14589=VECTOR('',#48310,1000.);
#14590=VECTOR('',#48311,1000.);
#14591=VECTOR('',#48312,1000.);
#14592=VECTOR('',#48313,1000.);
#14593=VECTOR('',#48314,1000.);
#14594=VECTOR('',#48315,1000.);
#14595=VECTOR('',#48316,1000.);
#14596=VECTOR('',#48317,1000.);
#14597=VECTOR('',#48318,1000.);
#14598=VECTOR('',#48319,1000.);
#14599=VECTOR('',#48320,1000.);
#14600=VECTOR('',#48321,1000.);
#14601=VECTOR('',#48322,1000.);
#14602=VECTOR('',#48323,1000.);
#14603=VECTOR('',#48324,1000.);
#14604=VECTOR('',#48325,1000.);
#14605=VECTOR('',#48326,1000.);
#14606=VECTOR('',#48327,1000.);
#14607=VECTOR('',#48328,1000.);
#14608=VECTOR('',#48329,1000.);
#14609=VECTOR('',#48330,1000.);
#14610=VECTOR('',#48331,1000.);
#14611=VECTOR('',#48332,1000.);
#14612=VECTOR('',#48333,1000.);
#14613=VECTOR('',#48334,1000.);
#14614=VECTOR('',#48335,1000.);
#14615=VECTOR('',#48336,1000.);
#14616=VECTOR('',#48337,1000.);
#14617=VECTOR('',#48338,1000.);
#14618=VECTOR('',#48339,1000.);
#14619=VECTOR('',#48340,1000.);
#14620=VECTOR('',#48341,1000.);
#14621=VECTOR('',#48342,1000.);
#14622=VECTOR('',#48343,1000.);
#14623=VECTOR('',#48344,1000.);
#14624=VECTOR('',#48345,1000.);
#14625=VECTOR('',#48346,1000.);
#14626=VECTOR('',#48347,1000.);
#14627=VECTOR('',#48348,1000.);
#14628=VECTOR('',#48349,1000.);
#14629=VECTOR('',#48350,1000.);
#14630=VECTOR('',#48351,1000.);
#14631=VECTOR('',#48352,1000.);
#14632=VECTOR('',#48353,1000.);
#14633=VECTOR('',#48354,1000.);
#14634=VECTOR('',#48355,1000.);
#14635=VECTOR('',#48356,1000.);
#14636=VECTOR('',#48357,1000.);
#14637=VECTOR('',#48358,1000.);
#14638=VECTOR('',#48359,1000.);
#14639=VECTOR('',#48360,1000.);
#14640=VECTOR('',#48361,1000.);
#14641=VECTOR('',#48362,1000.);
#14642=VECTOR('',#48363,1000.);
#14643=VECTOR('',#48364,1000.);
#14644=VECTOR('',#48365,1000.);
#14645=VECTOR('',#48366,1000.);
#14646=VECTOR('',#48367,1000.);
#14647=VECTOR('',#48368,1000.);
#14648=VECTOR('',#48369,1000.);
#14649=VECTOR('',#48370,1000.);
#14650=VECTOR('',#48371,1000.);
#14651=VECTOR('',#48372,1000.);
#14652=VECTOR('',#48373,1000.);
#14653=VECTOR('',#48374,1000.);
#14654=VECTOR('',#48375,1000.);
#14655=VECTOR('',#48376,1000.);
#14656=VECTOR('',#48377,1000.);
#14657=VECTOR('',#48378,1000.);
#14658=VECTOR('',#48379,1000.);
#14659=VECTOR('',#48380,1000.);
#14660=VECTOR('',#48381,1000.);
#14661=VECTOR('',#48382,1000.);
#14662=VECTOR('',#48383,1000.);
#14663=VECTOR('',#48384,1000.);
#14664=VECTOR('',#48385,1000.);
#14665=VECTOR('',#48386,1000.);
#14666=VECTOR('',#48387,1000.);
#14667=VECTOR('',#48388,1000.);
#14668=VECTOR('',#48389,1000.);
#14669=VECTOR('',#48390,1000.);
#14670=VECTOR('',#48391,1000.);
#14671=VECTOR('',#48392,1000.);
#14672=VECTOR('',#48393,1000.);
#14673=VECTOR('',#48394,1000.);
#14674=VECTOR('',#48395,1000.);
#14675=VECTOR('',#48396,1000.);
#14676=VECTOR('',#48397,1000.);
#14677=VECTOR('',#48398,1000.);
#14678=VECTOR('',#48399,1000.);
#14679=VECTOR('',#48400,1000.);
#14680=VECTOR('',#48401,1000.);
#14681=VECTOR('',#48402,1000.);
#14682=VECTOR('',#48403,1000.);
#14683=VECTOR('',#48404,1000.);
#14684=VECTOR('',#48405,1000.);
#14685=VECTOR('',#48406,1000.);
#14686=VECTOR('',#48407,1000.);
#14687=VECTOR('',#48408,1000.);
#14688=VECTOR('',#48409,1000.);
#14689=VECTOR('',#48410,1000.);
#14690=VECTOR('',#48411,1000.);
#14691=VECTOR('',#48412,1000.);
#14692=VECTOR('',#48413,1000.);
#14693=VECTOR('',#48414,1000.);
#14694=VECTOR('',#48415,1000.);
#14695=VECTOR('',#48416,1000.);
#14696=VECTOR('',#48417,1000.);
#14697=VECTOR('',#48418,1000.);
#14698=VECTOR('',#48419,1000.);
#14699=VECTOR('',#48420,1000.);
#14700=VECTOR('',#48421,1000.);
#14701=VECTOR('',#48422,1000.);
#14702=VECTOR('',#48423,1000.);
#14703=VECTOR('',#48424,1000.);
#14704=VECTOR('',#48425,1000.);
#14705=VECTOR('',#48426,1000.);
#14706=VECTOR('',#48427,1000.);
#14707=VECTOR('',#48428,1000.);
#14708=VECTOR('',#48429,1000.);
#14709=VECTOR('',#48430,1000.);
#14710=VECTOR('',#48431,1000.);
#14711=VECTOR('',#48432,1000.);
#14712=VECTOR('',#48433,1000.);
#14713=VECTOR('',#48434,1000.);
#14714=VECTOR('',#48435,1000.);
#14715=VECTOR('',#48436,1000.);
#14716=VECTOR('',#48437,1000.);
#14717=VECTOR('',#48438,1000.);
#14718=VECTOR('',#48439,1000.);
#14719=VECTOR('',#48440,1000.);
#14720=VECTOR('',#48441,1000.);
#14721=VECTOR('',#48442,1000.);
#14722=VECTOR('',#48443,1000.);
#14723=VECTOR('',#48444,1000.);
#14724=VECTOR('',#48445,1000.);
#14725=VECTOR('',#48446,1000.);
#14726=VECTOR('',#48447,1000.);
#14727=VECTOR('',#48448,1000.);
#14728=VECTOR('',#48449,1000.);
#14729=VECTOR('',#48450,1000.);
#14730=VECTOR('',#48451,1000.);
#14731=VECTOR('',#48452,1000.);
#14732=VECTOR('',#48453,1000.);
#14733=VECTOR('',#48454,1000.);
#14734=VECTOR('',#48455,1000.);
#14735=VECTOR('',#48456,1000.);
#14736=VECTOR('',#48457,1000.);
#14737=VECTOR('',#48458,1000.);
#14738=VECTOR('',#48459,1000.);
#14739=VECTOR('',#48460,1000.);
#14740=VECTOR('',#48461,1000.);
#14741=VECTOR('',#48462,1000.);
#14742=VECTOR('',#48463,1000.);
#14743=VECTOR('',#48464,1000.);
#14744=VECTOR('',#48465,1000.);
#14745=VECTOR('',#48466,1000.);
#14746=VECTOR('',#48467,1000.);
#14747=VECTOR('',#48468,1000.);
#14748=VECTOR('',#48469,1000.);
#14749=VECTOR('',#48470,1000.);
#14750=VECTOR('',#48471,1000.);
#14751=VECTOR('',#48472,1000.);
#14752=VECTOR('',#48473,1000.);
#14753=VECTOR('',#48474,1000.);
#14754=VECTOR('',#48475,1000.);
#14755=VECTOR('',#48476,1000.);
#14756=VECTOR('',#48477,1000.);
#14757=VECTOR('',#48478,1000.);
#14758=VECTOR('',#48479,1000.);
#14759=VECTOR('',#48480,1000.);
#14760=VECTOR('',#48481,1000.);
#14761=VECTOR('',#48482,1000.);
#14762=VECTOR('',#48483,1000.);
#14763=VECTOR('',#48484,1000.);
#14764=VECTOR('',#48485,1000.);
#14765=VECTOR('',#48486,1000.);
#14766=VECTOR('',#48487,1000.);
#14767=VECTOR('',#48488,1000.);
#14768=VECTOR('',#48489,1000.);
#14769=VECTOR('',#48490,1000.);
#14770=VECTOR('',#48491,1000.);
#14771=VECTOR('',#48492,1000.);
#14772=VECTOR('',#48493,1000.);
#14773=VECTOR('',#48494,1000.);
#14774=VECTOR('',#48495,1000.);
#14775=VECTOR('',#48496,1000.);
#14776=VECTOR('',#48497,1000.);
#14777=VECTOR('',#48498,1000.);
#14778=VECTOR('',#48499,1000.);
#14779=VECTOR('',#48500,1000.);
#14780=VECTOR('',#48501,1000.);
#14781=VECTOR('',#48502,1000.);
#14782=VECTOR('',#48503,1000.);
#14783=VECTOR('',#48504,1000.);
#14784=VECTOR('',#48505,1000.);
#14785=VECTOR('',#48506,1000.);
#14786=VECTOR('',#48507,1000.);
#14787=VECTOR('',#48508,1000.);
#14788=VECTOR('',#48509,1000.);
#14789=VECTOR('',#48510,1000.);
#14790=VECTOR('',#48511,1000.);
#14791=VECTOR('',#48512,1000.);
#14792=VECTOR('',#48513,1000.);
#14793=VECTOR('',#48514,1000.);
#14794=VECTOR('',#48515,1000.);
#14795=VECTOR('',#48516,1000.);
#14796=VECTOR('',#48517,1000.);
#14797=VECTOR('',#48518,1000.);
#14798=VECTOR('',#48519,1000.);
#14799=VECTOR('',#48520,1000.);
#14800=VECTOR('',#48521,1000.);
#14801=VECTOR('',#48522,1000.);
#14802=VECTOR('',#48523,1000.);
#14803=VECTOR('',#48524,1000.);
#14804=VECTOR('',#48525,1000.);
#14805=VECTOR('',#48526,1000.);
#14806=VECTOR('',#48527,1000.);
#14807=VECTOR('',#48528,1000.);
#14808=VECTOR('',#48529,1000.);
#14809=VECTOR('',#48530,1000.);
#14810=VECTOR('',#48531,1000.);
#14811=VECTOR('',#48532,1000.);
#14812=VECTOR('',#48533,1000.);
#14813=VECTOR('',#48534,1000.);
#14814=VECTOR('',#48535,1000.);
#14815=VECTOR('',#48536,1000.);
#14816=VECTOR('',#48537,1000.);
#14817=VECTOR('',#48538,1000.);
#14818=VECTOR('',#48539,1000.);
#14819=VECTOR('',#48540,1000.);
#14820=VECTOR('',#48541,1000.);
#14821=VECTOR('',#48542,1000.);
#14822=VECTOR('',#48543,1000.);
#14823=VECTOR('',#48544,1000.);
#14824=VECTOR('',#48545,1000.);
#14825=VECTOR('',#48546,1000.);
#14826=VECTOR('',#48547,1000.);
#14827=VECTOR('',#48548,1000.);
#14828=VECTOR('',#48549,1000.);
#14829=VECTOR('',#48550,1000.);
#14830=VECTOR('',#48551,1000.);
#14831=VECTOR('',#48552,1000.);
#14832=VECTOR('',#48553,1000.);
#14833=VECTOR('',#48554,1000.);
#14834=VECTOR('',#48555,1000.);
#14835=VECTOR('',#48556,1000.);
#14836=VECTOR('',#48557,1000.);
#14837=VECTOR('',#48558,1000.);
#14838=VECTOR('',#48559,1000.);
#14839=VECTOR('',#48560,1000.);
#14840=VECTOR('',#48561,1000.);
#14841=VECTOR('',#48562,1000.);
#14842=VECTOR('',#48563,1000.);
#14843=VECTOR('',#48564,1000.);
#14844=VECTOR('',#48565,1000.);
#14845=VECTOR('',#48566,1000.);
#14846=VECTOR('',#48567,1000.);
#14847=VECTOR('',#48568,1000.);
#14848=VECTOR('',#48569,1000.);
#14849=VECTOR('',#48570,1000.);
#14850=VECTOR('',#48571,1000.);
#14851=VECTOR('',#48572,1000.);
#14852=VECTOR('',#48573,1000.);
#14853=VECTOR('',#48574,1000.);
#14854=VECTOR('',#48575,1000.);
#14855=VECTOR('',#48576,1000.);
#14856=VECTOR('',#48577,1000.);
#14857=VECTOR('',#48578,1000.);
#14858=VECTOR('',#48579,1000.);
#14859=VECTOR('',#48580,1000.);
#14860=VECTOR('',#48581,1000.);
#14861=VECTOR('',#48582,1000.);
#14862=VECTOR('',#48583,1000.);
#14863=VECTOR('',#48584,1000.);
#14864=VECTOR('',#48585,1000.);
#14865=VECTOR('',#48586,1000.);
#14866=VECTOR('',#48587,1000.);
#14867=VECTOR('',#48588,1000.);
#14868=VECTOR('',#48589,1000.);
#14869=VECTOR('',#48590,1000.);
#14870=VECTOR('',#48591,1000.);
#14871=VECTOR('',#48592,1000.);
#14872=VECTOR('',#48593,1000.);
#14873=VECTOR('',#48594,1000.);
#14874=VECTOR('',#48595,1000.);
#14875=VECTOR('',#48596,1000.);
#14876=VECTOR('',#48597,1000.);
#14877=VECTOR('',#48598,1000.);
#14878=VECTOR('',#48599,1000.);
#14879=VECTOR('',#48600,1000.);
#14880=VECTOR('',#48601,1000.);
#14881=VECTOR('',#48602,1000.);
#14882=VECTOR('',#48603,1000.);
#14883=VECTOR('',#48604,1000.);
#14884=VECTOR('',#48605,1000.);
#14885=VECTOR('',#48606,1000.);
#14886=VECTOR('',#48607,1000.);
#14887=VECTOR('',#48608,1000.);
#14888=VECTOR('',#48609,1000.);
#14889=VECTOR('',#48610,1000.);
#14890=VECTOR('',#48611,1000.);
#14891=VECTOR('',#48612,1000.);
#14892=VECTOR('',#48613,1000.);
#14893=VECTOR('',#48614,1000.);
#14894=VECTOR('',#48615,1000.);
#14895=VECTOR('',#48616,1000.);
#14896=VECTOR('',#48617,1000.);
#14897=VECTOR('',#48618,1000.);
#14898=VECTOR('',#48619,1000.);
#14899=VECTOR('',#48620,1000.);
#14900=VECTOR('',#48621,1000.);
#14901=VECTOR('',#48622,1000.);
#14902=VECTOR('',#48623,1000.);
#14903=VECTOR('',#48624,1000.);
#14904=VECTOR('',#48625,1000.);
#14905=VECTOR('',#48626,1000.);
#14906=VECTOR('',#48627,1000.);
#14907=VECTOR('',#48628,1000.);
#14908=VECTOR('',#48629,1000.);
#14909=VECTOR('',#48630,1000.);
#14910=VECTOR('',#48631,1000.);
#14911=VECTOR('',#48632,1000.);
#14912=VECTOR('',#48633,1000.);
#14913=VECTOR('',#48634,1000.);
#14914=VECTOR('',#48635,1000.);
#14915=VECTOR('',#48636,1000.);
#14916=VECTOR('',#48637,1000.);
#14917=VECTOR('',#48638,1000.);
#14918=VECTOR('',#48639,1000.);
#14919=VECTOR('',#48640,1000.);
#14920=VECTOR('',#48641,1000.);
#14921=VECTOR('',#48642,1000.);
#14922=VECTOR('',#48643,1000.);
#14923=VECTOR('',#48644,1000.);
#14924=VECTOR('',#48645,1000.);
#14925=VECTOR('',#48646,1000.);
#14926=VECTOR('',#48647,1000.);
#14927=VECTOR('',#48648,1000.);
#14928=VECTOR('',#48649,1000.);
#14929=VECTOR('',#48650,1000.);
#14930=VECTOR('',#48651,1000.);
#14931=VECTOR('',#48652,1000.);
#14932=VECTOR('',#48653,1000.);
#14933=VECTOR('',#48654,1000.);
#14934=VECTOR('',#48655,1000.);
#14935=VECTOR('',#48656,1000.);
#14936=VECTOR('',#48657,1000.);
#14937=VECTOR('',#48658,1000.);
#14938=VECTOR('',#48659,1000.);
#14939=VECTOR('',#48660,1000.);
#14940=VECTOR('',#48661,1000.);
#14941=VECTOR('',#48662,1000.);
#14942=VECTOR('',#48663,1000.);
#14943=VECTOR('',#48664,1000.);
#14944=VECTOR('',#48665,1000.);
#14945=VECTOR('',#48666,1000.);
#14946=VECTOR('',#48667,1000.);
#14947=VECTOR('',#48668,1000.);
#14948=VECTOR('',#48669,1000.);
#14949=VECTOR('',#48670,1000.);
#14950=VECTOR('',#48671,1000.);
#14951=VECTOR('',#48672,1000.);
#14952=VECTOR('',#48673,1000.);
#14953=VECTOR('',#48674,1000.);
#14954=VECTOR('',#48675,1000.);
#14955=VECTOR('',#48676,1000.);
#14956=VECTOR('',#48677,1000.);
#14957=VECTOR('',#48678,1000.);
#14958=VECTOR('',#48679,1000.);
#14959=VECTOR('',#48680,1000.);
#14960=VECTOR('',#48681,1000.);
#14961=VECTOR('',#48682,1000.);
#14962=VECTOR('',#48683,1000.);
#14963=VECTOR('',#48684,1000.);
#14964=VECTOR('',#48685,1000.);
#14965=VECTOR('',#48686,1000.);
#14966=VECTOR('',#48687,1000.);
#14967=VECTOR('',#48688,1000.);
#14968=VECTOR('',#48689,1000.);
#14969=VECTOR('',#48690,1000.);
#14970=VECTOR('',#48691,1000.);
#14971=VECTOR('',#48692,1000.);
#14972=VECTOR('',#48693,1000.);
#14973=VECTOR('',#48694,1000.);
#14974=VECTOR('',#48695,1000.);
#14975=VECTOR('',#48696,1000.);
#14976=VECTOR('',#48697,1000.);
#14977=VECTOR('',#48698,1000.);
#14978=VECTOR('',#48699,1000.);
#14979=VECTOR('',#48700,1000.);
#14980=VECTOR('',#48701,1000.);
#14981=VECTOR('',#48702,1000.);
#14982=VECTOR('',#48703,1000.);
#14983=VECTOR('',#48704,1000.);
#14984=VECTOR('',#48705,1000.);
#14985=VECTOR('',#48706,1000.);
#14986=VECTOR('',#48707,1000.);
#14987=VECTOR('',#48708,1000.);
#14988=VECTOR('',#48709,1000.);
#14989=VECTOR('',#48710,1000.);
#14990=VECTOR('',#48711,1000.);
#14991=VECTOR('',#48712,1000.);
#14992=VECTOR('',#48713,1000.);
#14993=VECTOR('',#48714,1000.);
#14994=VECTOR('',#48715,1000.);
#14995=VECTOR('',#48716,1000.);
#14996=VECTOR('',#48717,1000.);
#14997=VECTOR('',#48718,1000.);
#14998=VECTOR('',#48719,1000.);
#14999=VECTOR('',#48720,1000.);
#15000=VECTOR('',#48721,1000.);
#15001=VECTOR('',#48722,1000.);
#15002=VECTOR('',#48723,1000.);
#15003=VECTOR('',#48724,1000.);
#15004=VECTOR('',#48725,1000.);
#15005=VECTOR('',#48726,1000.);
#15006=VECTOR('',#48727,1000.);
#15007=VECTOR('',#48728,1000.);
#15008=VECTOR('',#48729,1000.);
#15009=VECTOR('',#48730,1000.);
#15010=VECTOR('',#48731,1000.);
#15011=VECTOR('',#48732,1000.);
#15012=VECTOR('',#48733,1000.);
#15013=VECTOR('',#48734,1000.);
#15014=VECTOR('',#48735,1000.);
#15015=VECTOR('',#48736,1000.);
#15016=VECTOR('',#48737,1000.);
#15017=VECTOR('',#48738,1000.);
#15018=VECTOR('',#48739,1000.);
#15019=VECTOR('',#48740,1000.);
#15020=VECTOR('',#48741,1000.);
#15021=VECTOR('',#48742,1000.);
#15022=VECTOR('',#48743,1000.);
#15023=VECTOR('',#48744,1000.);
#15024=VECTOR('',#48745,1000.);
#15025=VECTOR('',#48746,1000.);
#15026=VECTOR('',#48747,1000.);
#15027=VECTOR('',#48748,1000.);
#15028=VECTOR('',#48749,1000.);
#15029=VECTOR('',#48750,1000.);
#15030=VECTOR('',#48751,1000.);
#15031=VECTOR('',#48752,1000.);
#15032=VECTOR('',#48753,1000.);
#15033=VECTOR('',#48754,1000.);
#15034=VECTOR('',#48755,1000.);
#15035=VECTOR('',#48756,1000.);
#15036=VECTOR('',#48757,1000.);
#15037=VECTOR('',#48758,1000.);
#15038=VECTOR('',#48759,1000.);
#15039=VECTOR('',#48760,1000.);
#15040=VECTOR('',#48761,1000.);
#15041=VECTOR('',#48762,1000.);
#15042=VECTOR('',#48763,1000.);
#15043=VECTOR('',#48764,1000.);
#15044=VECTOR('',#48765,1000.);
#15045=VECTOR('',#48766,1000.);
#15046=VECTOR('',#48767,1000.);
#15047=VECTOR('',#48768,1000.);
#15048=VECTOR('',#48769,1000.);
#15049=VECTOR('',#48770,1000.);
#15050=VECTOR('',#48771,1000.);
#15051=VECTOR('',#48772,1000.);
#15052=VECTOR('',#48773,1000.);
#15053=VECTOR('',#48774,1000.);
#15054=VECTOR('',#48775,1000.);
#15055=VECTOR('',#48776,1000.);
#15056=VECTOR('',#48777,1000.);
#15057=VECTOR('',#48778,1000.);
#15058=VECTOR('',#48779,1000.);
#15059=VECTOR('',#48780,1000.);
#15060=VECTOR('',#48781,1000.);
#15061=VECTOR('',#48782,1000.);
#15062=VECTOR('',#48783,1000.);
#15063=VECTOR('',#48784,1000.);
#15064=VECTOR('',#48785,1000.);
#15065=VECTOR('',#48786,1000.);
#15066=VECTOR('',#48787,1000.);
#15067=VECTOR('',#48788,1000.);
#15068=VECTOR('',#48789,1000.);
#15069=VECTOR('',#48790,1000.);
#15070=VECTOR('',#48791,1000.);
#15071=VECTOR('',#48792,1000.);
#15072=VECTOR('',#48793,1000.);
#15073=VECTOR('',#48794,1000.);
#15074=VECTOR('',#48795,1000.);
#15075=VECTOR('',#48796,1000.);
#15076=VECTOR('',#48797,1000.);
#15077=VECTOR('',#48798,1000.);
#15078=VECTOR('',#48799,1000.);
#15079=VECTOR('',#48800,1000.);
#15080=VECTOR('',#48801,1000.);
#15081=VECTOR('',#48802,1000.);
#15082=VECTOR('',#48803,1000.);
#15083=VECTOR('',#48804,1000.);
#15084=VECTOR('',#48805,1000.);
#15085=VECTOR('',#48806,1000.);
#15086=VECTOR('',#48807,1000.);
#15087=VECTOR('',#48808,1000.);
#15088=VECTOR('',#48809,1000.);
#15089=VECTOR('',#48810,1000.);
#15090=VECTOR('',#48811,1000.);
#15091=VECTOR('',#48812,1000.);
#15092=VECTOR('',#48813,1000.);
#15093=VECTOR('',#48814,1000.);
#15094=VECTOR('',#48815,1000.);
#15095=VECTOR('',#48816,1000.);
#15096=VECTOR('',#48817,1000.);
#15097=VECTOR('',#48818,1000.);
#15098=VECTOR('',#48819,1000.);
#15099=VECTOR('',#48820,1000.);
#15100=VECTOR('',#48821,1000.);
#15101=VECTOR('',#48822,1000.);
#15102=VECTOR('',#48823,1000.);
#15103=VECTOR('',#48824,1000.);
#15104=VECTOR('',#48825,1000.);
#15105=VECTOR('',#48826,1000.);
#15106=VECTOR('',#48827,1000.);
#15107=VECTOR('',#48828,1000.);
#15108=VECTOR('',#48829,1000.);
#15109=VECTOR('',#48830,1000.);
#15110=VECTOR('',#48831,1000.);
#15111=VECTOR('',#48832,1000.);
#15112=VECTOR('',#48833,1000.);
#15113=VECTOR('',#48834,1000.);
#15114=VECTOR('',#48835,1000.);
#15115=VECTOR('',#48836,1000.);
#15116=VECTOR('',#48837,1000.);
#15117=VECTOR('',#48838,1000.);
#15118=VECTOR('',#48839,1000.);
#15119=VECTOR('',#48840,1000.);
#15120=VECTOR('',#48841,1000.);
#15121=VECTOR('',#48842,1000.);
#15122=VECTOR('',#48843,1000.);
#15123=VECTOR('',#48844,1000.);
#15124=VECTOR('',#48845,1000.);
#15125=VECTOR('',#48846,1000.);
#15126=VECTOR('',#48847,1000.);
#15127=VECTOR('',#48848,1000.);
#15128=VECTOR('',#48849,1000.);
#15129=VECTOR('',#48850,1000.);
#15130=VECTOR('',#48851,1000.);
#15131=VECTOR('',#48852,1000.);
#15132=VECTOR('',#48853,1000.);
#15133=VECTOR('',#48854,1000.);
#15134=VECTOR('',#48855,1000.);
#15135=VECTOR('',#48856,1000.);
#15136=VECTOR('',#48857,1000.);
#15137=VECTOR('',#48858,1000.);
#15138=VECTOR('',#48859,1000.);
#15139=VECTOR('',#48860,1000.);
#15140=VECTOR('',#48861,1000.);
#15141=VECTOR('',#48862,1000.);
#15142=VECTOR('',#48863,1000.);
#15143=VECTOR('',#48864,1000.);
#15144=VECTOR('',#48865,1000.);
#15145=VECTOR('',#48866,1000.);
#15146=VECTOR('',#48867,1000.);
#15147=VECTOR('',#48868,1000.);
#15148=VECTOR('',#48869,1000.);
#15149=VECTOR('',#48870,1000.);
#15150=VECTOR('',#48871,1000.);
#15151=VECTOR('',#48872,1000.);
#15152=VECTOR('',#48873,1000.);
#15153=VECTOR('',#48874,1000.);
#15154=VECTOR('',#48875,1000.);
#15155=VECTOR('',#48876,1000.);
#15156=VECTOR('',#48877,1000.);
#15157=VECTOR('',#48878,1000.);
#15158=VECTOR('',#48879,1000.);
#15159=VECTOR('',#48880,1000.);
#15160=VECTOR('',#48881,1000.);
#15161=VECTOR('',#48882,1000.);
#15162=VECTOR('',#48883,1000.);
#15163=VECTOR('',#48884,1000.);
#15164=VECTOR('',#48885,1000.);
#15165=VECTOR('',#48886,1000.);
#15166=VECTOR('',#48887,1000.);
#15167=VECTOR('',#48888,1000.);
#15168=VECTOR('',#48889,1000.);
#15169=VECTOR('',#48890,1000.);
#15170=VECTOR('',#48891,1000.);
#15171=VECTOR('',#48892,1000.);
#15172=VECTOR('',#48893,1000.);
#15173=VECTOR('',#48894,1000.);
#15174=VECTOR('',#48895,1000.);
#15175=VECTOR('',#48896,1000.);
#15176=VECTOR('',#48897,1000.);
#15177=VECTOR('',#48898,1000.);
#15178=VECTOR('',#48899,1000.);
#15179=VECTOR('',#48900,1000.);
#15180=VECTOR('',#48901,1000.);
#15181=VECTOR('',#48902,1000.);
#15182=VECTOR('',#48903,1000.);
#15183=VECTOR('',#48904,1000.);
#15184=VECTOR('',#48905,1000.);
#15185=VECTOR('',#48906,1000.);
#15186=VECTOR('',#48907,1000.);
#15187=VECTOR('',#48908,1000.);
#15188=VECTOR('',#48909,1000.);
#15189=VECTOR('',#48910,1000.);
#15190=VECTOR('',#48911,1000.);
#15191=VECTOR('',#48912,1000.);
#15192=VECTOR('',#48913,1000.);
#15193=VECTOR('',#48914,1000.);
#15194=VECTOR('',#48915,1000.);
#15195=VECTOR('',#48916,1000.);
#15196=VECTOR('',#48917,1000.);
#15197=VECTOR('',#48918,1000.);
#15198=VECTOR('',#48919,1000.);
#15199=VECTOR('',#48920,1000.);
#15200=VECTOR('',#48921,1000.);
#15201=VECTOR('',#48922,1000.);
#15202=VECTOR('',#48923,1000.);
#15203=VECTOR('',#48924,1000.);
#15204=VECTOR('',#48925,1000.);
#15205=VECTOR('',#48926,1000.);
#15206=VECTOR('',#48927,1000.);
#15207=VECTOR('',#48928,1000.);
#15208=VECTOR('',#48929,1000.);
#15209=VECTOR('',#48930,1000.);
#15210=VECTOR('',#48931,1000.);
#15211=VECTOR('',#48932,1000.);
#15212=VECTOR('',#48933,1000.);
#15213=VECTOR('',#48934,1000.);
#15214=VECTOR('',#48935,1000.);
#15215=VECTOR('',#48936,1000.);
#15216=VECTOR('',#48937,1000.);
#15217=VECTOR('',#48938,1000.);
#15218=VECTOR('',#48939,1000.);
#15219=VECTOR('',#48940,1000.);
#15220=VECTOR('',#48941,1000.);
#15221=VECTOR('',#48942,1000.);
#15222=VECTOR('',#48943,1000.);
#15223=VECTOR('',#48944,1000.);
#15224=VECTOR('',#48945,1000.);
#15225=VECTOR('',#48946,1000.);
#15226=VECTOR('',#48947,1000.);
#15227=VECTOR('',#48948,1000.);
#15228=VECTOR('',#48949,1000.);
#15229=VECTOR('',#48950,1000.);
#15230=VECTOR('',#48951,1000.);
#15231=VECTOR('',#48952,1000.);
#15232=VECTOR('',#48953,1000.);
#15233=VECTOR('',#48954,1000.);
#15234=VECTOR('',#48955,1000.);
#15235=VECTOR('',#48956,1000.);
#15236=VECTOR('',#48957,1000.);
#15237=VECTOR('',#48958,1000.);
#15238=VECTOR('',#48959,1000.);
#15239=VECTOR('',#48960,1000.);
#15240=VECTOR('',#48961,1000.);
#15241=VECTOR('',#48962,1000.);
#15242=VECTOR('',#48963,1000.);
#15243=VECTOR('',#48964,1000.);
#15244=VECTOR('',#48965,1000.);
#15245=VECTOR('',#48966,1000.);
#15246=VECTOR('',#48967,1000.);
#15247=VECTOR('',#48968,1000.);
#15248=VECTOR('',#48969,1000.);
#15249=VECTOR('',#48970,1000.);
#15250=VECTOR('',#48971,1000.);
#15251=VECTOR('',#48972,1000.);
#15252=VECTOR('',#48973,1000.);
#15253=VECTOR('',#48974,1000.);
#15254=VECTOR('',#48975,1000.);
#15255=VECTOR('',#48976,1000.);
#15256=VECTOR('',#48977,1000.);
#15257=VECTOR('',#48978,1000.);
#15258=VECTOR('',#48979,1000.);
#15259=VECTOR('',#48980,1000.);
#15260=VECTOR('',#48981,1000.);
#15261=VECTOR('',#48982,1000.);
#15262=VECTOR('',#48983,1000.);
#15263=VECTOR('',#48984,1000.);
#15264=VECTOR('',#48985,1000.);
#15265=VECTOR('',#48986,1000.);
#15266=VECTOR('',#48987,1000.);
#15267=VECTOR('',#48988,1000.);
#15268=VECTOR('',#48989,1000.);
#15269=VECTOR('',#48990,1000.);
#15270=VECTOR('',#48991,1000.);
#15271=VECTOR('',#48992,1000.);
#15272=VECTOR('',#48993,1000.);
#15273=VECTOR('',#48994,1000.);
#15274=VECTOR('',#48995,1000.);
#15275=VECTOR('',#48996,1000.);
#15276=VECTOR('',#48997,1000.);
#15277=VECTOR('',#48998,1000.);
#15278=VECTOR('',#48999,1000.);
#15279=VECTOR('',#49000,1000.);
#15280=VECTOR('',#49001,1000.);
#15281=VECTOR('',#49002,1000.);
#15282=VECTOR('',#49003,1000.);
#15283=VECTOR('',#49004,1000.);
#15284=VECTOR('',#49005,1000.);
#15285=VECTOR('',#49006,1000.);
#15286=VECTOR('',#49007,1000.);
#15287=VECTOR('',#49008,1000.);
#15288=VECTOR('',#49009,1000.);
#15289=VECTOR('',#49010,1000.);
#15290=VECTOR('',#49011,1000.);
#15291=VECTOR('',#49012,1000.);
#15292=VECTOR('',#49013,1000.);
#15293=VECTOR('',#49014,1000.);
#15294=VECTOR('',#49015,1000.);
#15295=VECTOR('',#49016,1000.);
#15296=VECTOR('',#49017,1000.);
#15297=VECTOR('',#49018,1000.);
#15298=VECTOR('',#49019,1000.);
#15299=VECTOR('',#49020,1000.);
#15300=VECTOR('',#49021,1000.);
#15301=VECTOR('',#49022,1000.);
#15302=VECTOR('',#49023,1000.);
#15303=VECTOR('',#49024,1000.);
#15304=VECTOR('',#49025,1000.);
#15305=VECTOR('',#49026,1000.);
#15306=VECTOR('',#49027,1000.);
#15307=VECTOR('',#49028,1000.);
#15308=VECTOR('',#49029,1000.);
#15309=VECTOR('',#49030,1000.);
#15310=VECTOR('',#49031,1000.);
#15311=VECTOR('',#49032,1000.);
#15312=VECTOR('',#49033,1000.);
#15313=VECTOR('',#49034,1000.);
#15314=VECTOR('',#49035,1000.);
#15315=VECTOR('',#49036,1000.);
#15316=VECTOR('',#49037,1000.);
#15317=VECTOR('',#49038,1000.);
#15318=VECTOR('',#49039,1000.);
#15319=VECTOR('',#49040,1000.);
#15320=VECTOR('',#49041,1000.);
#15321=VECTOR('',#49042,1000.);
#15322=VECTOR('',#49043,1000.);
#15323=VECTOR('',#49044,1000.);
#15324=VECTOR('',#49045,1000.);
#15325=VECTOR('',#49046,1000.);
#15326=VECTOR('',#49047,1000.);
#15327=VECTOR('',#49048,1000.);
#15328=VECTOR('',#49049,1000.);
#15329=VECTOR('',#49050,1000.);
#15330=VECTOR('',#49051,1000.);
#15331=VECTOR('',#49052,1000.);
#15332=VECTOR('',#49053,1000.);
#15333=VECTOR('',#49054,1000.);
#15334=VECTOR('',#49055,1000.);
#15335=VECTOR('',#49056,1000.);
#15336=VECTOR('',#49057,1000.);
#15337=VECTOR('',#49058,1000.);
#15338=VECTOR('',#49059,1000.);
#15339=VECTOR('',#49060,1000.);
#15340=VECTOR('',#49061,1000.);
#15341=VECTOR('',#49062,1000.);
#15342=VECTOR('',#49063,1000.);
#15343=VECTOR('',#49064,1000.);
#15344=VECTOR('',#49065,1000.);
#15345=VECTOR('',#49066,1000.);
#15346=VECTOR('',#49067,1000.);
#15347=VECTOR('',#49068,1000.);
#15348=VECTOR('',#49069,1000.);
#15349=VECTOR('',#49070,1000.);
#15350=VECTOR('',#49071,1000.);
#15351=VECTOR('',#49072,1000.);
#15352=VECTOR('',#49073,1000.);
#15353=VECTOR('',#49074,1000.);
#15354=VECTOR('',#49075,1000.);
#15355=VECTOR('',#49076,1000.);
#15356=VECTOR('',#49077,1000.);
#15357=VECTOR('',#49078,1000.);
#15358=VECTOR('',#49079,1000.);
#15359=VECTOR('',#49080,1000.);
#15360=VECTOR('',#49081,1000.);
#15361=VECTOR('',#49082,1000.);
#15362=VECTOR('',#49083,1000.);
#15363=VECTOR('',#49084,1000.);
#15364=VECTOR('',#49085,1000.);
#15365=VECTOR('',#49086,1000.);
#15366=VECTOR('',#49087,1000.);
#15367=VECTOR('',#49088,1000.);
#15368=VECTOR('',#49089,1000.);
#15369=VECTOR('',#49090,1000.);
#15370=VECTOR('',#49091,1000.);
#15371=VECTOR('',#49092,1000.);
#15372=VECTOR('',#49093,1000.);
#15373=VECTOR('',#49094,1000.);
#15374=VECTOR('',#49097,1000.);
#15375=VECTOR('',#49098,1000.);
#15376=VECTOR('',#49101,1000.);
#15377=VECTOR('',#49104,1000.);
#15378=VECTOR('',#49107,1000.);
#15379=VECTOR('',#49110,1000.);
#15380=VECTOR('',#49115,1000.);
#15381=VECTOR('',#49116,1000.);
#15382=VECTOR('',#49119,1000.);
#15383=VECTOR('',#49122,1000.);
#15384=VECTOR('',#49125,1000.);
#15385=VECTOR('',#49128,1000.);
#15386=VECTOR('',#49133,1000.);
#15387=VECTOR('',#49134,1000.);
#15388=VECTOR('',#49137,1000.);
#15389=VECTOR('',#49140,1000.);
#15390=VECTOR('',#49143,1000.);
#15391=VECTOR('',#49146,1000.);
#15392=VECTOR('',#49151,1000.);
#15393=VECTOR('',#49152,1000.);
#15394=VECTOR('',#49155,1000.);
#15395=VECTOR('',#49158,1000.);
#15396=VECTOR('',#49161,1000.);
#15397=VECTOR('',#49164,1000.);
#15398=VECTOR('',#49169,1000.);
#15399=VECTOR('',#49170,1000.);
#15400=VECTOR('',#49173,1000.);
#15401=VECTOR('',#49176,1000.);
#15402=VECTOR('',#49179,1000.);
#15403=VECTOR('',#49182,1000.);
#15404=VECTOR('',#49187,1000.);
#15405=VECTOR('',#49188,1000.);
#15406=VECTOR('',#49191,1000.);
#15407=VECTOR('',#49194,1000.);
#15408=VECTOR('',#49197,1000.);
#15409=VECTOR('',#49200,1000.);
#15410=VECTOR('',#49205,1000.);
#15411=VECTOR('',#49206,1000.);
#15412=VECTOR('',#49209,1000.);
#15413=VECTOR('',#49212,1000.);
#15414=VECTOR('',#49215,1000.);
#15415=VECTOR('',#49218,1000.);
#15416=VECTOR('',#49223,1000.);
#15417=VECTOR('',#49224,1000.);
#15418=VECTOR('',#49227,1000.);
#15419=VECTOR('',#49230,1000.);
#15420=VECTOR('',#49233,1000.);
#15421=VECTOR('',#49236,1000.);
#15422=VECTOR('',#49241,1000.);
#15423=VECTOR('',#49242,1000.);
#15424=VECTOR('',#49245,1000.);
#15425=VECTOR('',#49248,1000.);
#15426=VECTOR('',#49251,1000.);
#15427=VECTOR('',#49254,1000.);
#15428=VECTOR('',#49259,1000.);
#15429=VECTOR('',#49260,1000.);
#15430=VECTOR('',#49263,1000.);
#15431=VECTOR('',#49266,1000.);
#15432=VECTOR('',#49269,1000.);
#15433=VECTOR('',#49272,1000.);
#15434=VECTOR('',#49277,1000.);
#15435=VECTOR('',#49278,1000.);
#15436=VECTOR('',#49281,1000.);
#15437=VECTOR('',#49284,1000.);
#15438=VECTOR('',#49287,1000.);
#15439=VECTOR('',#49290,1000.);
#15440=VECTOR('',#49295,1000.);
#15441=VECTOR('',#49296,1000.);
#15442=VECTOR('',#49299,1000.);
#15443=VECTOR('',#49302,1000.);
#15444=VECTOR('',#49305,1000.);
#15445=VECTOR('',#49308,1000.);
#15446=VECTOR('',#49313,1000.);
#15447=VECTOR('',#49314,1000.);
#15448=VECTOR('',#49317,1000.);
#15449=VECTOR('',#49320,1000.);
#15450=VECTOR('',#49323,1000.);
#15451=VECTOR('',#49326,1000.);
#15452=VECTOR('',#49331,1000.);
#15453=VECTOR('',#49332,1000.);
#15454=VECTOR('',#49335,1000.);
#15455=VECTOR('',#49338,1000.);
#15456=VECTOR('',#49341,1000.);
#15457=VECTOR('',#49344,1000.);
#15458=VECTOR('',#49349,1000.);
#15459=VECTOR('',#49350,1000.);
#15460=VECTOR('',#49353,1000.);
#15461=VECTOR('',#49356,1000.);
#15462=VECTOR('',#49359,1000.);
#15463=VECTOR('',#49362,1000.);
#15464=VECTOR('',#49367,1000.);
#15465=VECTOR('',#49368,1000.);
#15466=VECTOR('',#49371,1000.);
#15467=VECTOR('',#49374,1000.);
#15468=VECTOR('',#49377,1000.);
#15469=VECTOR('',#49380,1000.);
#15470=VECTOR('',#49385,1000.);
#15471=VECTOR('',#49386,1000.);
#15472=VECTOR('',#49389,1000.);
#15473=VECTOR('',#49392,1000.);
#15474=VECTOR('',#49395,1000.);
#15475=VECTOR('',#49398,1000.);
#15476=VECTOR('',#49403,1000.);
#15477=VECTOR('',#49404,1000.);
#15478=VECTOR('',#49407,1000.);
#15479=VECTOR('',#49410,1000.);
#15480=VECTOR('',#49413,1000.);
#15481=VECTOR('',#49416,1000.);
#15482=VECTOR('',#49421,1000.);
#15483=VECTOR('',#49422,1000.);
#15484=VECTOR('',#49425,1000.);
#15485=VECTOR('',#49428,1000.);
#15486=VECTOR('',#49431,1000.);
#15487=VECTOR('',#49434,1000.);
#15488=VECTOR('',#49439,1000.);
#15489=VECTOR('',#49440,1000.);
#15490=VECTOR('',#49443,1000.);
#15491=VECTOR('',#49446,1000.);
#15492=VECTOR('',#49449,1000.);
#15493=VECTOR('',#49452,1000.);
#15494=VECTOR('',#49457,1000.);
#15495=VECTOR('',#49458,1000.);
#15496=VECTOR('',#49461,1000.);
#15497=VECTOR('',#49464,1000.);
#15498=VECTOR('',#49467,1000.);
#15499=VECTOR('',#49470,1000.);
#15500=VECTOR('',#49475,1000.);
#15501=VECTOR('',#49476,1000.);
#15502=VECTOR('',#49479,1000.);
#15503=VECTOR('',#49482,1000.);
#15504=VECTOR('',#49485,1000.);
#15505=VECTOR('',#49488,1000.);
#15506=VECTOR('',#49493,1000.);
#15507=VECTOR('',#49494,1000.);
#15508=VECTOR('',#49497,1000.);
#15509=VECTOR('',#49500,1000.);
#15510=VECTOR('',#49503,1000.);
#15511=VECTOR('',#49506,1000.);
#15512=VECTOR('',#49511,1000.);
#15513=VECTOR('',#49512,1000.);
#15514=VECTOR('',#49515,1000.);
#15515=VECTOR('',#49518,1000.);
#15516=VECTOR('',#49521,1000.);
#15517=VECTOR('',#49524,1000.);
#15518=VECTOR('',#49529,1000.);
#15519=VECTOR('',#49530,1000.);
#15520=VECTOR('',#49533,1000.);
#15521=VECTOR('',#49536,1000.);
#15522=VECTOR('',#49539,1000.);
#15523=VECTOR('',#49542,1000.);
#15524=VECTOR('',#49547,1000.);
#15525=VECTOR('',#49548,1000.);
#15526=VECTOR('',#49551,1000.);
#15527=VECTOR('',#49554,1000.);
#15528=VECTOR('',#49557,1000.);
#15529=VECTOR('',#49560,1000.);
#15530=VECTOR('',#49565,1000.);
#15531=VECTOR('',#49566,1000.);
#15532=VECTOR('',#49569,1000.);
#15533=VECTOR('',#49572,1000.);
#15534=VECTOR('',#49575,1000.);
#15535=VECTOR('',#49578,1000.);
#15536=VECTOR('',#49583,1000.);
#15537=VECTOR('',#49584,1000.);
#15538=VECTOR('',#49587,1000.);
#15539=VECTOR('',#49590,1000.);
#15540=VECTOR('',#49593,1000.);
#15541=VECTOR('',#49596,1000.);
#15542=VECTOR('',#49601,1000.);
#15543=VECTOR('',#49602,1000.);
#15544=VECTOR('',#49605,1000.);
#15545=VECTOR('',#49608,1000.);
#15546=VECTOR('',#49611,1000.);
#15547=VECTOR('',#49614,1000.);
#15548=VECTOR('',#49619,1000.);
#15549=VECTOR('',#49620,1000.);
#15550=VECTOR('',#49623,1000.);
#15551=VECTOR('',#49626,1000.);
#15552=VECTOR('',#49629,1000.);
#15553=VECTOR('',#49632,1000.);
#15554=VECTOR('',#49637,1000.);
#15555=VECTOR('',#49638,1000.);
#15556=VECTOR('',#49641,1000.);
#15557=VECTOR('',#49644,1000.);
#15558=VECTOR('',#49647,1000.);
#15559=VECTOR('',#49650,1000.);
#15560=VECTOR('',#49655,1000.);
#15561=VECTOR('',#49656,1000.);
#15562=VECTOR('',#49659,1000.);
#15563=VECTOR('',#49662,1000.);
#15564=VECTOR('',#49665,1000.);
#15565=VECTOR('',#49668,1000.);
#15566=VECTOR('',#49673,1000.);
#15567=VECTOR('',#49674,1000.);
#15568=VECTOR('',#49677,1000.);
#15569=VECTOR('',#49680,1000.);
#15570=VECTOR('',#49683,1000.);
#15571=VECTOR('',#49686,1000.);
#15572=VECTOR('',#49691,1000.);
#15573=VECTOR('',#49692,1000.);
#15574=VECTOR('',#49695,1000.);
#15575=VECTOR('',#49698,1000.);
#15576=VECTOR('',#49701,1000.);
#15577=VECTOR('',#49704,1000.);
#15578=VECTOR('',#49709,1000.);
#15579=VECTOR('',#49710,1000.);
#15580=VECTOR('',#49713,1000.);
#15581=VECTOR('',#49716,1000.);
#15582=VECTOR('',#49719,1000.);
#15583=VECTOR('',#49722,1000.);
#15584=VECTOR('',#49727,1000.);
#15585=VECTOR('',#49728,1000.);
#15586=VECTOR('',#49731,1000.);
#15587=VECTOR('',#49734,1000.);
#15588=VECTOR('',#49737,1000.);
#15589=VECTOR('',#49740,1000.);
#15590=VECTOR('',#49745,1000.);
#15591=VECTOR('',#49746,1000.);
#15592=VECTOR('',#49749,1000.);
#15593=VECTOR('',#49752,1000.);
#15594=VECTOR('',#49755,1000.);
#15595=VECTOR('',#49758,1000.);
#15596=VECTOR('',#49763,1000.);
#15597=VECTOR('',#49764,1000.);
#15598=VECTOR('',#49767,1000.);
#15599=VECTOR('',#49770,1000.);
#15600=VECTOR('',#49773,1000.);
#15601=VECTOR('',#49776,1000.);
#15602=VECTOR('',#49781,1000.);
#15603=VECTOR('',#49782,1000.);
#15604=VECTOR('',#49785,1000.);
#15605=VECTOR('',#49788,1000.);
#15606=VECTOR('',#49791,1000.);
#15607=VECTOR('',#49794,1000.);
#15608=VECTOR('',#49799,1000.);
#15609=VECTOR('',#49800,1000.);
#15610=VECTOR('',#49803,1000.);
#15611=VECTOR('',#49806,1000.);
#15612=VECTOR('',#49809,1000.);
#15613=VECTOR('',#49812,1000.);
#15614=VECTOR('',#49817,1000.);
#15615=VECTOR('',#49818,1000.);
#15616=VECTOR('',#49821,1000.);
#15617=VECTOR('',#49824,1000.);
#15618=VECTOR('',#49827,1000.);
#15619=VECTOR('',#49830,1000.);
#15620=VECTOR('',#49835,1000.);
#15621=VECTOR('',#49836,1000.);
#15622=VECTOR('',#49839,1000.);
#15623=VECTOR('',#49842,1000.);
#15624=VECTOR('',#49845,1000.);
#15625=VECTOR('',#49848,1000.);
#15626=VECTOR('',#49853,1000.);
#15627=VECTOR('',#49854,1000.);
#15628=VECTOR('',#49857,1000.);
#15629=VECTOR('',#49860,1000.);
#15630=VECTOR('',#49863,1000.);
#15631=VECTOR('',#49866,1000.);
#15632=VECTOR('',#49871,1000.);
#15633=VECTOR('',#49872,1000.);
#15634=VECTOR('',#49875,1000.);
#15635=VECTOR('',#49878,1000.);
#15636=VECTOR('',#49881,1000.);
#15637=VECTOR('',#49884,1000.);
#15638=VECTOR('',#49889,1000.);
#15639=VECTOR('',#49890,1000.);
#15640=VECTOR('',#49893,1000.);
#15641=VECTOR('',#49896,1000.);
#15642=VECTOR('',#49899,1000.);
#15643=VECTOR('',#49902,1000.);
#15644=VECTOR('',#49907,1000.);
#15645=VECTOR('',#49908,1000.);
#15646=VECTOR('',#49911,1000.);
#15647=VECTOR('',#49914,1000.);
#15648=VECTOR('',#49917,1000.);
#15649=VECTOR('',#49920,1000.);
#15650=VECTOR('',#49925,1000.);
#15651=VECTOR('',#49926,1000.);
#15652=VECTOR('',#49929,1000.);
#15653=VECTOR('',#49932,1000.);
#15654=VECTOR('',#49935,1000.);
#15655=VECTOR('',#49938,1000.);
#15656=VECTOR('',#49943,1000.);
#15657=VECTOR('',#49944,1000.);
#15658=VECTOR('',#49947,1000.);
#15659=VECTOR('',#49950,1000.);
#15660=VECTOR('',#49953,1000.);
#15661=VECTOR('',#49956,1000.);
#15662=VECTOR('',#49961,1000.);
#15663=VECTOR('',#49962,1000.);
#15664=VECTOR('',#49965,1000.);
#15665=VECTOR('',#49968,1000.);
#15666=VECTOR('',#49971,1000.);
#15667=VECTOR('',#49974,1000.);
#15668=VECTOR('',#49979,1000.);
#15669=VECTOR('',#49980,1000.);
#15670=VECTOR('',#49983,1000.);
#15671=VECTOR('',#49986,1000.);
#15672=VECTOR('',#49989,1000.);
#15673=VECTOR('',#49992,1000.);
#15674=VECTOR('',#49997,1000.);
#15675=VECTOR('',#49998,1000.);
#15676=VECTOR('',#50001,1000.);
#15677=VECTOR('',#50004,1000.);
#15678=VECTOR('',#50007,1000.);
#15679=VECTOR('',#50010,1000.);
#15680=VECTOR('',#50015,1000.);
#15681=VECTOR('',#50016,1000.);
#15682=VECTOR('',#50019,1000.);
#15683=VECTOR('',#50022,1000.);
#15684=VECTOR('',#50025,1000.);
#15685=VECTOR('',#50028,1000.);
#15686=VECTOR('',#50033,1000.);
#15687=VECTOR('',#50034,1000.);
#15688=VECTOR('',#50037,1000.);
#15689=VECTOR('',#50040,1000.);
#15690=VECTOR('',#50043,1000.);
#15691=VECTOR('',#50046,1000.);
#15692=VECTOR('',#50051,1000.);
#15693=VECTOR('',#50052,1000.);
#15694=VECTOR('',#50055,1000.);
#15695=VECTOR('',#50058,1000.);
#15696=VECTOR('',#50061,1000.);
#15697=VECTOR('',#50064,1000.);
#15698=VECTOR('',#50069,1000.);
#15699=VECTOR('',#50070,1000.);
#15700=VECTOR('',#50073,1000.);
#15701=VECTOR('',#50076,1000.);
#15702=VECTOR('',#50079,1000.);
#15703=VECTOR('',#50082,1000.);
#15704=VECTOR('',#50087,1000.);
#15705=VECTOR('',#50088,1000.);
#15706=VECTOR('',#50091,1000.);
#15707=VECTOR('',#50094,1000.);
#15708=VECTOR('',#50097,1000.);
#15709=VECTOR('',#50100,1000.);
#15710=VECTOR('',#50105,1000.);
#15711=VECTOR('',#50106,1000.);
#15712=VECTOR('',#50109,1000.);
#15713=VECTOR('',#50112,1000.);
#15714=VECTOR('',#50115,1000.);
#15715=VECTOR('',#50118,1000.);
#15716=VECTOR('',#50123,1000.);
#15717=VECTOR('',#50124,1000.);
#15718=VECTOR('',#50127,1000.);
#15719=VECTOR('',#50130,1000.);
#15720=VECTOR('',#50133,1000.);
#15721=VECTOR('',#50136,1000.);
#15722=VECTOR('',#50141,1000.);
#15723=VECTOR('',#50142,1000.);
#15724=VECTOR('',#50145,1000.);
#15725=VECTOR('',#50148,1000.);
#15726=VECTOR('',#50151,1000.);
#15727=VECTOR('',#50154,1000.);
#15728=VECTOR('',#50159,1000.);
#15729=VECTOR('',#50160,1000.);
#15730=VECTOR('',#50163,1000.);
#15731=VECTOR('',#50166,1000.);
#15732=VECTOR('',#50169,1000.);
#15733=VECTOR('',#50172,1000.);
#15734=VECTOR('',#50177,1000.);
#15735=VECTOR('',#50178,1000.);
#15736=VECTOR('',#50181,1000.);
#15737=VECTOR('',#50184,1000.);
#15738=VECTOR('',#50187,1000.);
#15739=VECTOR('',#50190,1000.);
#15740=VECTOR('',#50195,1000.);
#15741=VECTOR('',#50196,1000.);
#15742=VECTOR('',#50199,1000.);
#15743=VECTOR('',#50202,1000.);
#15744=VECTOR('',#50205,1000.);
#15745=VECTOR('',#50208,1000.);
#15746=VECTOR('',#50213,1000.);
#15747=VECTOR('',#50214,1000.);
#15748=VECTOR('',#50217,1000.);
#15749=VECTOR('',#50220,1000.);
#15750=VECTOR('',#50223,1000.);
#15751=VECTOR('',#50226,1000.);
#15752=VECTOR('',#50231,1000.);
#15753=VECTOR('',#50232,1000.);
#15754=VECTOR('',#50235,1000.);
#15755=VECTOR('',#50238,1000.);
#15756=VECTOR('',#50241,1000.);
#15757=VECTOR('',#50244,1000.);
#15758=VECTOR('',#50249,1000.);
#15759=VECTOR('',#50250,1000.);
#15760=VECTOR('',#50253,1000.);
#15761=VECTOR('',#50256,1000.);
#15762=VECTOR('',#50259,1000.);
#15763=VECTOR('',#50262,1000.);
#15764=VECTOR('',#50267,1000.);
#15765=VECTOR('',#50268,1000.);
#15766=VECTOR('',#50271,1000.);
#15767=VECTOR('',#50274,1000.);
#15768=VECTOR('',#50277,1000.);
#15769=VECTOR('',#50280,1000.);
#15770=VECTOR('',#50285,1000.);
#15771=VECTOR('',#50286,1000.);
#15772=VECTOR('',#50289,1000.);
#15773=VECTOR('',#50292,1000.);
#15774=VECTOR('',#50295,1000.);
#15775=VECTOR('',#50298,1000.);
#15776=VECTOR('',#50303,1000.);
#15777=VECTOR('',#50304,1000.);
#15778=VECTOR('',#50307,1000.);
#15779=VECTOR('',#50310,1000.);
#15780=VECTOR('',#50313,1000.);
#15781=VECTOR('',#50316,1000.);
#15782=VECTOR('',#50321,1000.);
#15783=VECTOR('',#50322,1000.);
#15784=VECTOR('',#50325,1000.);
#15785=VECTOR('',#50328,1000.);
#15786=VECTOR('',#50331,1000.);
#15787=VECTOR('',#50334,1000.);
#15788=VECTOR('',#50339,1000.);
#15789=VECTOR('',#50340,1000.);
#15790=VECTOR('',#50343,1000.);
#15791=VECTOR('',#50346,1000.);
#15792=VECTOR('',#50349,1000.);
#15793=VECTOR('',#50352,1000.);
#15794=VECTOR('',#50357,1000.);
#15795=VECTOR('',#50358,1000.);
#15796=VECTOR('',#50361,1000.);
#15797=VECTOR('',#50364,1000.);
#15798=VECTOR('',#50367,1000.);
#15799=VECTOR('',#50370,1000.);
#15800=VECTOR('',#50375,1000.);
#15801=VECTOR('',#50376,1000.);
#15802=VECTOR('',#50379,1000.);
#15803=VECTOR('',#50382,1000.);
#15804=VECTOR('',#50385,1000.);
#15805=VECTOR('',#50388,1000.);
#15806=VECTOR('',#50393,1000.);
#15807=VECTOR('',#50394,1000.);
#15808=VECTOR('',#50397,1000.);
#15809=VECTOR('',#50400,1000.);
#15810=VECTOR('',#50403,1000.);
#15811=VECTOR('',#50406,1000.);
#15812=VECTOR('',#50411,1000.);
#15813=VECTOR('',#50412,1000.);
#15814=VECTOR('',#50415,1000.);
#15815=VECTOR('',#50418,1000.);
#15816=VECTOR('',#50421,1000.);
#15817=VECTOR('',#50424,1000.);
#15818=VECTOR('',#50429,1000.);
#15819=VECTOR('',#50430,1000.);
#15820=VECTOR('',#50433,1000.);
#15821=VECTOR('',#50436,1000.);
#15822=VECTOR('',#50439,1000.);
#15823=VECTOR('',#50442,1000.);
#15824=VECTOR('',#50447,1000.);
#15825=VECTOR('',#50448,1000.);
#15826=VECTOR('',#50451,1000.);
#15827=VECTOR('',#50454,1000.);
#15828=VECTOR('',#50457,1000.);
#15829=VECTOR('',#50460,1000.);
#15830=VECTOR('',#50465,1000.);
#15831=VECTOR('',#50466,1000.);
#15832=VECTOR('',#50469,1000.);
#15833=VECTOR('',#50472,1000.);
#15834=VECTOR('',#50475,1000.);
#15835=VECTOR('',#50478,1000.);
#15836=VECTOR('',#50483,1000.);
#15837=VECTOR('',#50484,1000.);
#15838=VECTOR('',#50487,1000.);
#15839=VECTOR('',#50490,1000.);
#15840=VECTOR('',#50493,1000.);
#15841=VECTOR('',#50496,1000.);
#15842=VECTOR('',#50501,1000.);
#15843=VECTOR('',#50502,1000.);
#15844=VECTOR('',#50505,1000.);
#15845=VECTOR('',#50508,1000.);
#15846=VECTOR('',#50511,1000.);
#15847=VECTOR('',#50514,1000.);
#15848=VECTOR('',#50519,1000.);
#15849=VECTOR('',#50520,1000.);
#15850=VECTOR('',#50523,1000.);
#15851=VECTOR('',#50526,1000.);
#15852=VECTOR('',#50529,1000.);
#15853=VECTOR('',#50532,1000.);
#15854=VECTOR('',#50537,1000.);
#15855=VECTOR('',#50538,1000.);
#15856=VECTOR('',#50541,1000.);
#15857=VECTOR('',#50544,1000.);
#15858=VECTOR('',#50547,1000.);
#15859=VECTOR('',#50550,1000.);
#15860=VECTOR('',#50555,1000.);
#15861=VECTOR('',#50556,1000.);
#15862=VECTOR('',#50559,1000.);
#15863=VECTOR('',#50562,1000.);
#15864=VECTOR('',#50565,1000.);
#15865=VECTOR('',#50568,1000.);
#15866=VECTOR('',#50573,1000.);
#15867=VECTOR('',#50574,1000.);
#15868=VECTOR('',#50577,1000.);
#15869=VECTOR('',#50580,1000.);
#15870=VECTOR('',#50583,1000.);
#15871=VECTOR('',#50586,1000.);
#15872=VECTOR('',#50591,1000.);
#15873=VECTOR('',#50592,1000.);
#15874=VECTOR('',#50595,1000.);
#15875=VECTOR('',#50598,1000.);
#15876=VECTOR('',#50601,1000.);
#15877=VECTOR('',#50604,1000.);
#15878=VECTOR('',#50609,1000.);
#15879=VECTOR('',#50610,1000.);
#15880=VECTOR('',#50613,1000.);
#15881=VECTOR('',#50616,1000.);
#15882=VECTOR('',#50619,1000.);
#15883=VECTOR('',#50622,1000.);
#15884=VECTOR('',#50627,1000.);
#15885=VECTOR('',#50628,1000.);
#15886=VECTOR('',#50631,1000.);
#15887=VECTOR('',#50634,1000.);
#15888=VECTOR('',#50637,1000.);
#15889=VECTOR('',#50640,1000.);
#15890=VECTOR('',#50645,1000.);
#15891=VECTOR('',#50646,1000.);
#15892=VECTOR('',#50649,1000.);
#15893=VECTOR('',#50652,1000.);
#15894=VECTOR('',#50655,1000.);
#15895=VECTOR('',#50658,1000.);
#15896=VECTOR('',#50663,1000.);
#15897=VECTOR('',#50664,1000.);
#15898=VECTOR('',#50667,1000.);
#15899=VECTOR('',#50670,1000.);
#15900=VECTOR('',#50673,1000.);
#15901=VECTOR('',#50676,1000.);
#15902=VECTOR('',#50681,1000.);
#15903=VECTOR('',#50682,1000.);
#15904=VECTOR('',#50685,1000.);
#15905=VECTOR('',#50688,1000.);
#15906=VECTOR('',#50691,1000.);
#15907=VECTOR('',#50694,1000.);
#15908=VECTOR('',#50699,1000.);
#15909=VECTOR('',#50700,1000.);
#15910=VECTOR('',#50703,1000.);
#15911=VECTOR('',#50706,1000.);
#15912=VECTOR('',#50709,1000.);
#15913=VECTOR('',#50712,1000.);
#15914=VECTOR('',#50717,1000.);
#15915=VECTOR('',#50718,1000.);
#15916=VECTOR('',#50721,1000.);
#15917=VECTOR('',#50724,1000.);
#15918=VECTOR('',#50727,1000.);
#15919=VECTOR('',#50730,1000.);
#15920=VECTOR('',#50735,1000.);
#15921=VECTOR('',#50736,1000.);
#15922=VECTOR('',#50739,1000.);
#15923=VECTOR('',#50742,1000.);
#15924=VECTOR('',#50745,1000.);
#15925=VECTOR('',#50748,1000.);
#15926=VECTOR('',#50753,1000.);
#15927=VECTOR('',#50754,1000.);
#15928=VECTOR('',#50757,1000.);
#15929=VECTOR('',#50760,1000.);
#15930=VECTOR('',#50763,1000.);
#15931=VECTOR('',#50766,1000.);
#15932=VECTOR('',#50771,1000.);
#15933=VECTOR('',#50772,1000.);
#15934=VECTOR('',#50775,1000.);
#15935=VECTOR('',#50778,1000.);
#15936=VECTOR('',#50781,1000.);
#15937=VECTOR('',#50784,1000.);
#15938=VECTOR('',#50789,1000.);
#15939=VECTOR('',#50790,1000.);
#15940=VECTOR('',#50793,1000.);
#15941=VECTOR('',#50796,1000.);
#15942=VECTOR('',#50799,1000.);
#15943=VECTOR('',#50802,1000.);
#15944=VECTOR('',#50807,1000.);
#15945=VECTOR('',#50808,1000.);
#15946=VECTOR('',#50811,1000.);
#15947=VECTOR('',#50814,1000.);
#15948=VECTOR('',#50817,1000.);
#15949=VECTOR('',#50820,1000.);
#15950=VECTOR('',#50825,1000.);
#15951=VECTOR('',#50826,1000.);
#15952=VECTOR('',#50829,1000.);
#15953=VECTOR('',#50832,1000.);
#15954=VECTOR('',#50835,1000.);
#15955=VECTOR('',#50838,1000.);
#15956=VECTOR('',#50843,1000.);
#15957=VECTOR('',#50844,1000.);
#15958=VECTOR('',#50847,1000.);
#15959=VECTOR('',#50850,1000.);
#15960=VECTOR('',#50853,1000.);
#15961=VECTOR('',#50856,1000.);
#15962=VECTOR('',#50861,1000.);
#15963=VECTOR('',#50862,1000.);
#15964=VECTOR('',#50865,1000.);
#15965=VECTOR('',#50868,1000.);
#15966=VECTOR('',#50871,1000.);
#15967=VECTOR('',#50874,1000.);
#15968=VECTOR('',#50879,1000.);
#15969=VECTOR('',#50880,1000.);
#15970=VECTOR('',#50883,1000.);
#15971=VECTOR('',#50886,1000.);
#15972=VECTOR('',#50889,1000.);
#15973=VECTOR('',#50892,1000.);
#15974=VECTOR('',#50897,1000.);
#15975=VECTOR('',#50898,1000.);
#15976=VECTOR('',#50901,1000.);
#15977=VECTOR('',#50904,1000.);
#15978=VECTOR('',#50907,1000.);
#15979=VECTOR('',#50910,1000.);
#15980=VECTOR('',#50915,1000.);
#15981=VECTOR('',#50916,1000.);
#15982=VECTOR('',#50919,1000.);
#15983=VECTOR('',#50922,1000.);
#15984=VECTOR('',#50925,1000.);
#15985=VECTOR('',#50928,1000.);
#15986=VECTOR('',#50933,1000.);
#15987=VECTOR('',#50934,1000.);
#15988=VECTOR('',#50937,1000.);
#15989=VECTOR('',#50940,1000.);
#15990=VECTOR('',#50943,1000.);
#15991=VECTOR('',#50946,1000.);
#15992=VECTOR('',#50951,1000.);
#15993=VECTOR('',#50952,1000.);
#15994=VECTOR('',#50955,1000.);
#15995=VECTOR('',#50958,1000.);
#15996=VECTOR('',#50961,1000.);
#15997=VECTOR('',#50964,1000.);
#15998=VECTOR('',#50969,1000.);
#15999=VECTOR('',#50970,1000.);
#16000=VECTOR('',#50973,1000.);
#16001=VECTOR('',#50976,1000.);
#16002=VECTOR('',#50979,1000.);
#16003=VECTOR('',#50982,1000.);
#16004=VECTOR('',#50987,1000.);
#16005=VECTOR('',#50988,1000.);
#16006=VECTOR('',#50991,1000.);
#16007=VECTOR('',#50994,1000.);
#16008=VECTOR('',#50997,1000.);
#16009=VECTOR('',#51000,1000.);
#16010=VECTOR('',#51005,1000.);
#16011=VECTOR('',#51006,1000.);
#16012=VECTOR('',#51009,1000.);
#16013=VECTOR('',#51012,1000.);
#16014=VECTOR('',#51015,1000.);
#16015=VECTOR('',#51018,1000.);
#16016=VECTOR('',#51023,1000.);
#16017=VECTOR('',#51024,1000.);
#16018=VECTOR('',#51027,1000.);
#16019=VECTOR('',#51030,1000.);
#16020=VECTOR('',#51033,1000.);
#16021=VECTOR('',#51036,1000.);
#16022=VECTOR('',#51041,1000.);
#16023=VECTOR('',#51042,1000.);
#16024=VECTOR('',#51045,1000.);
#16025=VECTOR('',#51048,1000.);
#16026=VECTOR('',#51051,1000.);
#16027=VECTOR('',#51054,1000.);
#16028=VECTOR('',#51059,1000.);
#16029=VECTOR('',#51060,1000.);
#16030=VECTOR('',#51063,1000.);
#16031=VECTOR('',#51066,1000.);
#16032=VECTOR('',#51069,1000.);
#16033=VECTOR('',#51072,1000.);
#16034=VECTOR('',#51077,1000.);
#16035=VECTOR('',#51078,1000.);
#16036=VECTOR('',#51081,1000.);
#16037=VECTOR('',#51084,1000.);
#16038=VECTOR('',#51087,1000.);
#16039=VECTOR('',#51090,1000.);
#16040=VECTOR('',#51095,1000.);
#16041=VECTOR('',#51096,1000.);
#16042=VECTOR('',#51099,1000.);
#16043=VECTOR('',#51102,1000.);
#16044=VECTOR('',#51105,1000.);
#16045=VECTOR('',#51108,1000.);
#16046=VECTOR('',#51113,1000.);
#16047=VECTOR('',#51114,1000.);
#16048=VECTOR('',#51117,1000.);
#16049=VECTOR('',#51120,1000.);
#16050=VECTOR('',#51123,1000.);
#16051=VECTOR('',#51126,1000.);
#16052=VECTOR('',#51131,1000.);
#16053=VECTOR('',#51132,1000.);
#16054=VECTOR('',#51135,1000.);
#16055=VECTOR('',#51138,1000.);
#16056=VECTOR('',#51141,1000.);
#16057=VECTOR('',#51144,1000.);
#16058=VECTOR('',#51149,1000.);
#16059=VECTOR('',#51150,1000.);
#16060=VECTOR('',#51153,1000.);
#16061=VECTOR('',#51156,1000.);
#16062=VECTOR('',#51159,1000.);
#16063=VECTOR('',#51162,1000.);
#16064=VECTOR('',#51167,1000.);
#16065=VECTOR('',#51168,1000.);
#16066=VECTOR('',#51171,1000.);
#16067=VECTOR('',#51174,1000.);
#16068=VECTOR('',#51177,1000.);
#16069=VECTOR('',#51180,1000.);
#16070=VECTOR('',#51185,1000.);
#16071=VECTOR('',#51186,1000.);
#16072=VECTOR('',#51189,1000.);
#16073=VECTOR('',#51192,1000.);
#16074=VECTOR('',#51195,1000.);
#16075=VECTOR('',#51198,1000.);
#16076=VECTOR('',#51203,1000.);
#16077=VECTOR('',#51204,1000.);
#16078=VECTOR('',#51207,1000.);
#16079=VECTOR('',#51210,1000.);
#16080=VECTOR('',#51213,1000.);
#16081=VECTOR('',#51216,1000.);
#16082=VECTOR('',#51221,1000.);
#16083=VECTOR('',#51222,1000.);
#16084=VECTOR('',#51225,1000.);
#16085=VECTOR('',#51228,1000.);
#16086=VECTOR('',#51231,1000.);
#16087=VECTOR('',#51234,1000.);
#16088=VECTOR('',#51239,1000.);
#16089=VECTOR('',#51240,1000.);
#16090=VECTOR('',#51243,1000.);
#16091=VECTOR('',#51246,1000.);
#16092=VECTOR('',#51249,1000.);
#16093=VECTOR('',#51252,1000.);
#16094=VECTOR('',#51257,1000.);
#16095=VECTOR('',#51258,1000.);
#16096=VECTOR('',#51261,1000.);
#16097=VECTOR('',#51264,1000.);
#16098=VECTOR('',#51267,1000.);
#16099=VECTOR('',#51270,1000.);
#16100=VECTOR('',#51275,1000.);
#16101=VECTOR('',#51276,1000.);
#16102=VECTOR('',#51279,1000.);
#16103=VECTOR('',#51282,1000.);
#16104=VECTOR('',#51285,1000.);
#16105=VECTOR('',#51288,1000.);
#16106=VECTOR('',#51293,1000.);
#16107=VECTOR('',#51294,1000.);
#16108=VECTOR('',#51297,1000.);
#16109=VECTOR('',#51300,1000.);
#16110=VECTOR('',#51303,1000.);
#16111=VECTOR('',#51306,1000.);
#16112=VECTOR('',#51311,1000.);
#16113=VECTOR('',#51312,1000.);
#16114=VECTOR('',#51315,1000.);
#16115=VECTOR('',#51318,1000.);
#16116=VECTOR('',#51321,1000.);
#16117=VECTOR('',#51324,1000.);
#16118=VECTOR('',#51329,1000.);
#16119=VECTOR('',#51330,1000.);
#16120=VECTOR('',#51333,1000.);
#16121=VECTOR('',#51336,1000.);
#16122=VECTOR('',#51339,1000.);
#16123=VECTOR('',#51342,1000.);
#16124=VECTOR('',#51347,1000.);
#16125=VECTOR('',#51348,1000.);
#16126=VECTOR('',#51351,1000.);
#16127=VECTOR('',#51354,1000.);
#16128=VECTOR('',#51357,1000.);
#16129=VECTOR('',#51360,1000.);
#16130=VECTOR('',#51365,1000.);
#16131=VECTOR('',#51366,1000.);
#16132=VECTOR('',#51369,1000.);
#16133=VECTOR('',#51372,1000.);
#16134=VECTOR('',#51375,1000.);
#16135=VECTOR('',#51378,1000.);
#16136=VECTOR('',#51383,1000.);
#16137=VECTOR('',#51384,1000.);
#16138=VECTOR('',#51387,1000.);
#16139=VECTOR('',#51390,1000.);
#16140=VECTOR('',#51393,1000.);
#16141=VECTOR('',#51396,1000.);
#16142=VECTOR('',#51401,1000.);
#16143=VECTOR('',#51402,1000.);
#16144=VECTOR('',#51405,1000.);
#16145=VECTOR('',#51408,1000.);
#16146=VECTOR('',#51411,1000.);
#16147=VECTOR('',#51414,1000.);
#16148=VECTOR('',#51419,1000.);
#16149=VECTOR('',#51420,1000.);
#16150=VECTOR('',#51423,1000.);
#16151=VECTOR('',#51426,1000.);
#16152=VECTOR('',#51429,1000.);
#16153=VECTOR('',#51432,1000.);
#16154=VECTOR('',#51437,1000.);
#16155=VECTOR('',#51438,1000.);
#16156=VECTOR('',#51441,1000.);
#16157=VECTOR('',#51444,1000.);
#16158=VECTOR('',#51447,1000.);
#16159=VECTOR('',#51450,1000.);
#16160=VECTOR('',#51455,1000.);
#16161=VECTOR('',#51456,1000.);
#16162=VECTOR('',#51459,1000.);
#16163=VECTOR('',#51462,1000.);
#16164=VECTOR('',#51465,1000.);
#16165=VECTOR('',#51468,1000.);
#16166=VECTOR('',#51473,1000.);
#16167=VECTOR('',#51474,1000.);
#16168=VECTOR('',#51477,1000.);
#16169=VECTOR('',#51480,1000.);
#16170=VECTOR('',#51483,1000.);
#16171=VECTOR('',#51486,1000.);
#16172=VECTOR('',#51491,1000.);
#16173=VECTOR('',#51492,1000.);
#16174=VECTOR('',#51495,1000.);
#16175=VECTOR('',#51498,1000.);
#16176=VECTOR('',#51501,1000.);
#16177=VECTOR('',#51504,1000.);
#16178=VECTOR('',#51509,1000.);
#16179=VECTOR('',#51510,1000.);
#16180=VECTOR('',#51513,1000.);
#16181=VECTOR('',#51516,1000.);
#16182=VECTOR('',#51519,1000.);
#16183=VECTOR('',#51522,1000.);
#16184=VECTOR('',#51527,1000.);
#16185=VECTOR('',#51528,1000.);
#16186=VECTOR('',#51531,1000.);
#16187=VECTOR('',#51534,1000.);
#16188=VECTOR('',#51537,1000.);
#16189=VECTOR('',#51540,1000.);
#16190=VECTOR('',#51545,1000.);
#16191=VECTOR('',#51546,1000.);
#16192=VECTOR('',#51549,1000.);
#16193=VECTOR('',#51552,1000.);
#16194=VECTOR('',#51555,1000.);
#16195=VECTOR('',#51558,1000.);
#16196=VECTOR('',#51563,1000.);
#16197=VECTOR('',#51564,1000.);
#16198=VECTOR('',#51567,1000.);
#16199=VECTOR('',#51570,1000.);
#16200=VECTOR('',#51573,1000.);
#16201=VECTOR('',#51576,1000.);
#16202=VECTOR('',#51581,1000.);
#16203=VECTOR('',#51582,1000.);
#16204=VECTOR('',#51585,1000.);
#16205=VECTOR('',#51588,1000.);
#16206=VECTOR('',#51591,1000.);
#16207=VECTOR('',#51594,1000.);
#16208=VECTOR('',#51599,1000.);
#16209=VECTOR('',#51600,1000.);
#16210=VECTOR('',#51603,1000.);
#16211=VECTOR('',#51606,1000.);
#16212=VECTOR('',#51609,1000.);
#16213=VECTOR('',#51612,1000.);
#16214=VECTOR('',#51617,1000.);
#16215=VECTOR('',#51618,1000.);
#16216=VECTOR('',#51621,1000.);
#16217=VECTOR('',#51624,1000.);
#16218=VECTOR('',#51627,1000.);
#16219=VECTOR('',#51630,1000.);
#16220=VECTOR('',#51635,1000.);
#16221=VECTOR('',#51636,1000.);
#16222=VECTOR('',#51639,1000.);
#16223=VECTOR('',#51642,1000.);
#16224=VECTOR('',#51645,1000.);
#16225=VECTOR('',#51648,1000.);
#16226=VECTOR('',#51653,1000.);
#16227=VECTOR('',#51654,1000.);
#16228=VECTOR('',#51657,1000.);
#16229=VECTOR('',#51660,1000.);
#16230=VECTOR('',#51663,1000.);
#16231=VECTOR('',#51666,1000.);
#16232=VECTOR('',#51671,1000.);
#16233=VECTOR('',#51672,1000.);
#16234=VECTOR('',#51675,1000.);
#16235=VECTOR('',#51678,1000.);
#16236=VECTOR('',#51681,1000.);
#16237=VECTOR('',#51684,1000.);
#16238=VECTOR('',#51689,1000.);
#16239=VECTOR('',#51690,1000.);
#16240=VECTOR('',#51693,1000.);
#16241=VECTOR('',#51696,1000.);
#16242=VECTOR('',#51699,1000.);
#16243=VECTOR('',#51702,1000.);
#16244=VECTOR('',#51707,1000.);
#16245=VECTOR('',#51708,1000.);
#16246=VECTOR('',#51711,1000.);
#16247=VECTOR('',#51714,1000.);
#16248=VECTOR('',#51717,1000.);
#16249=VECTOR('',#51720,1000.);
#16250=VECTOR('',#51725,1000.);
#16251=VECTOR('',#51726,1000.);
#16252=VECTOR('',#51729,1000.);
#16253=VECTOR('',#51732,1000.);
#16254=VECTOR('',#51735,1000.);
#16255=VECTOR('',#51738,1000.);
#16256=VECTOR('',#51743,1000.);
#16257=VECTOR('',#51744,1000.);
#16258=VECTOR('',#51747,1000.);
#16259=VECTOR('',#51750,1000.);
#16260=VECTOR('',#51753,1000.);
#16261=VECTOR('',#51756,1000.);
#16262=VECTOR('',#51761,1000.);
#16263=VECTOR('',#51762,1000.);
#16264=VECTOR('',#51765,1000.);
#16265=VECTOR('',#51768,1000.);
#16266=VECTOR('',#51771,1000.);
#16267=VECTOR('',#51774,1000.);
#16268=VECTOR('',#51779,1000.);
#16269=VECTOR('',#51780,1000.);
#16270=VECTOR('',#51783,1000.);
#16271=VECTOR('',#51786,1000.);
#16272=VECTOR('',#51789,1000.);
#16273=VECTOR('',#51792,1000.);
#16274=VECTOR('',#51797,1000.);
#16275=VECTOR('',#51798,1000.);
#16276=VECTOR('',#51801,1000.);
#16277=VECTOR('',#51804,1000.);
#16278=VECTOR('',#51807,1000.);
#16279=VECTOR('',#51810,1000.);
#16280=VECTOR('',#51815,1000.);
#16281=VECTOR('',#51816,1000.);
#16282=VECTOR('',#51819,1000.);
#16283=VECTOR('',#51822,1000.);
#16284=VECTOR('',#51825,1000.);
#16285=VECTOR('',#51828,1000.);
#16286=VECTOR('',#51833,1000.);
#16287=VECTOR('',#51834,1000.);
#16288=VECTOR('',#51837,1000.);
#16289=VECTOR('',#51840,1000.);
#16290=VECTOR('',#51843,1000.);
#16291=VECTOR('',#51846,1000.);
#16292=VECTOR('',#51851,1000.);
#16293=VECTOR('',#51852,1000.);
#16294=VECTOR('',#51855,1000.);
#16295=VECTOR('',#51858,1000.);
#16296=VECTOR('',#51861,1000.);
#16297=VECTOR('',#51864,1000.);
#16298=VECTOR('',#51869,1000.);
#16299=VECTOR('',#51870,1000.);
#16300=VECTOR('',#51873,1000.);
#16301=VECTOR('',#51876,1000.);
#16302=VECTOR('',#51879,1000.);
#16303=VECTOR('',#51882,1000.);
#16304=VECTOR('',#51887,1000.);
#16305=VECTOR('',#51888,1000.);
#16306=VECTOR('',#51891,1000.);
#16307=VECTOR('',#51894,1000.);
#16308=VECTOR('',#51897,1000.);
#16309=VECTOR('',#51900,1000.);
#16310=VECTOR('',#51905,1000.);
#16311=VECTOR('',#51906,1000.);
#16312=VECTOR('',#51909,1000.);
#16313=VECTOR('',#51912,1000.);
#16314=VECTOR('',#51915,1000.);
#16315=VECTOR('',#51918,1000.);
#16316=VECTOR('',#51923,1000.);
#16317=VECTOR('',#51924,1000.);
#16318=VECTOR('',#51927,1000.);
#16319=VECTOR('',#51930,1000.);
#16320=VECTOR('',#51933,1000.);
#16321=VECTOR('',#51936,1000.);
#16322=VECTOR('',#51941,1000.);
#16323=VECTOR('',#51942,1000.);
#16324=VECTOR('',#51945,1000.);
#16325=VECTOR('',#51948,1000.);
#16326=VECTOR('',#51951,1000.);
#16327=VECTOR('',#51954,1000.);
#16328=VECTOR('',#51959,1000.);
#16329=VECTOR('',#51960,1000.);
#16330=VECTOR('',#51963,1000.);
#16331=VECTOR('',#51966,1000.);
#16332=VECTOR('',#51969,1000.);
#16333=VECTOR('',#51972,1000.);
#16334=VECTOR('',#51977,1000.);
#16335=VECTOR('',#51978,1000.);
#16336=VECTOR('',#51981,1000.);
#16337=VECTOR('',#51984,1000.);
#16338=VECTOR('',#51987,1000.);
#16339=VECTOR('',#51990,1000.);
#16340=VECTOR('',#51995,1000.);
#16341=VECTOR('',#51996,1000.);
#16342=VECTOR('',#51999,1000.);
#16343=VECTOR('',#52002,1000.);
#16344=VECTOR('',#52005,1000.);
#16345=VECTOR('',#52008,1000.);
#16346=VECTOR('',#52013,1000.);
#16347=VECTOR('',#52014,1000.);
#16348=VECTOR('',#52017,1000.);
#16349=VECTOR('',#52020,1000.);
#16350=VECTOR('',#52023,1000.);
#16351=VECTOR('',#52026,1000.);
#16352=VECTOR('',#52031,1000.);
#16353=VECTOR('',#52032,1000.);
#16354=VECTOR('',#52035,1000.);
#16355=VECTOR('',#52038,1000.);
#16356=VECTOR('',#52041,1000.);
#16357=VECTOR('',#52044,1000.);
#16358=VECTOR('',#52049,1000.);
#16359=VECTOR('',#52050,1000.);
#16360=VECTOR('',#52053,1000.);
#16361=VECTOR('',#52056,1000.);
#16362=VECTOR('',#52059,1000.);
#16363=VECTOR('',#52062,1000.);
#16364=VECTOR('',#52067,1000.);
#16365=VECTOR('',#52068,1000.);
#16366=VECTOR('',#52071,1000.);
#16367=VECTOR('',#52074,1000.);
#16368=VECTOR('',#52077,1000.);
#16369=VECTOR('',#52080,1000.);
#16370=VECTOR('',#52085,1000.);
#16371=VECTOR('',#52086,1000.);
#16372=VECTOR('',#52089,1000.);
#16373=VECTOR('',#52092,1000.);
#16374=VECTOR('',#52095,1000.);
#16375=VECTOR('',#52098,1000.);
#16376=VECTOR('',#52103,1000.);
#16377=VECTOR('',#52104,1000.);
#16378=VECTOR('',#52107,1000.);
#16379=VECTOR('',#52110,1000.);
#16380=VECTOR('',#52113,1000.);
#16381=VECTOR('',#52116,1000.);
#16382=VECTOR('',#52121,1000.);
#16383=VECTOR('',#52122,1000.);
#16384=VECTOR('',#52125,1000.);
#16385=VECTOR('',#52128,1000.);
#16386=VECTOR('',#52131,1000.);
#16387=VECTOR('',#52134,1000.);
#16388=VECTOR('',#52139,1000.);
#16389=VECTOR('',#52140,1000.);
#16390=VECTOR('',#52143,1000.);
#16391=VECTOR('',#52146,1000.);
#16392=VECTOR('',#52149,1000.);
#16393=VECTOR('',#52152,1000.);
#16394=VECTOR('',#52157,1000.);
#16395=VECTOR('',#52158,1000.);
#16396=VECTOR('',#52161,1000.);
#16397=VECTOR('',#52164,1000.);
#16398=VECTOR('',#52167,1000.);
#16399=VECTOR('',#52170,1000.);
#16400=VECTOR('',#52175,1000.);
#16401=VECTOR('',#52176,1000.);
#16402=VECTOR('',#52179,1000.);
#16403=VECTOR('',#52182,1000.);
#16404=VECTOR('',#52185,1000.);
#16405=VECTOR('',#52188,1000.);
#16406=VECTOR('',#52193,1000.);
#16407=VECTOR('',#52194,1000.);
#16408=VECTOR('',#52197,1000.);
#16409=VECTOR('',#52200,1000.);
#16410=VECTOR('',#52203,1000.);
#16411=VECTOR('',#52206,1000.);
#16412=VECTOR('',#52211,1000.);
#16413=VECTOR('',#52212,1000.);
#16414=VECTOR('',#52215,1000.);
#16415=VECTOR('',#52218,1000.);
#16416=VECTOR('',#52221,1000.);
#16417=VECTOR('',#52224,1000.);
#16418=VECTOR('',#52229,1000.);
#16419=VECTOR('',#52230,1000.);
#16420=VECTOR('',#52233,1000.);
#16421=VECTOR('',#52236,1000.);
#16422=VECTOR('',#52239,1000.);
#16423=VECTOR('',#52242,1000.);
#16424=VECTOR('',#52247,1000.);
#16425=VECTOR('',#52248,1000.);
#16426=VECTOR('',#52251,1000.);
#16427=VECTOR('',#52254,1000.);
#16428=VECTOR('',#52257,1000.);
#16429=VECTOR('',#52260,1000.);
#16430=VECTOR('',#52265,1000.);
#16431=VECTOR('',#52266,1000.);
#16432=VECTOR('',#52269,1000.);
#16433=VECTOR('',#52272,1000.);
#16434=VECTOR('',#52275,1000.);
#16435=VECTOR('',#52278,1000.);
#16436=VECTOR('',#52283,1000.);
#16437=VECTOR('',#52284,1000.);
#16438=VECTOR('',#52287,1000.);
#16439=VECTOR('',#52290,1000.);
#16440=VECTOR('',#52293,1000.);
#16441=VECTOR('',#52296,1000.);
#16442=VECTOR('',#52301,1000.);
#16443=VECTOR('',#52302,1000.);
#16444=VECTOR('',#52305,1000.);
#16445=VECTOR('',#52308,1000.);
#16446=VECTOR('',#52311,1000.);
#16447=VECTOR('',#52314,1000.);
#16448=VECTOR('',#52319,1000.);
#16449=VECTOR('',#52320,1000.);
#16450=VECTOR('',#52323,1000.);
#16451=VECTOR('',#52326,1000.);
#16452=VECTOR('',#52329,1000.);
#16453=VECTOR('',#52332,1000.);
#16454=VECTOR('',#52337,1000.);
#16455=VECTOR('',#52338,1000.);
#16456=VECTOR('',#52341,1000.);
#16457=VECTOR('',#52344,1000.);
#16458=VECTOR('',#52347,1000.);
#16459=VECTOR('',#52350,1000.);
#16460=VECTOR('',#52355,1000.);
#16461=VECTOR('',#52356,1000.);
#16462=VECTOR('',#52359,1000.);
#16463=VECTOR('',#52362,1000.);
#16464=VECTOR('',#52365,1000.);
#16465=VECTOR('',#52368,1000.);
#16466=VECTOR('',#52373,1000.);
#16467=VECTOR('',#52374,1000.);
#16468=VECTOR('',#52377,1000.);
#16469=VECTOR('',#52380,1000.);
#16470=VECTOR('',#52383,1000.);
#16471=VECTOR('',#52386,1000.);
#16472=VECTOR('',#52391,1000.);
#16473=VECTOR('',#52392,1000.);
#16474=VECTOR('',#52395,1000.);
#16475=VECTOR('',#52398,1000.);
#16476=VECTOR('',#52401,1000.);
#16477=VECTOR('',#52404,1000.);
#16478=VECTOR('',#52409,1000.);
#16479=VECTOR('',#52410,1000.);
#16480=VECTOR('',#52413,1000.);
#16481=VECTOR('',#52416,1000.);
#16482=VECTOR('',#52419,1000.);
#16483=VECTOR('',#52422,1000.);
#16484=VECTOR('',#52427,1000.);
#16485=VECTOR('',#52428,1000.);
#16486=VECTOR('',#52431,1000.);
#16487=VECTOR('',#52434,1000.);
#16488=VECTOR('',#52437,1000.);
#16489=VECTOR('',#52440,1000.);
#16490=CIRCLE('',#39986,1.75);
#16491=CIRCLE('',#39987,1.75);
#16492=CIRCLE('',#39989,1.75);
#16493=CIRCLE('',#39990,1.75);
#16494=CIRCLE('',#39992,1.75);
#16495=CIRCLE('',#39993,1.75);
#16496=CIRCLE('',#39995,1.75);
#16497=CIRCLE('',#39996,1.75);
#16498=CIRCLE('',#39998,1.25);
#16499=CIRCLE('',#39999,1.25);
#16500=CIRCLE('',#40001,1.25);
#16501=CIRCLE('',#40002,1.25);
#16502=CIRCLE('',#40004,1.5);
#16503=CIRCLE('',#40005,1.5);
#16504=CIRCLE('',#40007,1.5);
#16505=CIRCLE('',#40008,1.5);
#16506=CIRCLE('',#40010,1.5);
#16507=CIRCLE('',#40011,1.5);
#16508=CIRCLE('',#40013,1.5);
#16509=CIRCLE('',#40014,1.5);
#16510=CIRCLE('',#40016,1.5);
#16511=CIRCLE('',#40017,1.5);
#16512=CIRCLE('',#40019,1.5);
#16513=CIRCLE('',#40020,1.5);
#16514=CIRCLE('',#40022,1.5);
#16515=CIRCLE('',#40023,1.5);
#16516=CIRCLE('',#40025,1.5);
#16517=CIRCLE('',#40026,1.5);
#16518=CIRCLE('',#40028,1.5);
#16519=CIRCLE('',#40029,1.5);
#16520=CIRCLE('',#40031,1.5);
#16521=CIRCLE('',#40032,1.5);
#16522=CIRCLE('',#40034,1.5);
#16523=CIRCLE('',#40035,1.5);
#16524=CIRCLE('',#40037,1.5);
#16525=CIRCLE('',#40038,1.5);
#16526=CIRCLE('',#40040,1.5);
#16527=CIRCLE('',#40041,1.5);
#16528=CIRCLE('',#40043,1.5);
#16529=CIRCLE('',#40044,1.5);
#16530=CIRCLE('',#40046,1.5);
#16531=CIRCLE('',#40047,1.5);
#16532=CIRCLE('',#40049,1.5);
#16533=CIRCLE('',#40050,1.5);
#16534=CIRCLE('',#40052,1.5);
#16535=CIRCLE('',#40053,1.5);
#16536=CIRCLE('',#40055,1.5);
#16537=CIRCLE('',#40056,1.5);
#16538=CIRCLE('',#40058,1.5);
#16539=CIRCLE('',#40059,1.5);
#16540=CIRCLE('',#40061,1.5);
#16541=CIRCLE('',#40062,1.5);
#16542=CIRCLE('',#40064,1.5);
#16543=CIRCLE('',#40065,1.5);
#16544=CIRCLE('',#40067,1.5);
#16545=CIRCLE('',#40068,1.5);
#16546=CIRCLE('',#40070,1.5);
#16547=CIRCLE('',#40071,1.5);
#16548=CIRCLE('',#40073,1.5);
#16549=CIRCLE('',#40074,1.5);
#16550=CIRCLE('',#40076,1.5);
#16551=CIRCLE('',#40077,1.5);
#16552=CIRCLE('',#40079,1.5);
#16553=CIRCLE('',#40080,1.5);
#16554=CIRCLE('',#40082,1.5);
#16555=CIRCLE('',#40083,1.5);
#16556=CIRCLE('',#40085,1.5);
#16557=CIRCLE('',#40086,1.5);
#16558=CIRCLE('',#40088,1.5);
#16559=CIRCLE('',#40089,1.5);
#16560=CIRCLE('',#40091,1.5);
#16561=CIRCLE('',#40092,1.5);
#16562=CIRCLE('',#40094,1.5);
#16563=CIRCLE('',#40095,1.5);
#16564=CIRCLE('',#40097,1.5);
#16565=CIRCLE('',#40098,1.5);
#16566=CIRCLE('',#40100,1.5);
#16567=CIRCLE('',#40101,1.5);
#16568=CIRCLE('',#40103,1.5);
#16569=CIRCLE('',#40104,1.5);
#16570=CIRCLE('',#40106,1.5);
#16571=CIRCLE('',#40107,1.5);
#16572=CIRCLE('',#40109,1.5);
#16573=CIRCLE('',#40110,1.5);
#16574=CIRCLE('',#40112,1.5);
#16575=CIRCLE('',#40113,1.5);
#16576=CIRCLE('',#40115,1.5);
#16577=CIRCLE('',#40116,1.5);
#16578=CIRCLE('',#40118,1.5);
#16579=CIRCLE('',#40119,1.5);
#16580=CIRCLE('',#40121,1.5);
#16581=CIRCLE('',#40122,1.5);
#16582=CIRCLE('',#40124,1.5);
#16583=CIRCLE('',#40125,1.5);
#16584=CIRCLE('',#40127,1.5);
#16585=CIRCLE('',#40128,1.5);
#16586=CIRCLE('',#40130,1.5);
#16587=CIRCLE('',#40131,1.5);
#16588=CIRCLE('',#40133,1.5);
#16589=CIRCLE('',#40134,1.5);
#16590=CIRCLE('',#40136,1.5);
#16591=CIRCLE('',#40137,1.5);
#16592=CIRCLE('',#40139,1.5);
#16593=CIRCLE('',#40140,1.5);
#16594=CIRCLE('',#40142,1.5);
#16595=CIRCLE('',#40143,1.5);
#16596=CIRCLE('',#40145,1.5);
#16597=CIRCLE('',#40146,1.5);
#16598=CIRCLE('',#40148,1.5);
#16599=CIRCLE('',#40149,1.5);
#16600=CIRCLE('',#40151,1.5);
#16601=CIRCLE('',#40152,1.5);
#16602=CIRCLE('',#40154,1.5);
#16603=CIRCLE('',#40155,1.5);
#16604=CIRCLE('',#40157,1.5);
#16605=CIRCLE('',#40158,1.5);
#16606=CIRCLE('',#40160,1.5);
#16607=CIRCLE('',#40161,1.5);
#16608=CIRCLE('',#40163,1.5);
#16609=CIRCLE('',#40164,1.5);
#16610=CIRCLE('',#40166,1.5);
#16611=CIRCLE('',#40167,1.5);
#16612=CIRCLE('',#40169,1.5);
#16613=CIRCLE('',#40170,1.5);
#16614=CIRCLE('',#40172,1.5);
#16615=CIRCLE('',#40173,1.5);
#16616=CIRCLE('',#40175,1.5);
#16617=CIRCLE('',#40176,1.5);
#16618=CIRCLE('',#40178,1.5);
#16619=CIRCLE('',#40179,1.5);
#16620=CIRCLE('',#40181,1.5);
#16621=CIRCLE('',#40182,1.5);
#16622=CIRCLE('',#40184,1.5);
#16623=CIRCLE('',#40185,1.5);
#16624=CIRCLE('',#40187,1.5);
#16625=CIRCLE('',#40188,1.5);
#16626=CIRCLE('',#40190,1.5);
#16627=CIRCLE('',#40191,1.5);
#16628=CIRCLE('',#40193,1.5);
#16629=CIRCLE('',#40194,1.5);
#16630=CIRCLE('',#40196,1.5);
#16631=CIRCLE('',#40197,1.5);
#16632=CIRCLE('',#40199,1.5);
#16633=CIRCLE('',#40200,1.5);
#16634=CIRCLE('',#40202,1.74999999999999);
#16635=CIRCLE('',#40203,1.74999999999999);
#16636=CIRCLE('',#40205,1.74999999999998);
#16637=CIRCLE('',#40206,1.74999999999998);
#16638=CIRCLE('',#40208,1.75);
#16639=CIRCLE('',#40209,1.75);
#16640=CIRCLE('',#40211,1.75);
#16641=CIRCLE('',#40212,1.75);
#16642=CIRCLE('',#40214,42.4898979485563);
#16643=CIRCLE('',#40215,0.5);
#16644=CIRCLE('',#40216,42.);
#16645=CIRCLE('',#40218,43.2737346662473);
#16646=CIRCLE('',#40219,1.2);
#16647=CIRCLE('',#40220,44.4494897427832);
#16648=CIRCLE('',#40222,42.);
#16649=CIRCLE('',#40223,1.3);
#16650=CIRCLE('',#40225,44.4494897427832);
#16651=CIRCLE('',#40226,2.);
#16652=CIRCLE('',#40228,1.25);
#16653=CIRCLE('',#40229,1.25);
#16654=CIRCLE('',#40231,1.25);
#16655=CIRCLE('',#40232,1.25);
#16656=CIRCLE('',#40234,1.25);
#16657=CIRCLE('',#40235,1.25);
#16658=CIRCLE('',#40237,1.25);
#16659=CIRCLE('',#40238,1.25);
#16660=CIRCLE('',#40240,1.5);
#16661=CIRCLE('',#40241,1.5);
#16662=CIRCLE('',#40242,1.5);
#16663=CIRCLE('',#40243,1.5);
#16664=CIRCLE('',#40245,1.5);
#16665=CIRCLE('',#40246,1.5);
#16666=CIRCLE('',#40247,1.5);
#16667=CIRCLE('',#40248,1.5);
#16668=CIRCLE('',#40252,4.);
#16669=CIRCLE('',#40253,4.);
#16670=CIRCLE('',#40255,4.);
#16671=CIRCLE('',#40256,4.);
#16672=CIRCLE('',#40260,1.5);
#16673=CIRCLE('',#40261,1.5);
#16674=CIRCLE('',#40262,1.5);
#16675=CIRCLE('',#40263,1.5);
#16676=CIRCLE('',#40264,1.5);
#16677=CIRCLE('',#40265,1.5);
#16678=CIRCLE('',#40266,1.5);
#16679=CIRCLE('',#40267,1.5);
#16680=CIRCLE('',#40268,1.5);
#16681=CIRCLE('',#40269,1.5);
#16682=CIRCLE('',#40270,1.5);
#16683=CIRCLE('',#40271,1.5);
#16684=CIRCLE('',#40272,1.5);
#16685=CIRCLE('',#40273,1.5);
#16686=CIRCLE('',#40274,1.5);
#16687=CIRCLE('',#40275,1.5);
#16688=CIRCLE('',#40276,1.5);
#16689=CIRCLE('',#40277,1.5);
#16690=CIRCLE('',#40278,1.5);
#16691=CIRCLE('',#40279,1.5);
#16692=CIRCLE('',#40280,1.5);
#16693=CIRCLE('',#40281,1.5);
#16694=CIRCLE('',#40282,1.5);
#16695=CIRCLE('',#40283,1.5);
#16696=CIRCLE('',#40284,1.5);
#16697=CIRCLE('',#40285,1.5);
#16698=CIRCLE('',#40286,1.5);
#16699=CIRCLE('',#40287,1.5);
#16700=CIRCLE('',#40288,1.5);
#16701=CIRCLE('',#40289,1.5);
#16702=CIRCLE('',#40290,1.5);
#16703=CIRCLE('',#40291,1.5);
#16704=CIRCLE('',#40292,1.5);
#16705=CIRCLE('',#40293,1.5);
#16706=CIRCLE('',#40294,1.5);
#16707=CIRCLE('',#40295,1.5);
#16708=CIRCLE('',#40296,1.5);
#16709=CIRCLE('',#40297,1.5);
#16710=CIRCLE('',#40298,1.5);
#16711=CIRCLE('',#40299,1.5);
#16712=CIRCLE('',#40300,1.5);
#16713=CIRCLE('',#40301,1.5);
#16714=CIRCLE('',#40302,1.5);
#16715=CIRCLE('',#40303,1.5);
#16716=CIRCLE('',#40304,1.5);
#16717=CIRCLE('',#40305,1.5);
#16718=CIRCLE('',#40306,1.5);
#16719=CIRCLE('',#40307,1.5);
#16720=CIRCLE('',#40308,1.5);
#16721=CIRCLE('',#40309,1.5);
#16722=CIRCLE('',#40311,1.5);
#16723=CIRCLE('',#40312,1.5);
#16724=CIRCLE('',#40313,1.5);
#16725=CIRCLE('',#40314,1.5);
#16726=CIRCLE('',#40315,1.5);
#16727=CIRCLE('',#40316,1.5);
#16728=CIRCLE('',#40317,1.5);
#16729=CIRCLE('',#40318,1.5);
#16730=CIRCLE('',#40319,1.5);
#16731=CIRCLE('',#40320,1.5);
#16732=CIRCLE('',#40321,1.5);
#16733=CIRCLE('',#40322,1.5);
#16734=CIRCLE('',#40323,1.5);
#16735=CIRCLE('',#40324,1.5);
#16736=CIRCLE('',#40325,1.5);
#16737=CIRCLE('',#40326,1.5);
#16738=CIRCLE('',#40327,1.5);
#16739=CIRCLE('',#40328,1.5);
#16740=CIRCLE('',#40329,1.5);
#16741=CIRCLE('',#40330,1.5);
#16742=CIRCLE('',#40331,1.5);
#16743=CIRCLE('',#40332,1.5);
#16744=CIRCLE('',#40333,1.5);
#16745=CIRCLE('',#40334,1.5);
#16746=CIRCLE('',#40335,1.5);
#16747=CIRCLE('',#40336,1.5);
#16748=CIRCLE('',#40337,1.5);
#16749=CIRCLE('',#40338,1.5);
#16750=CIRCLE('',#40339,1.5);
#16751=CIRCLE('',#40340,1.5);
#16752=CIRCLE('',#40341,1.5);
#16753=CIRCLE('',#40342,1.5);
#16754=CIRCLE('',#40343,1.5);
#16755=CIRCLE('',#40344,1.5);
#16756=CIRCLE('',#40345,1.5);
#16757=CIRCLE('',#40346,1.5);
#16758=CIRCLE('',#40347,1.5);
#16759=CIRCLE('',#40348,1.5);
#16760=CIRCLE('',#40349,1.5);
#16761=CIRCLE('',#40350,1.5);
#16762=CIRCLE('',#40351,1.5);
#16763=CIRCLE('',#40352,1.5);
#16764=CIRCLE('',#40353,1.5);
#16765=CIRCLE('',#40354,1.5);
#16766=CIRCLE('',#40355,1.5);
#16767=CIRCLE('',#40356,1.5);
#16768=CIRCLE('',#40357,1.5);
#16769=CIRCLE('',#40358,1.5);
#16770=CIRCLE('',#40359,1.5);
#16771=CIRCLE('',#40360,1.5);
#16772=CIRCLE('',#40386,1.5);
#16773=CIRCLE('',#40387,1.5);
#16774=CIRCLE('',#40388,1.5);
#16775=CIRCLE('',#40389,1.5);
#16776=CIRCLE('',#40390,1.5);
#16777=CIRCLE('',#40391,1.5);
#16778=CIRCLE('',#40392,1.5);
#16779=CIRCLE('',#40393,1.5);
#16780=CIRCLE('',#40394,1.5);
#16781=CIRCLE('',#40395,1.5);
#16782=CIRCLE('',#40396,1.5);
#16783=CIRCLE('',#40397,1.5);
#16784=CIRCLE('',#40398,1.5);
#16785=CIRCLE('',#40399,1.5);
#16786=CIRCLE('',#40400,1.5);
#16787=CIRCLE('',#40401,1.5);
#16788=CIRCLE('',#40402,1.5);
#16789=CIRCLE('',#40403,1.5);
#16790=CIRCLE('',#40404,1.5);
#16791=CIRCLE('',#40405,1.5);
#16792=CIRCLE('',#40406,1.5);
#16793=CIRCLE('',#40407,1.5);
#16794=CIRCLE('',#40408,1.5);
#16795=CIRCLE('',#40409,1.5);
#16796=CIRCLE('',#40410,1.5);
#16797=CIRCLE('',#40411,1.5);
#16798=CIRCLE('',#40412,1.5);
#16799=CIRCLE('',#40413,1.5);
#16800=CIRCLE('',#40414,1.5);
#16801=CIRCLE('',#40415,1.5);
#16802=CIRCLE('',#40416,1.5);
#16803=CIRCLE('',#40417,1.5);
#16804=CIRCLE('',#40418,1.5);
#16805=CIRCLE('',#40419,1.5);
#16806=CIRCLE('',#40420,1.5);
#16807=CIRCLE('',#40421,1.5);
#16808=CIRCLE('',#40422,1.5);
#16809=CIRCLE('',#40423,1.5);
#16810=CIRCLE('',#40424,1.5);
#16811=CIRCLE('',#40425,1.5);
#16812=CIRCLE('',#40426,1.5);
#16813=CIRCLE('',#40427,1.5);
#16814=CIRCLE('',#40428,1.5);
#16815=CIRCLE('',#40429,1.5);
#16816=CIRCLE('',#40430,1.5);
#16817=CIRCLE('',#40431,1.5);
#16818=CIRCLE('',#40432,1.5);
#16819=CIRCLE('',#40433,1.5);
#16820=CIRCLE('',#40434,1.5);
#16821=CIRCLE('',#40435,1.5);
#16822=CIRCLE('',#40436,1.5);
#16823=CIRCLE('',#40437,1.5);
#16824=CIRCLE('',#40438,1.5);
#16825=CIRCLE('',#40439,1.5);
#16826=CIRCLE('',#40442,1.5);
#16827=CIRCLE('',#40443,1.5);
#16828=CIRCLE('',#40444,2.667);
#16829=CIRCLE('',#40445,2.667);
#16830=CIRCLE('',#40446,2.66699999999999);
#16831=CIRCLE('',#40447,2.667);
#16832=CIRCLE('',#40448,2.667);
#16833=CIRCLE('',#40449,2.667);
#16834=CIRCLE('',#40451,1.5);
#16835=CIRCLE('',#40452,1.5);
#16836=CIRCLE('',#40453,2.667);
#16837=CIRCLE('',#40454,2.667);
#16838=CIRCLE('',#40455,2.667);
#16839=CIRCLE('',#40456,2.667);
#16840=CIRCLE('',#40457,2.66699999999999);
#16841=CIRCLE('',#40458,2.667);
#16842=CIRCLE('',#40486,2.);
#16843=CIRCLE('',#40487,2.);
#16844=CIRCLE('',#40489,2.);
#16845=CIRCLE('',#40490,2.);
#16846=CIRCLE('',#40492,2.);
#16847=CIRCLE('',#40493,2.);
#16848=CIRCLE('',#40495,2.);
#16849=CIRCLE('',#40496,2.);
#16850=CIRCLE('',#40498,1.2);
#16851=CIRCLE('',#40499,1.5);
#16852=CIRCLE('',#40500,1.5);
#16853=CIRCLE('',#40501,1.20000000000001);
#16854=CIRCLE('',#40502,2.3);
#16855=CIRCLE('',#40503,2.3);
#16856=CIRCLE('',#40505,1.20000000000001);
#16857=CIRCLE('',#40506,1.5);
#16858=CIRCLE('',#40507,1.5);
#16859=CIRCLE('',#40508,1.2);
#16860=CIRCLE('',#40509,2.3);
#16861=CIRCLE('',#40510,2.3);
#16862=CIRCLE('',#40524,2.);
#16863=CIRCLE('',#40525,2.);
#16864=CIRCLE('',#40527,2.);
#16865=CIRCLE('',#40528,2.);
#16866=CIRCLE('',#40530,2.);
#16867=CIRCLE('',#40531,2.);
#16868=CIRCLE('',#40533,2.);
#16869=CIRCLE('',#40534,2.);
#16870=CIRCLE('',#40536,1.2);
#16871=CIRCLE('',#40537,1.5);
#16872=CIRCLE('',#40538,1.5);
#16873=CIRCLE('',#40539,1.20000000000001);
#16874=CIRCLE('',#40540,2.3);
#16875=CIRCLE('',#40541,2.3);
#16876=CIRCLE('',#40543,1.20000000000001);
#16877=CIRCLE('',#40544,1.5);
#16878=CIRCLE('',#40545,1.5);
#16879=CIRCLE('',#40546,1.2);
#16880=CIRCLE('',#40547,2.3);
#16881=CIRCLE('',#40548,2.3);
#16882=CIRCLE('',#40562,2.);
#16883=CIRCLE('',#40563,2.);
#16884=CIRCLE('',#40565,2.);
#16885=CIRCLE('',#40566,2.);
#16886=CIRCLE('',#40568,2.);
#16887=CIRCLE('',#40569,2.);
#16888=CIRCLE('',#40571,2.);
#16889=CIRCLE('',#40572,2.);
#16890=CIRCLE('',#40574,1.2);
#16891=CIRCLE('',#40575,1.5);
#16892=CIRCLE('',#40576,1.5);
#16893=CIRCLE('',#40577,1.2);
#16894=CIRCLE('',#40578,2.3);
#16895=CIRCLE('',#40579,2.3);
#16896=CIRCLE('',#40581,1.2);
#16897=CIRCLE('',#40582,1.5);
#16898=CIRCLE('',#40583,1.5);
#16899=CIRCLE('',#40584,1.2);
#16900=CIRCLE('',#40585,2.3);
#16901=CIRCLE('',#40586,2.3);
#16902=CIRCLE('',#40600,2.);
#16903=CIRCLE('',#40601,2.);
#16904=CIRCLE('',#40603,2.);
#16905=CIRCLE('',#40604,2.);
#16906=CIRCLE('',#40606,2.);
#16907=CIRCLE('',#40607,2.);
#16908=CIRCLE('',#40609,2.);
#16909=CIRCLE('',#40610,2.);
#16910=CIRCLE('',#40612,1.2);
#16911=CIRCLE('',#40613,1.5);
#16912=CIRCLE('',#40614,1.5);
#16913=CIRCLE('',#40615,1.2);
#16914=CIRCLE('',#40616,2.3);
#16915=CIRCLE('',#40617,2.3);
#16916=CIRCLE('',#40619,1.2);
#16917=CIRCLE('',#40620,1.5);
#16918=CIRCLE('',#40621,1.5);
#16919=CIRCLE('',#40622,1.2);
#16920=CIRCLE('',#40623,2.3);
#16921=CIRCLE('',#40624,2.3);
#16922=CIRCLE('',#40638,1.5);
#16923=CIRCLE('',#40639,1.5);
#16924=CIRCLE('',#40640,1.5);
#16925=CIRCLE('',#40641,1.5);
#16926=CIRCLE('',#40642,1.5);
#16927=CIRCLE('',#40643,1.5);
#16928=CIRCLE('',#40644,1.5);
#16929=CIRCLE('',#40645,1.5);
#16930=CIRCLE('',#40646,1.5);
#16931=CIRCLE('',#40647,1.5);
#16932=CIRCLE('',#40648,1.5);
#16933=CIRCLE('',#40649,1.5);
#16934=CIRCLE('',#40650,1.5);
#16935=CIRCLE('',#40651,1.5);
#16936=CIRCLE('',#40652,1.5);
#16937=CIRCLE('',#40653,1.5);
#16938=CIRCLE('',#40654,1.5);
#16939=CIRCLE('',#40655,1.5);
#16940=CIRCLE('',#40656,1.5);
#16941=CIRCLE('',#40657,1.5);
#16942=CIRCLE('',#40658,1.5);
#16943=CIRCLE('',#40659,1.5);
#16944=CIRCLE('',#40660,1.5);
#16945=CIRCLE('',#40661,1.5);
#16946=CIRCLE('',#40662,1.5);
#16947=CIRCLE('',#40663,1.5);
#16948=CIRCLE('',#40664,1.5);
#16949=CIRCLE('',#40665,1.5);
#16950=CIRCLE('',#40666,1.5);
#16951=CIRCLE('',#40667,1.5);
#16952=CIRCLE('',#40668,1.5);
#16953=CIRCLE('',#40669,1.5);
#16954=CIRCLE('',#40670,1.5);
#16955=CIRCLE('',#40671,1.5);
#16956=CIRCLE('',#40672,1.5);
#16957=CIRCLE('',#40673,1.5);
#16958=CIRCLE('',#40674,1.5);
#16959=CIRCLE('',#40675,1.5);
#16960=CIRCLE('',#40676,1.5);
#16961=CIRCLE('',#40677,1.5);
#16962=CIRCLE('',#40678,1.5);
#16963=CIRCLE('',#40679,1.5);
#16964=CIRCLE('',#40680,1.5);
#16965=CIRCLE('',#40681,1.5);
#16966=CIRCLE('',#40682,1.5);
#16967=CIRCLE('',#40683,1.5);
#16968=CIRCLE('',#40684,1.5);
#16969=CIRCLE('',#40685,1.5);
#16970=CIRCLE('',#40686,1.5);
#16971=CIRCLE('',#40687,1.5);
#16972=CIRCLE('',#40688,1.5);
#16973=CIRCLE('',#40689,1.5);
#16974=CIRCLE('',#40690,1.5);
#16975=CIRCLE('',#40691,1.5);
#16976=CIRCLE('',#40928,0.799999999999995);
#16977=CIRCLE('',#40929,1.59999999999999);
#16978=CIRCLE('',#40931,0.799999999999995);
#16979=CIRCLE('',#40932,1.59999999999999);
#16980=CIRCLE('',#40941,2.);
#16981=CIRCLE('',#40942,2.);
#16982=CIRCLE('',#40944,2.);
#16983=CIRCLE('',#40945,2.);
#16984=CIRCLE('',#40947,2.);
#16985=CIRCLE('',#40948,2.);
#16986=CIRCLE('',#40950,2.);
#16987=CIRCLE('',#40951,2.);
#16988=CIRCLE('',#40953,1.20000000000001);
#16989=CIRCLE('',#40954,2.3);
#16990=CIRCLE('',#40955,2.3);
#16991=CIRCLE('',#40956,1.20000000000001);
#16992=CIRCLE('',#40957,1.5);
#16993=CIRCLE('',#40958,1.5);
#16994=CIRCLE('',#40960,1.20000000000001);
#16995=CIRCLE('',#40961,2.3);
#16996=CIRCLE('',#40962,2.3);
#16997=CIRCLE('',#40963,1.20000000000001);
#16998=CIRCLE('',#40964,1.5);
#16999=CIRCLE('',#40965,1.5);
#17000=CIRCLE('',#40979,2.);
#17001=CIRCLE('',#40980,2.);
#17002=CIRCLE('',#40982,2.);
#17003=CIRCLE('',#40983,2.);
#17004=CIRCLE('',#40985,2.);
#17005=CIRCLE('',#40986,2.);
#17006=CIRCLE('',#40988,2.);
#17007=CIRCLE('',#40989,2.);
#17008=CIRCLE('',#40991,1.2);
#17009=CIRCLE('',#40992,2.3);
#17010=CIRCLE('',#40993,2.3);
#17011=CIRCLE('',#40994,1.2);
#17012=CIRCLE('',#40995,1.5);
#17013=CIRCLE('',#40996,1.5);
#17014=CIRCLE('',#40998,1.2);
#17015=CIRCLE('',#40999,2.3);
#17016=CIRCLE('',#41000,2.3);
#17017=CIRCLE('',#41001,1.2);
#17018=CIRCLE('',#41002,1.5);
#17019=CIRCLE('',#41003,1.5);
#17020=CIRCLE('',#41023,0.799999999999995);
#17021=CIRCLE('',#41024,1.59999999999999);
#17022=CIRCLE('',#41026,0.799999999999995);
#17023=CIRCLE('',#41027,1.59999999999999);
#17024=CIRCLE('',#41033,4.);
#17025=CIRCLE('',#41034,4.);
#17026=CIRCLE('',#41036,4.);
#17027=CIRCLE('',#41037,4.);
#17028=CIRCLE('',#41043,0.800100000000001);
#17029=CIRCLE('',#41044,0.800100000000001);
#17030=CIRCLE('',#41046,0.800100000000001);
#17031=CIRCLE('',#41047,0.800100000000001);
#17032=CIRCLE('',#41049,0.800100000000001);
#17033=CIRCLE('',#41050,0.800100000000001);
#17034=CIRCLE('',#41052,1.20015);
#17035=CIRCLE('',#41053,1.20015);
#17036=CIRCLE('',#41054,1.97294590991864);
#17037=CIRCLE('',#41056,1.20015);
#17038=CIRCLE('',#41057,1.20015);
#17039=CIRCLE('',#41058,1.97294590991864);
#17040=CIRCLE('',#41060,1.20015);
#17041=CIRCLE('',#41062,3.556);
#17042=CIRCLE('',#41063,3.556);
#17043=CIRCLE('',#41065,1.20015);
#17044=CIRCLE('',#41067,2.667);
#17045=CIRCLE('',#41068,2.667);
#17046=CIRCLE('',#41069,2.667);
#17047=CIRCLE('',#41070,2.66700000000001);
#17048=CIRCLE('',#41071,2.667);
#17049=CIRCLE('',#41072,2.667);
#17050=CIRCLE('',#41086,1.778);
#17051=CIRCLE('',#41087,1.778);
#17052=CIRCLE('',#41088,1.778);
#17053=CIRCLE('',#41089,1.778);
#17054=CIRCLE('',#41090,1.778);
#17055=CIRCLE('',#41091,1.778);
#17056=CIRCLE('',#41093,3.2004);
#17057=CIRCLE('',#41094,3.2004);
#17058=CIRCLE('',#41095,3.2004);
#17059=CIRCLE('',#41096,3.2004);
#17060=CIRCLE('',#41097,1.778);
#17061=CIRCLE('',#41098,1.778);
#17062=CIRCLE('',#41099,1.778);
#17063=CIRCLE('',#41100,1.778);
#17064=CIRCLE('',#41101,1.778);
#17065=CIRCLE('',#41102,1.778);
#17066=CIRCLE('',#41104,3.556);
#17067=CIRCLE('',#41105,3.556);
#17068=CIRCLE('',#41106,3.556);
#17069=CIRCLE('',#41107,3.556);
#17070=CIRCLE('',#41108,3.556);
#17071=CIRCLE('',#41109,2.667);
#17072=CIRCLE('',#41110,2.667);
#17073=CIRCLE('',#41111,2.667);
#17074=CIRCLE('',#41112,2.66700000000001);
#17075=CIRCLE('',#41113,2.667);
#17076=CIRCLE('',#41114,2.667);
#17077=CIRCLE('',#41116,3.556);
#17078=CIRCLE('',#41117,3.556);
#17079=CIRCLE('',#41120,3.556);
#17080=CIRCLE('',#41121,3.556);
#17081=CIRCLE('',#41124,3.556);
#17082=CIRCLE('',#41125,3.556);
#17083=CIRCLE('',#41128,3.556);
#17084=CIRCLE('',#41129,3.556);
#17085=CIRCLE('',#41133,3.556);
#17086=CIRCLE('',#41140,0.3556);
#17087=CIRCLE('',#41141,0.3556);
#17088=CIRCLE('',#41143,0.3556);
#17089=CIRCLE('',#41145,0.3556);
#17090=CIRCLE('',#41147,0.3556);
#17091=CIRCLE('',#41149,0.3556);
#17092=CIRCLE('',#41151,0.3556);
#17093=CIRCLE('',#41153,0.355599999999999);
#17094=CIRCLE('',#41232,1.);
#17095=CIRCLE('',#41233,1.);
#17096=CIRCLE('',#41235,1.);
#17097=CIRCLE('',#41236,1.);
#17098=CIRCLE('',#41238,56.);
#17099=CIRCLE('',#41239,56.);
#17100=CIRCLE('',#41256,0.5);
#17101=CIRCLE('',#41257,0.5);
#17102=CIRCLE('',#41260,0.5);
#17103=CIRCLE('',#41261,0.5);
#17104=CIRCLE('',#41274,1.);
#17105=CIRCLE('',#41276,1.);
#17106=CIRCLE('',#41279,1.);
#17107=CIRCLE('',#41281,1.);
#17108=CIRCLE('',#41304,0.5);
#17109=CIRCLE('',#41306,0.5);
#17110=CIRCLE('',#41309,59.9898979485574);
#17111=CIRCLE('',#41310,0.5);
#17112=CIRCLE('',#41311,59.5);
#17113=CIRCLE('',#41313,60.7737346662472);
#17114=CIRCLE('',#41314,1.2);
#17115=CIRCLE('',#41315,61.9494897427832);
#17116=CIRCLE('',#41317,59.5);
#17117=CIRCLE('',#41318,1.3);
#17118=CIRCLE('',#41320,61.9494897427832);
#17119=CIRCLE('',#41321,2.);
#17120=CIRCLE('',#41333,0.799999999999995);
#17121=CIRCLE('',#41334,1.6);
#17122=CIRCLE('',#41336,0.799999999999995);
#17123=CIRCLE('',#41337,1.6);
#17124=CIRCLE('',#41341,0.799999999999995);
#17125=CIRCLE('',#41342,1.6);
#17126=CIRCLE('',#41344,0.799999999999995);
#17127=CIRCLE('',#41345,1.6);
#17128=CIRCLE('',#41349,5.);
#17129=CIRCLE('',#41350,5.);
#17130=CIRCLE('',#41353,5.);
#17131=CIRCLE('',#41354,5.);
#17132=CIRCLE('',#41363,0.799999999999995);
#17133=CIRCLE('',#41364,1.6);
#17134=CIRCLE('',#41366,0.799999999999995);
#17135=CIRCLE('',#41367,1.6);
#17136=CIRCLE('',#41371,0.799999999999995);
#17137=CIRCLE('',#41372,1.6);
#17138=CIRCLE('',#41374,0.799999999999995);
#17139=CIRCLE('',#41375,1.6);
#17140=CIRCLE('',#41379,5.);
#17141=CIRCLE('',#41380,5.);
#17142=CIRCLE('',#41383,5.);
#17143=CIRCLE('',#41384,5.);
#17144=VERTEX_POINT('',#52454);
#17145=VERTEX_POINT('',#52456);
#17146=VERTEX_POINT('',#52460);
#17147=VERTEX_POINT('',#52462);
#17148=VERTEX_POINT('',#52466);
#17149=VERTEX_POINT('',#52468);
#17150=VERTEX_POINT('',#52472);
#17151=VERTEX_POINT('',#52474);
#17152=VERTEX_POINT('',#52478);
#17153=VERTEX_POINT('',#52480);
#17154=VERTEX_POINT('',#52484);
#17155=VERTEX_POINT('',#52486);
#17156=VERTEX_POINT('',#52490);
#17157=VERTEX_POINT('',#52491);
#17158=VERTEX_POINT('',#52493);
#17159=VERTEX_POINT('',#52495);
#17160=VERTEX_POINT('',#52499);
#17161=VERTEX_POINT('',#52500);
#17162=VERTEX_POINT('',#52502);
#17163=VERTEX_POINT('',#52504);
#17164=VERTEX_POINT('',#52508);
#17165=VERTEX_POINT('',#52509);
#17166=VERTEX_POINT('',#52511);
#17167=VERTEX_POINT('',#52513);
#17168=VERTEX_POINT('',#52517);
#17169=VERTEX_POINT('',#52518);
#17170=VERTEX_POINT('',#52520);
#17171=VERTEX_POINT('',#52522);
#17172=VERTEX_POINT('',#52526);
#17173=VERTEX_POINT('',#52527);
#17174=VERTEX_POINT('',#52529);
#17175=VERTEX_POINT('',#52531);
#17176=VERTEX_POINT('',#52535);
#17177=VERTEX_POINT('',#52536);
#17178=VERTEX_POINT('',#52538);
#17179=VERTEX_POINT('',#52540);
#17180=VERTEX_POINT('',#52544);
#17181=VERTEX_POINT('',#52545);
#17182=VERTEX_POINT('',#52547);
#17183=VERTEX_POINT('',#52549);
#17184=VERTEX_POINT('',#52553);
#17185=VERTEX_POINT('',#52554);
#17186=VERTEX_POINT('',#52556);
#17187=VERTEX_POINT('',#52558);
#17188=VERTEX_POINT('',#52562);
#17189=VERTEX_POINT('',#52563);
#17190=VERTEX_POINT('',#52565);
#17191=VERTEX_POINT('',#52567);
#17192=VERTEX_POINT('',#52571);
#17193=VERTEX_POINT('',#52572);
#17194=VERTEX_POINT('',#52574);
#17195=VERTEX_POINT('',#52576);
#17196=VERTEX_POINT('',#52580);
#17197=VERTEX_POINT('',#52581);
#17198=VERTEX_POINT('',#52583);
#17199=VERTEX_POINT('',#52585);
#17200=VERTEX_POINT('',#52589);
#17201=VERTEX_POINT('',#52590);
#17202=VERTEX_POINT('',#52592);
#17203=VERTEX_POINT('',#52594);
#17204=VERTEX_POINT('',#52598);
#17205=VERTEX_POINT('',#52599);
#17206=VERTEX_POINT('',#52601);
#17207=VERTEX_POINT('',#52603);
#17208=VERTEX_POINT('',#52607);
#17209=VERTEX_POINT('',#52608);
#17210=VERTEX_POINT('',#52610);
#17211=VERTEX_POINT('',#52612);
#17212=VERTEX_POINT('',#52616);
#17213=VERTEX_POINT('',#52617);
#17214=VERTEX_POINT('',#52619);
#17215=VERTEX_POINT('',#52621);
#17216=VERTEX_POINT('',#52625);
#17217=VERTEX_POINT('',#52626);
#17218=VERTEX_POINT('',#52628);
#17219=VERTEX_POINT('',#52630);
#17220=VERTEX_POINT('',#52634);
#17221=VERTEX_POINT('',#52635);
#17222=VERTEX_POINT('',#52637);
#17223=VERTEX_POINT('',#52639);
#17224=VERTEX_POINT('',#52643);
#17225=VERTEX_POINT('',#52644);
#17226=VERTEX_POINT('',#52646);
#17227=VERTEX_POINT('',#52648);
#17228=VERTEX_POINT('',#52652);
#17229=VERTEX_POINT('',#52653);
#17230=VERTEX_POINT('',#52655);
#17231=VERTEX_POINT('',#52657);
#17232=VERTEX_POINT('',#52661);
#17233=VERTEX_POINT('',#52662);
#17234=VERTEX_POINT('',#52664);
#17235=VERTEX_POINT('',#52666);
#17236=VERTEX_POINT('',#52670);
#17237=VERTEX_POINT('',#52671);
#17238=VERTEX_POINT('',#52673);
#17239=VERTEX_POINT('',#52675);
#17240=VERTEX_POINT('',#52679);
#17241=VERTEX_POINT('',#52680);
#17242=VERTEX_POINT('',#52682);
#17243=VERTEX_POINT('',#52684);
#17244=VERTEX_POINT('',#52688);
#17245=VERTEX_POINT('',#52689);
#17246=VERTEX_POINT('',#52691);
#17247=VERTEX_POINT('',#52693);
#17248=VERTEX_POINT('',#52697);
#17249=VERTEX_POINT('',#52698);
#17250=VERTEX_POINT('',#52700);
#17251=VERTEX_POINT('',#52702);
#17252=VERTEX_POINT('',#52706);
#17253=VERTEX_POINT('',#52707);
#17254=VERTEX_POINT('',#52709);
#17255=VERTEX_POINT('',#52711);
#17256=VERTEX_POINT('',#52715);
#17257=VERTEX_POINT('',#52716);
#17258=VERTEX_POINT('',#52718);
#17259=VERTEX_POINT('',#52720);
#17260=VERTEX_POINT('',#52724);
#17261=VERTEX_POINT('',#52725);
#17262=VERTEX_POINT('',#52727);
#17263=VERTEX_POINT('',#52729);
#17264=VERTEX_POINT('',#52733);
#17265=VERTEX_POINT('',#52734);
#17266=VERTEX_POINT('',#52736);
#17267=VERTEX_POINT('',#52738);
#17268=VERTEX_POINT('',#52742);
#17269=VERTEX_POINT('',#52743);
#17270=VERTEX_POINT('',#52745);
#17271=VERTEX_POINT('',#52747);
#17272=VERTEX_POINT('',#52751);
#17273=VERTEX_POINT('',#52752);
#17274=VERTEX_POINT('',#52754);
#17275=VERTEX_POINT('',#52756);
#17276=VERTEX_POINT('',#52760);
#17277=VERTEX_POINT('',#52761);
#17278=VERTEX_POINT('',#52763);
#17279=VERTEX_POINT('',#52765);
#17280=VERTEX_POINT('',#52769);
#17281=VERTEX_POINT('',#52770);
#17282=VERTEX_POINT('',#52772);
#17283=VERTEX_POINT('',#52774);
#17284=VERTEX_POINT('',#52778);
#17285=VERTEX_POINT('',#52779);
#17286=VERTEX_POINT('',#52781);
#17287=VERTEX_POINT('',#52783);
#17288=VERTEX_POINT('',#52787);
#17289=VERTEX_POINT('',#52788);
#17290=VERTEX_POINT('',#52790);
#17291=VERTEX_POINT('',#52792);
#17292=VERTEX_POINT('',#52796);
#17293=VERTEX_POINT('',#52797);
#17294=VERTEX_POINT('',#52799);
#17295=VERTEX_POINT('',#52801);
#17296=VERTEX_POINT('',#52805);
#17297=VERTEX_POINT('',#52806);
#17298=VERTEX_POINT('',#52808);
#17299=VERTEX_POINT('',#52810);
#17300=VERTEX_POINT('',#52814);
#17301=VERTEX_POINT('',#52815);
#17302=VERTEX_POINT('',#52817);
#17303=VERTEX_POINT('',#52819);
#17304=VERTEX_POINT('',#52823);
#17305=VERTEX_POINT('',#52824);
#17306=VERTEX_POINT('',#52826);
#17307=VERTEX_POINT('',#52828);
#17308=VERTEX_POINT('',#52832);
#17309=VERTEX_POINT('',#52833);
#17310=VERTEX_POINT('',#52835);
#17311=VERTEX_POINT('',#52837);
#17312=VERTEX_POINT('',#52841);
#17313=VERTEX_POINT('',#52842);
#17314=VERTEX_POINT('',#52844);
#17315=VERTEX_POINT('',#52846);
#17316=VERTEX_POINT('',#52850);
#17317=VERTEX_POINT('',#52851);
#17318=VERTEX_POINT('',#52853);
#17319=VERTEX_POINT('',#52855);
#17320=VERTEX_POINT('',#52859);
#17321=VERTEX_POINT('',#52860);
#17322=VERTEX_POINT('',#52862);
#17323=VERTEX_POINT('',#52864);
#17324=VERTEX_POINT('',#52868);
#17325=VERTEX_POINT('',#52869);
#17326=VERTEX_POINT('',#52871);
#17327=VERTEX_POINT('',#52873);
#17328=VERTEX_POINT('',#52877);
#17329=VERTEX_POINT('',#52878);
#17330=VERTEX_POINT('',#52880);
#17331=VERTEX_POINT('',#52882);
#17332=VERTEX_POINT('',#52886);
#17333=VERTEX_POINT('',#52887);
#17334=VERTEX_POINT('',#52889);
#17335=VERTEX_POINT('',#52891);
#17336=VERTEX_POINT('',#52895);
#17337=VERTEX_POINT('',#52896);
#17338=VERTEX_POINT('',#52898);
#17339=VERTEX_POINT('',#52900);
#17340=VERTEX_POINT('',#52904);
#17341=VERTEX_POINT('',#52905);
#17342=VERTEX_POINT('',#52907);
#17343=VERTEX_POINT('',#52909);
#17344=VERTEX_POINT('',#52913);
#17345=VERTEX_POINT('',#52914);
#17346=VERTEX_POINT('',#52916);
#17347=VERTEX_POINT('',#52918);
#17348=VERTEX_POINT('',#52922);
#17349=VERTEX_POINT('',#52923);
#17350=VERTEX_POINT('',#52925);
#17351=VERTEX_POINT('',#52927);
#17352=VERTEX_POINT('',#52931);
#17353=VERTEX_POINT('',#52932);
#17354=VERTEX_POINT('',#52934);
#17355=VERTEX_POINT('',#52936);
#17356=VERTEX_POINT('',#52940);
#17357=VERTEX_POINT('',#52941);
#17358=VERTEX_POINT('',#52943);
#17359=VERTEX_POINT('',#52945);
#17360=VERTEX_POINT('',#52949);
#17361=VERTEX_POINT('',#52950);
#17362=VERTEX_POINT('',#52952);
#17363=VERTEX_POINT('',#52954);
#17364=VERTEX_POINT('',#52958);
#17365=VERTEX_POINT('',#52959);
#17366=VERTEX_POINT('',#52961);
#17367=VERTEX_POINT('',#52963);
#17368=VERTEX_POINT('',#52967);
#17369=VERTEX_POINT('',#52968);
#17370=VERTEX_POINT('',#52970);
#17371=VERTEX_POINT('',#52972);
#17372=VERTEX_POINT('',#52976);
#17373=VERTEX_POINT('',#52977);
#17374=VERTEX_POINT('',#52979);
#17375=VERTEX_POINT('',#52981);
#17376=VERTEX_POINT('',#52985);
#17377=VERTEX_POINT('',#52986);
#17378=VERTEX_POINT('',#52988);
#17379=VERTEX_POINT('',#52990);
#17380=VERTEX_POINT('',#52994);
#17381=VERTEX_POINT('',#52995);
#17382=VERTEX_POINT('',#52997);
#17383=VERTEX_POINT('',#52999);
#17384=VERTEX_POINT('',#53003);
#17385=VERTEX_POINT('',#53004);
#17386=VERTEX_POINT('',#53006);
#17387=VERTEX_POINT('',#53008);
#17388=VERTEX_POINT('',#53012);
#17389=VERTEX_POINT('',#53013);
#17390=VERTEX_POINT('',#53015);
#17391=VERTEX_POINT('',#53017);
#17392=VERTEX_POINT('',#53021);
#17393=VERTEX_POINT('',#53022);
#17394=VERTEX_POINT('',#53024);
#17395=VERTEX_POINT('',#53026);
#17396=VERTEX_POINT('',#53030);
#17397=VERTEX_POINT('',#53031);
#17398=VERTEX_POINT('',#53033);
#17399=VERTEX_POINT('',#53035);
#17400=VERTEX_POINT('',#53039);
#17401=VERTEX_POINT('',#53040);
#17402=VERTEX_POINT('',#53042);
#17403=VERTEX_POINT('',#53044);
#17404=VERTEX_POINT('',#53048);
#17405=VERTEX_POINT('',#53049);
#17406=VERTEX_POINT('',#53051);
#17407=VERTEX_POINT('',#53053);
#17408=VERTEX_POINT('',#53057);
#17409=VERTEX_POINT('',#53058);
#17410=VERTEX_POINT('',#53060);
#17411=VERTEX_POINT('',#53062);
#17412=VERTEX_POINT('',#53066);
#17413=VERTEX_POINT('',#53067);
#17414=VERTEX_POINT('',#53069);
#17415=VERTEX_POINT('',#53071);
#17416=VERTEX_POINT('',#53075);
#17417=VERTEX_POINT('',#53076);
#17418=VERTEX_POINT('',#53078);
#17419=VERTEX_POINT('',#53080);
#17420=VERTEX_POINT('',#53093);
#17421=VERTEX_POINT('',#53094);
#17422=VERTEX_POINT('',#53102);
#17423=VERTEX_POINT('',#53104);
#17424=VERTEX_POINT('',#53123);
#17425=VERTEX_POINT('',#53124);
#17426=VERTEX_POINT('',#53130);
#17427=VERTEX_POINT('',#53132);
#17428=VERTEX_POINT('',#53149);
#17429=VERTEX_POINT('',#53150);
#17430=VERTEX_POINT('',#53156);
#17431=VERTEX_POINT('',#53158);
#17432=VERTEX_POINT('',#53177);
#17433=VERTEX_POINT('',#53178);
#17434=VERTEX_POINT('',#53185);
#17435=VERTEX_POINT('',#53187);
#17436=VERTEX_POINT('',#53207);
#17437=VERTEX_POINT('',#53208);
#17438=VERTEX_POINT('',#53215);
#17439=VERTEX_POINT('',#53217);
#17440=VERTEX_POINT('',#53226);
#17441=VERTEX_POINT('',#53228);
#17442=VERTEX_POINT('',#53232);
#17443=VERTEX_POINT('',#53234);
#17444=VERTEX_POINT('',#53238);
#17445=VERTEX_POINT('',#53240);
#17446=VERTEX_POINT('',#53244);
#17447=VERTEX_POINT('',#53246);
#17448=VERTEX_POINT('',#53250);
#17449=VERTEX_POINT('',#53252);
#17450=VERTEX_POINT('',#53256);
#17451=VERTEX_POINT('',#53258);
#17452=VERTEX_POINT('',#53262);
#17453=VERTEX_POINT('',#53266);
#17454=VERTEX_POINT('',#53270);
#17455=VERTEX_POINT('',#53272);
#17456=VERTEX_POINT('',#53276);
#17457=VERTEX_POINT('',#53278);
#17458=VERTEX_POINT('',#53282);
#17459=VERTEX_POINT('',#53284);
#17460=VERTEX_POINT('',#53288);
#17461=VERTEX_POINT('',#53290);
#17462=VERTEX_POINT('',#53309);
#17463=VERTEX_POINT('',#53310);
#17464=VERTEX_POINT('',#53319);
#17465=VERTEX_POINT('',#53321);
#17466=VERTEX_POINT('',#53332);
#17467=VERTEX_POINT('',#53333);
#17468=VERTEX_POINT('',#53335);
#17469=VERTEX_POINT('',#53337);
#17470=VERTEX_POINT('',#53339);
#17471=VERTEX_POINT('',#53341);
#17472=VERTEX_POINT('',#53343);
#17473=VERTEX_POINT('',#53345);
#17474=VERTEX_POINT('',#53347);
#17475=VERTEX_POINT('',#53349);
#17476=VERTEX_POINT('',#53351);
#17477=VERTEX_POINT('',#53353);
#17478=VERTEX_POINT('',#53355);
#17479=VERTEX_POINT('',#53357);
#17480=VERTEX_POINT('',#53359);
#17481=VERTEX_POINT('',#53361);
#17482=VERTEX_POINT('',#53363);
#17483=VERTEX_POINT('',#53365);
#17484=VERTEX_POINT('',#53367);
#17485=VERTEX_POINT('',#53369);
#17486=VERTEX_POINT('',#53371);
#17487=VERTEX_POINT('',#53373);
#17488=VERTEX_POINT('',#53375);
#17489=VERTEX_POINT('',#53377);
#17490=VERTEX_POINT('',#53379);
#17491=VERTEX_POINT('',#53381);
#17492=VERTEX_POINT('',#53383);
#17493=VERTEX_POINT('',#53385);
#17494=VERTEX_POINT('',#53388);
#17495=VERTEX_POINT('',#53389);
#17496=VERTEX_POINT('',#53391);
#17497=VERTEX_POINT('',#53393);
#17498=VERTEX_POINT('',#53395);
#17499=VERTEX_POINT('',#53397);
#17500=VERTEX_POINT('',#53399);
#17501=VERTEX_POINT('',#53401);
#17502=VERTEX_POINT('',#53404);
#17503=VERTEX_POINT('',#53405);
#17504=VERTEX_POINT('',#53407);
#17505=VERTEX_POINT('',#53409);
#17506=VERTEX_POINT('',#53411);
#17507=VERTEX_POINT('',#53413);
#17508=VERTEX_POINT('',#53415);
#17509=VERTEX_POINT('',#53417);
#17510=VERTEX_POINT('',#53420);
#17511=VERTEX_POINT('',#53421);
#17512=VERTEX_POINT('',#53423);
#17513=VERTEX_POINT('',#53425);
#17514=VERTEX_POINT('',#53427);
#17515=VERTEX_POINT('',#53429);
#17516=VERTEX_POINT('',#53431);
#17517=VERTEX_POINT('',#53433);
#17518=VERTEX_POINT('',#53436);
#17519=VERTEX_POINT('',#53437);
#17520=VERTEX_POINT('',#53439);
#17521=VERTEX_POINT('',#53441);
#17522=VERTEX_POINT('',#53443);
#17523=VERTEX_POINT('',#53445);
#17524=VERTEX_POINT('',#53447);
#17525=VERTEX_POINT('',#53449);
#17526=VERTEX_POINT('',#53453);
#17527=VERTEX_POINT('',#53454);
#17528=VERTEX_POINT('',#53456);
#17529=VERTEX_POINT('',#53458);
#17530=VERTEX_POINT('',#53460);
#17531=VERTEX_POINT('',#53462);
#17532=VERTEX_POINT('',#53464);
#17533=VERTEX_POINT('',#53466);
#17534=VERTEX_POINT('',#53468);
#17535=VERTEX_POINT('',#53470);
#17536=VERTEX_POINT('',#53472);
#17537=VERTEX_POINT('',#53474);
#17538=VERTEX_POINT('',#53476);
#17539=VERTEX_POINT('',#53478);
#17540=VERTEX_POINT('',#53480);
#17541=VERTEX_POINT('',#53482);
#17542=VERTEX_POINT('',#53484);
#17543=VERTEX_POINT('',#53486);
#17544=VERTEX_POINT('',#53488);
#17545=VERTEX_POINT('',#53490);
#17546=VERTEX_POINT('',#53492);
#17547=VERTEX_POINT('',#53494);
#17548=VERTEX_POINT('',#53496);
#17549=VERTEX_POINT('',#53498);
#17550=VERTEX_POINT('',#53500);
#17551=VERTEX_POINT('',#53502);
#17552=VERTEX_POINT('',#53504);
#17553=VERTEX_POINT('',#53506);
#17554=VERTEX_POINT('',#53509);
#17555=VERTEX_POINT('',#53510);
#17556=VERTEX_POINT('',#53512);
#17557=VERTEX_POINT('',#53514);
#17558=VERTEX_POINT('',#53517);
#17559=VERTEX_POINT('',#53518);
#17560=VERTEX_POINT('',#53520);
#17561=VERTEX_POINT('',#53522);
#17562=VERTEX_POINT('',#53525);
#17563=VERTEX_POINT('',#53526);
#17564=VERTEX_POINT('',#53528);
#17565=VERTEX_POINT('',#53530);
#17566=VERTEX_POINT('',#53533);
#17567=VERTEX_POINT('',#53534);
#17568=VERTEX_POINT('',#53536);
#17569=VERTEX_POINT('',#53538);
#17570=VERTEX_POINT('',#53548);
#17571=VERTEX_POINT('',#53549);
#17572=VERTEX_POINT('',#53551);
#17573=VERTEX_POINT('',#53553);
#17574=VERTEX_POINT('',#53555);
#17575=VERTEX_POINT('',#53557);
#17576=VERTEX_POINT('',#53560);
#17577=VERTEX_POINT('',#53561);
#17578=VERTEX_POINT('',#53563);
#17579=VERTEX_POINT('',#53565);
#17580=VERTEX_POINT('',#53567);
#17581=VERTEX_POINT('',#53569);
#17582=VERTEX_POINT('',#53571);
#17583=VERTEX_POINT('',#53573);
#17584=VERTEX_POINT('',#53576);
#17585=VERTEX_POINT('',#53577);
#17586=VERTEX_POINT('',#53579);
#17587=VERTEX_POINT('',#53581);
#17588=VERTEX_POINT('',#53583);
#17589=VERTEX_POINT('',#53585);
#17590=VERTEX_POINT('',#53587);
#17591=VERTEX_POINT('',#53589);
#17592=VERTEX_POINT('',#53593);
#17593=VERTEX_POINT('',#53594);
#17594=VERTEX_POINT('',#53596);
#17595=VERTEX_POINT('',#53598);
#17596=VERTEX_POINT('',#53600);
#17597=VERTEX_POINT('',#53602);
#17598=VERTEX_POINT('',#53605);
#17599=VERTEX_POINT('',#53606);
#17600=VERTEX_POINT('',#53608);
#17601=VERTEX_POINT('',#53610);
#17602=VERTEX_POINT('',#53613);
#17603=VERTEX_POINT('',#53614);
#17604=VERTEX_POINT('',#53616);
#17605=VERTEX_POINT('',#53618);
#17606=VERTEX_POINT('',#53628);
#17607=VERTEX_POINT('',#53629);
#17608=VERTEX_POINT('',#53631);
#17609=VERTEX_POINT('',#53633);
#17610=VERTEX_POINT('',#53635);
#17611=VERTEX_POINT('',#53637);
#17612=VERTEX_POINT('',#53639);
#17613=VERTEX_POINT('',#53641);
#17614=VERTEX_POINT('',#53643);
#17615=VERTEX_POINT('',#53645);
#17616=VERTEX_POINT('',#53648);
#17617=VERTEX_POINT('',#53650);
#17618=VERTEX_POINT('',#53653);
#17619=VERTEX_POINT('',#53655);
#17620=VERTEX_POINT('',#53658);
#17621=VERTEX_POINT('',#53660);
#17622=VERTEX_POINT('',#53663);
#17623=VERTEX_POINT('',#53665);
#17624=VERTEX_POINT('',#53668);
#17625=VERTEX_POINT('',#53670);
#17626=VERTEX_POINT('',#53673);
#17627=VERTEX_POINT('',#53675);
#17628=VERTEX_POINT('',#53678);
#17629=VERTEX_POINT('',#53680);
#17630=VERTEX_POINT('',#53683);
#17631=VERTEX_POINT('',#53685);
#17632=VERTEX_POINT('',#53688);
#17633=VERTEX_POINT('',#53690);
#17634=VERTEX_POINT('',#53693);
#17635=VERTEX_POINT('',#53695);
#17636=VERTEX_POINT('',#53698);
#17637=VERTEX_POINT('',#53700);
#17638=VERTEX_POINT('',#53703);
#17639=VERTEX_POINT('',#53705);
#17640=VERTEX_POINT('',#53708);
#17641=VERTEX_POINT('',#53710);
#17642=VERTEX_POINT('',#53713);
#17643=VERTEX_POINT('',#53715);
#17644=VERTEX_POINT('',#53718);
#17645=VERTEX_POINT('',#53720);
#17646=VERTEX_POINT('',#53723);
#17647=VERTEX_POINT('',#53725);
#17648=VERTEX_POINT('',#53728);
#17649=VERTEX_POINT('',#53730);
#17650=VERTEX_POINT('',#53733);
#17651=VERTEX_POINT('',#53735);
#17652=VERTEX_POINT('',#53738);
#17653=VERTEX_POINT('',#53740);
#17654=VERTEX_POINT('',#53743);
#17655=VERTEX_POINT('',#53745);
#17656=VERTEX_POINT('',#53748);
#17657=VERTEX_POINT('',#53750);
#17658=VERTEX_POINT('',#53753);
#17659=VERTEX_POINT('',#53755);
#17660=VERTEX_POINT('',#53758);
#17661=VERTEX_POINT('',#53760);
#17662=VERTEX_POINT('',#53763);
#17663=VERTEX_POINT('',#53765);
#17664=VERTEX_POINT('',#53768);
#17665=VERTEX_POINT('',#53770);
#17666=VERTEX_POINT('',#53773);
#17667=VERTEX_POINT('',#53775);
#17668=VERTEX_POINT('',#53778);
#17669=VERTEX_POINT('',#53780);
#17670=VERTEX_POINT('',#53783);
#17671=VERTEX_POINT('',#53785);
#17672=VERTEX_POINT('',#53788);
#17673=VERTEX_POINT('',#53790);
#17674=VERTEX_POINT('',#53793);
#17675=VERTEX_POINT('',#53795);
#17676=VERTEX_POINT('',#53798);
#17677=VERTEX_POINT('',#53800);
#17678=VERTEX_POINT('',#53803);
#17679=VERTEX_POINT('',#53805);
#17680=VERTEX_POINT('',#53808);
#17681=VERTEX_POINT('',#53810);
#17682=VERTEX_POINT('',#53813);
#17683=VERTEX_POINT('',#53815);
#17684=VERTEX_POINT('',#53818);
#17685=VERTEX_POINT('',#53820);
#17686=VERTEX_POINT('',#53823);
#17687=VERTEX_POINT('',#53825);
#17688=VERTEX_POINT('',#53828);
#17689=VERTEX_POINT('',#53830);
#17690=VERTEX_POINT('',#53833);
#17691=VERTEX_POINT('',#53835);
#17692=VERTEX_POINT('',#53838);
#17693=VERTEX_POINT('',#53840);
#17694=VERTEX_POINT('',#53843);
#17695=VERTEX_POINT('',#53845);
#17696=VERTEX_POINT('',#53848);
#17697=VERTEX_POINT('',#53850);
#17698=VERTEX_POINT('',#53853);
#17699=VERTEX_POINT('',#53855);
#17700=VERTEX_POINT('',#53858);
#17701=VERTEX_POINT('',#53860);
#17702=VERTEX_POINT('',#53863);
#17703=VERTEX_POINT('',#53865);
#17704=VERTEX_POINT('',#53868);
#17705=VERTEX_POINT('',#53870);
#17706=VERTEX_POINT('',#53873);
#17707=VERTEX_POINT('',#53875);
#17708=VERTEX_POINT('',#53878);
#17709=VERTEX_POINT('',#53880);
#17710=VERTEX_POINT('',#53883);
#17711=VERTEX_POINT('',#53885);
#17712=VERTEX_POINT('',#53889);
#17713=VERTEX_POINT('',#53890);
#17714=VERTEX_POINT('',#53892);
#17715=VERTEX_POINT('',#53894);
#17716=VERTEX_POINT('',#53896);
#17717=VERTEX_POINT('',#53898);
#17718=VERTEX_POINT('',#53900);
#17719=VERTEX_POINT('',#53902);
#17720=VERTEX_POINT('',#53904);
#17721=VERTEX_POINT('',#53906);
#17722=VERTEX_POINT('',#53909);
#17723=VERTEX_POINT('',#53911);
#17724=VERTEX_POINT('',#53914);
#17725=VERTEX_POINT('',#53916);
#17726=VERTEX_POINT('',#53919);
#17727=VERTEX_POINT('',#53921);
#17728=VERTEX_POINT('',#53924);
#17729=VERTEX_POINT('',#53926);
#17730=VERTEX_POINT('',#53929);
#17731=VERTEX_POINT('',#53931);
#17732=VERTEX_POINT('',#53934);
#17733=VERTEX_POINT('',#53936);
#17734=VERTEX_POINT('',#53939);
#17735=VERTEX_POINT('',#53941);
#17736=VERTEX_POINT('',#53944);
#17737=VERTEX_POINT('',#53946);
#17738=VERTEX_POINT('',#53949);
#17739=VERTEX_POINT('',#53951);
#17740=VERTEX_POINT('',#53954);
#17741=VERTEX_POINT('',#53956);
#17742=VERTEX_POINT('',#53959);
#17743=VERTEX_POINT('',#53961);
#17744=VERTEX_POINT('',#53964);
#17745=VERTEX_POINT('',#53966);
#17746=VERTEX_POINT('',#53969);
#17747=VERTEX_POINT('',#53971);
#17748=VERTEX_POINT('',#53974);
#17749=VERTEX_POINT('',#53976);
#17750=VERTEX_POINT('',#53979);
#17751=VERTEX_POINT('',#53981);
#17752=VERTEX_POINT('',#53984);
#17753=VERTEX_POINT('',#53986);
#17754=VERTEX_POINT('',#53989);
#17755=VERTEX_POINT('',#53991);
#17756=VERTEX_POINT('',#53994);
#17757=VERTEX_POINT('',#53996);
#17758=VERTEX_POINT('',#53999);
#17759=VERTEX_POINT('',#54001);
#17760=VERTEX_POINT('',#54004);
#17761=VERTEX_POINT('',#54006);
#17762=VERTEX_POINT('',#54009);
#17763=VERTEX_POINT('',#54011);
#17764=VERTEX_POINT('',#54014);
#17765=VERTEX_POINT('',#54016);
#17766=VERTEX_POINT('',#54019);
#17767=VERTEX_POINT('',#54021);
#17768=VERTEX_POINT('',#54024);
#17769=VERTEX_POINT('',#54026);
#17770=VERTEX_POINT('',#54029);
#17771=VERTEX_POINT('',#54031);
#17772=VERTEX_POINT('',#54034);
#17773=VERTEX_POINT('',#54036);
#17774=VERTEX_POINT('',#54039);
#17775=VERTEX_POINT('',#54041);
#17776=VERTEX_POINT('',#54044);
#17777=VERTEX_POINT('',#54046);
#17778=VERTEX_POINT('',#54049);
#17779=VERTEX_POINT('',#54051);
#17780=VERTEX_POINT('',#54054);
#17781=VERTEX_POINT('',#54056);
#17782=VERTEX_POINT('',#54059);
#17783=VERTEX_POINT('',#54061);
#17784=VERTEX_POINT('',#54064);
#17785=VERTEX_POINT('',#54066);
#17786=VERTEX_POINT('',#54069);
#17787=VERTEX_POINT('',#54071);
#17788=VERTEX_POINT('',#54074);
#17789=VERTEX_POINT('',#54076);
#17790=VERTEX_POINT('',#54079);
#17791=VERTEX_POINT('',#54081);
#17792=VERTEX_POINT('',#54084);
#17793=VERTEX_POINT('',#54086);
#17794=VERTEX_POINT('',#54089);
#17795=VERTEX_POINT('',#54091);
#17796=VERTEX_POINT('',#54094);
#17797=VERTEX_POINT('',#54096);
#17798=VERTEX_POINT('',#54099);
#17799=VERTEX_POINT('',#54101);
#17800=VERTEX_POINT('',#54104);
#17801=VERTEX_POINT('',#54106);
#17802=VERTEX_POINT('',#54109);
#17803=VERTEX_POINT('',#54111);
#17804=VERTEX_POINT('',#54114);
#17805=VERTEX_POINT('',#54116);
#17806=VERTEX_POINT('',#54119);
#17807=VERTEX_POINT('',#54121);
#17808=VERTEX_POINT('',#54124);
#17809=VERTEX_POINT('',#54126);
#17810=VERTEX_POINT('',#54129);
#17811=VERTEX_POINT('',#54131);
#17812=VERTEX_POINT('',#54134);
#17813=VERTEX_POINT('',#54136);
#17814=VERTEX_POINT('',#54139);
#17815=VERTEX_POINT('',#54141);
#17816=VERTEX_POINT('',#54144);
#17817=VERTEX_POINT('',#54146);
#17818=VERTEX_POINT('',#54150);
#17819=VERTEX_POINT('',#54152);
#17820=VERTEX_POINT('',#54156);
#17821=VERTEX_POINT('',#54158);
#17822=VERTEX_POINT('',#54162);
#17823=VERTEX_POINT('',#54163);
#17824=VERTEX_POINT('',#54165);
#17825=VERTEX_POINT('',#54167);
#17826=VERTEX_POINT('',#54171);
#17827=VERTEX_POINT('',#54173);
#17828=VERTEX_POINT('',#54177);
#17829=VERTEX_POINT('',#54178);
#17830=VERTEX_POINT('',#54180);
#17831=VERTEX_POINT('',#54182);
#17832=VERTEX_POINT('',#54186);
#17833=VERTEX_POINT('',#54188);
#17834=VERTEX_POINT('',#54192);
#17835=VERTEX_POINT('',#54194);
#17836=VERTEX_POINT('',#54198);
#17837=VERTEX_POINT('',#54199);
#17838=VERTEX_POINT('',#54201);
#17839=VERTEX_POINT('',#54203);
#17840=VERTEX_POINT('',#54207);
#17841=VERTEX_POINT('',#54208);
#17842=VERTEX_POINT('',#54210);
#17843=VERTEX_POINT('',#54212);
#17844=VERTEX_POINT('',#54216);
#17845=VERTEX_POINT('',#54218);
#17846=VERTEX_POINT('',#54222);
#17847=VERTEX_POINT('',#54223);
#17848=VERTEX_POINT('',#54225);
#17849=VERTEX_POINT('',#54227);
#17850=VERTEX_POINT('',#54231);
#17851=VERTEX_POINT('',#54232);
#17852=VERTEX_POINT('',#54234);
#17853=VERTEX_POINT('',#54236);
#17854=VERTEX_POINT('',#54240);
#17855=VERTEX_POINT('',#54242);
#17856=VERTEX_POINT('',#54246);
#17857=VERTEX_POINT('',#54248);
#17858=VERTEX_POINT('',#54252);
#17859=VERTEX_POINT('',#54253);
#17860=VERTEX_POINT('',#54255);
#17861=VERTEX_POINT('',#54257);
#17862=VERTEX_POINT('',#54261);
#17863=VERTEX_POINT('',#54263);
#17864=VERTEX_POINT('',#54267);
#17865=VERTEX_POINT('',#54268);
#17866=VERTEX_POINT('',#54270);
#17867=VERTEX_POINT('',#54272);
#17868=VERTEX_POINT('',#54276);
#17869=VERTEX_POINT('',#54278);
#17870=VERTEX_POINT('',#54282);
#17871=VERTEX_POINT('',#54284);
#17872=VERTEX_POINT('',#54288);
#17873=VERTEX_POINT('',#54289);
#17874=VERTEX_POINT('',#54291);
#17875=VERTEX_POINT('',#54293);
#17876=VERTEX_POINT('',#54297);
#17877=VERTEX_POINT('',#54298);
#17878=VERTEX_POINT('',#54300);
#17879=VERTEX_POINT('',#54302);
#17880=VERTEX_POINT('',#54306);
#17881=VERTEX_POINT('',#54308);
#17882=VERTEX_POINT('',#54312);
#17883=VERTEX_POINT('',#54313);
#17884=VERTEX_POINT('',#54315);
#17885=VERTEX_POINT('',#54317);
#17886=VERTEX_POINT('',#54321);
#17887=VERTEX_POINT('',#54322);
#17888=VERTEX_POINT('',#54324);
#17889=VERTEX_POINT('',#54326);
#17890=VERTEX_POINT('',#54355);
#17891=VERTEX_POINT('',#54356);
#17892=VERTEX_POINT('',#54370);
#17893=VERTEX_POINT('',#54372);
#17894=VERTEX_POINT('',#54389);
#17895=VERTEX_POINT('',#54403);
#17896=VERTEX_POINT('',#54405);
#17897=VERTEX_POINT('',#54407);
#17898=VERTEX_POINT('',#54416);
#17899=VERTEX_POINT('',#54424);
#17900=VERTEX_POINT('',#54425);
#17901=VERTEX_POINT('',#54427);
#17902=VERTEX_POINT('',#54435);
#17903=VERTEX_POINT('',#54437);
#17904=VERTEX_POINT('',#54439);
#17905=VERTEX_POINT('',#54449);
#17906=VERTEX_POINT('',#54451);
#17907=VERTEX_POINT('',#54458);
#17908=VERTEX_POINT('',#54460);
#17909=VERTEX_POINT('',#54462);
#17910=VERTEX_POINT('',#54464);
#17911=VERTEX_POINT('',#54474);
#17912=VERTEX_POINT('',#54476);
#17913=VERTEX_POINT('',#54478);
#17914=VERTEX_POINT('',#54486);
#17915=VERTEX_POINT('',#54488);
#17916=VERTEX_POINT('',#54490);
#17917=VERTEX_POINT('',#54499);
#17918=VERTEX_POINT('',#54501);
#17919=VERTEX_POINT('',#54503);
#17920=VERTEX_POINT('',#54510);
#17921=VERTEX_POINT('',#54512);
#17922=VERTEX_POINT('',#54514);
#17923=VERTEX_POINT('',#54524);
#17924=VERTEX_POINT('',#54525);
#17925=VERTEX_POINT('',#54527);
#17926=VERTEX_POINT('',#54529);
#17927=VERTEX_POINT('',#54536);
#17928=VERTEX_POINT('',#54539);
#17929=VERTEX_POINT('',#54549);
#17930=VERTEX_POINT('',#54559);
#17931=VERTEX_POINT('',#54561);
#17932=VERTEX_POINT('',#54571);
#17933=VERTEX_POINT('',#54581);
#17934=VERTEX_POINT('',#54583);
#17935=VERTEX_POINT('',#54593);
#17936=VERTEX_POINT('',#54595);
#17937=VERTEX_POINT('',#54604);
#17938=VERTEX_POINT('',#54615);
#17939=VERTEX_POINT('',#54617);
#17940=VERTEX_POINT('',#54627);
#17941=VERTEX_POINT('',#54637);
#17942=VERTEX_POINT('',#54639);
#17943=VERTEX_POINT('',#54649);
#17944=VERTEX_POINT('',#54659);
#17945=VERTEX_POINT('',#54671);
#17946=VERTEX_POINT('',#54681);
#17947=VERTEX_POINT('',#54683);
#17948=VERTEX_POINT('',#54698);
#17949=VERTEX_POINT('',#54700);
#17950=VERTEX_POINT('',#54711);
#17951=VERTEX_POINT('',#54726);
#17952=VERTEX_POINT('',#54728);
#17953=VERTEX_POINT('',#54738);
#17954=VERTEX_POINT('',#54753);
#17955=VERTEX_POINT('',#54755);
#17956=VERTEX_POINT('',#54765);
#17957=VERTEX_POINT('',#54781);
#17958=VERTEX_POINT('',#54823);
#17959=VERTEX_POINT('',#54852);
#17960=VERTEX_POINT('',#54893);
#17961=VERTEX_POINT('',#54934);
#17962=VERTEX_POINT('',#54950);
#17963=VERTEX_POINT('',#54951);
#17964=VERTEX_POINT('',#54953);
#17965=VERTEX_POINT('',#54955);
#17966=VERTEX_POINT('',#54957);
#17967=VERTEX_POINT('',#54959);
#17968=VERTEX_POINT('',#54961);
#17969=VERTEX_POINT('',#54963);
#17970=VERTEX_POINT('',#54965);
#17971=VERTEX_POINT('',#54967);
#17972=VERTEX_POINT('',#54970);
#17973=VERTEX_POINT('',#54971);
#17974=VERTEX_POINT('',#54973);
#17975=VERTEX_POINT('',#54975);
#17976=VERTEX_POINT('',#54978);
#17977=VERTEX_POINT('',#54979);
#17978=VERTEX_POINT('',#54981);
#17979=VERTEX_POINT('',#54983);
#17980=VERTEX_POINT('',#54985);
#17981=VERTEX_POINT('',#54987);
#17982=VERTEX_POINT('',#54989);
#17983=VERTEX_POINT('',#54991);
#17984=VERTEX_POINT('',#54993);
#17985=VERTEX_POINT('',#54995);
#17986=VERTEX_POINT('',#54997);
#17987=VERTEX_POINT('',#54999);
#17988=VERTEX_POINT('',#55003);
#17989=VERTEX_POINT('',#55004);
#17990=VERTEX_POINT('',#55006);
#17991=VERTEX_POINT('',#55008);
#17992=VERTEX_POINT('',#55010);
#17993=VERTEX_POINT('',#55012);
#17994=VERTEX_POINT('',#55014);
#17995=VERTEX_POINT('',#55016);
#17996=VERTEX_POINT('',#55018);
#17997=VERTEX_POINT('',#55020);
#17998=VERTEX_POINT('',#55023);
#17999=VERTEX_POINT('',#55024);
#18000=VERTEX_POINT('',#55026);
#18001=VERTEX_POINT('',#55028);
#18002=VERTEX_POINT('',#55031);
#18003=VERTEX_POINT('',#55032);
#18004=VERTEX_POINT('',#55034);
#18005=VERTEX_POINT('',#55036);
#18006=VERTEX_POINT('',#55038);
#18007=VERTEX_POINT('',#55040);
#18008=VERTEX_POINT('',#55042);
#18009=VERTEX_POINT('',#55044);
#18010=VERTEX_POINT('',#55046);
#18011=VERTEX_POINT('',#55048);
#18012=VERTEX_POINT('',#55050);
#18013=VERTEX_POINT('',#55052);
#18014=VERTEX_POINT('',#55056);
#18015=VERTEX_POINT('',#55062);
#18016=VERTEX_POINT('',#55068);
#18017=VERTEX_POINT('',#55074);
#18018=VERTEX_POINT('',#55139);
#18019=VERTEX_POINT('',#55225);
#18020=VERTEX_POINT('',#55348);
#18021=VERTEX_POINT('',#55474);
#18022=VERTEX_POINT('',#55544);
#18023=VERTEX_POINT('',#55546);
#18024=VERTEX_POINT('',#55550);
#18025=VERTEX_POINT('',#55552);
#18026=VERTEX_POINT('',#55556);
#18027=VERTEX_POINT('',#55558);
#18028=VERTEX_POINT('',#55560);
#18029=VERTEX_POINT('',#55562);
#18030=VERTEX_POINT('',#55564);
#18031=VERTEX_POINT('',#55567);
#18032=VERTEX_POINT('',#55569);
#18033=VERTEX_POINT('',#55571);
#18034=VERTEX_POINT('',#55573);
#18035=VERTEX_POINT('',#55575);
#18036=VERTEX_POINT('',#55579);
#18037=VERTEX_POINT('',#55581);
#18038=VERTEX_POINT('',#55583);
#18039=VERTEX_POINT('',#55585);
#18040=VERTEX_POINT('',#55587);
#18041=VERTEX_POINT('',#55590);
#18042=VERTEX_POINT('',#55592);
#18043=VERTEX_POINT('',#55594);
#18044=VERTEX_POINT('',#55596);
#18045=VERTEX_POINT('',#55598);
#18046=VERTEX_POINT('',#55630);
#18047=VERTEX_POINT('',#55632);
#18048=VERTEX_POINT('',#55636);
#18049=VERTEX_POINT('',#55638);
#18050=VERTEX_POINT('',#55642);
#18051=VERTEX_POINT('',#55644);
#18052=VERTEX_POINT('',#55646);
#18053=VERTEX_POINT('',#55648);
#18054=VERTEX_POINT('',#55650);
#18055=VERTEX_POINT('',#55653);
#18056=VERTEX_POINT('',#55655);
#18057=VERTEX_POINT('',#55657);
#18058=VERTEX_POINT('',#55659);
#18059=VERTEX_POINT('',#55661);
#18060=VERTEX_POINT('',#55665);
#18061=VERTEX_POINT('',#55667);
#18062=VERTEX_POINT('',#55669);
#18063=VERTEX_POINT('',#55671);
#18064=VERTEX_POINT('',#55673);
#18065=VERTEX_POINT('',#55676);
#18066=VERTEX_POINT('',#55678);
#18067=VERTEX_POINT('',#55680);
#18068=VERTEX_POINT('',#55682);
#18069=VERTEX_POINT('',#55684);
#18070=VERTEX_POINT('',#55716);
#18071=VERTEX_POINT('',#55718);
#18072=VERTEX_POINT('',#55722);
#18073=VERTEX_POINT('',#55724);
#18074=VERTEX_POINT('',#55728);
#18075=VERTEX_POINT('',#55730);
#18076=VERTEX_POINT('',#55732);
#18077=VERTEX_POINT('',#55734);
#18078=VERTEX_POINT('',#55736);
#18079=VERTEX_POINT('',#55739);
#18080=VERTEX_POINT('',#55741);
#18081=VERTEX_POINT('',#55743);
#18082=VERTEX_POINT('',#55745);
#18083=VERTEX_POINT('',#55747);
#18084=VERTEX_POINT('',#55751);
#18085=VERTEX_POINT('',#55753);
#18086=VERTEX_POINT('',#55755);
#18087=VERTEX_POINT('',#55757);
#18088=VERTEX_POINT('',#55759);
#18089=VERTEX_POINT('',#55762);
#18090=VERTEX_POINT('',#55764);
#18091=VERTEX_POINT('',#55766);
#18092=VERTEX_POINT('',#55768);
#18093=VERTEX_POINT('',#55770);
#18094=VERTEX_POINT('',#55802);
#18095=VERTEX_POINT('',#55804);
#18096=VERTEX_POINT('',#55808);
#18097=VERTEX_POINT('',#55810);
#18098=VERTEX_POINT('',#55814);
#18099=VERTEX_POINT('',#55816);
#18100=VERTEX_POINT('',#55818);
#18101=VERTEX_POINT('',#55820);
#18102=VERTEX_POINT('',#55822);
#18103=VERTEX_POINT('',#55825);
#18104=VERTEX_POINT('',#55827);
#18105=VERTEX_POINT('',#55829);
#18106=VERTEX_POINT('',#55831);
#18107=VERTEX_POINT('',#55833);
#18108=VERTEX_POINT('',#55837);
#18109=VERTEX_POINT('',#55839);
#18110=VERTEX_POINT('',#55841);
#18111=VERTEX_POINT('',#55843);
#18112=VERTEX_POINT('',#55845);
#18113=VERTEX_POINT('',#55848);
#18114=VERTEX_POINT('',#55850);
#18115=VERTEX_POINT('',#55852);
#18116=VERTEX_POINT('',#55854);
#18117=VERTEX_POINT('',#55856);
#18118=VERTEX_POINT('',#55888);
#18119=VERTEX_POINT('',#55896);
#18120=VERTEX_POINT('',#55898);
#18121=VERTEX_POINT('',#55901);
#18122=VERTEX_POINT('',#55902);
#18123=VERTEX_POINT('',#55911);
#18124=VERTEX_POINT('',#55914);
#18125=VERTEX_POINT('',#55921);
#18126=VERTEX_POINT('',#55923);
#18127=VERTEX_POINT('',#55926);
#18128=VERTEX_POINT('',#55927);
#18129=VERTEX_POINT('',#55936);
#18130=VERTEX_POINT('',#55938);
#18131=VERTEX_POINT('',#55940);
#18132=VERTEX_POINT('',#55948);
#18133=VERTEX_POINT('',#55951);
#18134=VERTEX_POINT('',#55959);
#18135=VERTEX_POINT('',#55961);
#18136=VERTEX_POINT('',#55963);
#18137=VERTEX_POINT('',#55965);
#18138=VERTEX_POINT('',#55973);
#18139=VERTEX_POINT('',#55976);
#18140=VERTEX_POINT('',#55985);
#18141=VERTEX_POINT('',#55987);
#18142=VERTEX_POINT('',#55989);
#18143=VERTEX_POINT('',#55991);
#18144=VERTEX_POINT('',#55998);
#18145=VERTEX_POINT('',#56001);
#18146=VERTEX_POINT('',#56010);
#18147=VERTEX_POINT('',#56012);
#18148=VERTEX_POINT('',#56014);
#18149=VERTEX_POINT('',#56021);
#18150=VERTEX_POINT('',#56023);
#18151=VERTEX_POINT('',#56033);
#18152=VERTEX_POINT('',#56041);
#18153=VERTEX_POINT('',#56042);
#18154=VERTEX_POINT('',#56052);
#18155=VERTEX_POINT('',#56063);
#18156=VERTEX_POINT('',#56064);
#18157=VERTEX_POINT('',#56074);
#18158=VERTEX_POINT('',#56085);
#18159=VERTEX_POINT('',#56096);
#18160=VERTEX_POINT('',#56098);
#18161=VERTEX_POINT('',#56107);
#18162=VERTEX_POINT('',#56117);
#18163=VERTEX_POINT('',#56119);
#18164=VERTEX_POINT('',#56129);
#18165=VERTEX_POINT('',#56138);
#18166=VERTEX_POINT('',#56140);
#18167=VERTEX_POINT('',#56152);
#18168=VERTEX_POINT('',#56162);
#18169=VERTEX_POINT('',#56173);
#18170=VERTEX_POINT('',#56174);
#18171=VERTEX_POINT('',#56189);
#18172=VERTEX_POINT('',#56201);
#18173=VERTEX_POINT('',#56203);
#18174=VERTEX_POINT('',#56215);
#18175=VERTEX_POINT('',#56217);
#18176=VERTEX_POINT('',#56227);
#18177=VERTEX_POINT('',#56229);
#18178=VERTEX_POINT('',#57141);
#18179=VERTEX_POINT('',#57143);
#18180=VERTEX_POINT('',#57147);
#18181=VERTEX_POINT('',#57149);
#18182=VERTEX_POINT('',#57153);
#18183=VERTEX_POINT('',#57155);
#18184=VERTEX_POINT('',#57157);
#18185=VERTEX_POINT('',#57159);
#18186=VERTEX_POINT('',#57161);
#18187=VERTEX_POINT('',#57163);
#18188=VERTEX_POINT('',#57166);
#18189=VERTEX_POINT('',#57168);
#18190=VERTEX_POINT('',#57170);
#18191=VERTEX_POINT('',#57172);
#18192=VERTEX_POINT('',#57176);
#18193=VERTEX_POINT('',#57178);
#18194=VERTEX_POINT('',#57180);
#18195=VERTEX_POINT('',#57182);
#18196=VERTEX_POINT('',#57184);
#18197=VERTEX_POINT('',#57186);
#18198=VERTEX_POINT('',#57189);
#18199=VERTEX_POINT('',#57191);
#18200=VERTEX_POINT('',#57193);
#18201=VERTEX_POINT('',#57195);
#18202=VERTEX_POINT('',#57227);
#18203=VERTEX_POINT('',#57229);
#18204=VERTEX_POINT('',#57233);
#18205=VERTEX_POINT('',#57235);
#18206=VERTEX_POINT('',#57239);
#18207=VERTEX_POINT('',#57241);
#18208=VERTEX_POINT('',#57243);
#18209=VERTEX_POINT('',#57245);
#18210=VERTEX_POINT('',#57247);
#18211=VERTEX_POINT('',#57249);
#18212=VERTEX_POINT('',#57252);
#18213=VERTEX_POINT('',#57254);
#18214=VERTEX_POINT('',#57256);
#18215=VERTEX_POINT('',#57258);
#18216=VERTEX_POINT('',#57262);
#18217=VERTEX_POINT('',#57264);
#18218=VERTEX_POINT('',#57266);
#18219=VERTEX_POINT('',#57268);
#18220=VERTEX_POINT('',#57270);
#18221=VERTEX_POINT('',#57272);
#18222=VERTEX_POINT('',#57275);
#18223=VERTEX_POINT('',#57277);
#18224=VERTEX_POINT('',#57279);
#18225=VERTEX_POINT('',#57281);
#18226=VERTEX_POINT('',#57319);
#18227=VERTEX_POINT('',#57320);
#18228=VERTEX_POINT('',#57325);
#18229=VERTEX_POINT('',#57327);
#18230=VERTEX_POINT('',#57335);
#18231=VERTEX_POINT('',#57337);
#18232=VERTEX_POINT('',#57341);
#18233=VERTEX_POINT('',#57343);
#18234=VERTEX_POINT('',#57347);
#18235=VERTEX_POINT('',#57349);
#18236=VERTEX_POINT('',#57353);
#18237=VERTEX_POINT('',#57355);
#18238=VERTEX_POINT('',#57365);
#18239=VERTEX_POINT('',#57367);
#18240=VERTEX_POINT('',#57371);
#18241=VERTEX_POINT('',#57373);
#18242=VERTEX_POINT('',#57377);
#18243=VERTEX_POINT('',#57379);
#18244=VERTEX_POINT('',#57383);
#18245=VERTEX_POINT('',#57384);
#18246=VERTEX_POINT('',#57387);
#18247=VERTEX_POINT('',#57391);
#18248=VERTEX_POINT('',#57392);
#18249=VERTEX_POINT('',#57395);
#18250=VERTEX_POINT('',#57399);
#18251=VERTEX_POINT('',#57403);
#18252=VERTEX_POINT('',#57404);
#18253=VERTEX_POINT('',#57406);
#18254=VERTEX_POINT('',#57408);
#18255=VERTEX_POINT('',#57412);
#18256=VERTEX_POINT('',#57416);
#18257=VERTEX_POINT('',#57417);
#18258=VERTEX_POINT('',#57419);
#18259=VERTEX_POINT('',#57421);
#18260=VERTEX_POINT('',#57423);
#18261=VERTEX_POINT('',#57425);
#18262=VERTEX_POINT('',#57427);
#18263=VERTEX_POINT('',#57429);
#18264=VERTEX_POINT('',#57431);
#18265=VERTEX_POINT('',#57433);
#18266=VERTEX_POINT('',#57435);
#18267=VERTEX_POINT('',#57437);
#18268=VERTEX_POINT('',#57440);
#18269=VERTEX_POINT('',#57441);
#18270=VERTEX_POINT('',#57443);
#18271=VERTEX_POINT('',#57445);
#18272=VERTEX_POINT('',#57448);
#18273=VERTEX_POINT('',#57449);
#18274=VERTEX_POINT('',#57451);
#18275=VERTEX_POINT('',#57453);
#18276=VERTEX_POINT('',#57456);
#18277=VERTEX_POINT('',#57457);
#18278=VERTEX_POINT('',#57459);
#18279=VERTEX_POINT('',#57461);
#18280=VERTEX_POINT('',#57465);
#18281=VERTEX_POINT('',#57466);
#18282=VERTEX_POINT('',#57468);
#18283=VERTEX_POINT('',#57470);
#18284=VERTEX_POINT('',#57474);
#18285=VERTEX_POINT('',#57475);
#18286=VERTEX_POINT('',#57477);
#18287=VERTEX_POINT('',#57480);
#18288=VERTEX_POINT('',#57484);
#18289=VERTEX_POINT('',#57485);
#18290=VERTEX_POINT('',#57487);
#18291=VERTEX_POINT('',#57490);
#18292=VERTEX_POINT('',#57497);
#18293=VERTEX_POINT('',#57498);
#18294=VERTEX_POINT('',#57500);
#18295=VERTEX_POINT('',#57502);
#18296=VERTEX_POINT('',#57504);
#18297=VERTEX_POINT('',#57506);
#18298=VERTEX_POINT('',#57510);
#18299=VERTEX_POINT('',#57511);
#18300=VERTEX_POINT('',#57516);
#18301=VERTEX_POINT('',#57518);
#18302=VERTEX_POINT('',#57520);
#18303=VERTEX_POINT('',#57522);
#18304=VERTEX_POINT('',#57529);
#18305=VERTEX_POINT('',#57530);
#18306=VERTEX_POINT('',#57532);
#18307=VERTEX_POINT('',#57534);
#18308=VERTEX_POINT('',#57538);
#18309=VERTEX_POINT('',#57539);
#18310=VERTEX_POINT('',#57542);
#18311=VERTEX_POINT('',#57544);
#18312=VERTEX_POINT('',#57548);
#18313=VERTEX_POINT('',#57550);
#18314=VERTEX_POINT('',#57552);
#18315=VERTEX_POINT('',#57554);
#18316=VERTEX_POINT('',#57561);
#18317=VERTEX_POINT('',#57562);
#18318=VERTEX_POINT('',#57564);
#18319=VERTEX_POINT('',#57566);
#18320=VERTEX_POINT('',#57568);
#18321=VERTEX_POINT('',#57570);
#18322=VERTEX_POINT('',#57572);
#18323=VERTEX_POINT('',#57574);
#18324=VERTEX_POINT('',#57576);
#18325=VERTEX_POINT('',#57578);
#18326=VERTEX_POINT('',#57580);
#18327=VERTEX_POINT('',#57582);
#18328=VERTEX_POINT('',#57589);
#18329=VERTEX_POINT('',#57590);
#18330=VERTEX_POINT('',#57592);
#18331=VERTEX_POINT('',#57594);
#18332=VERTEX_POINT('',#57596);
#18333=VERTEX_POINT('',#57598);
#18334=VERTEX_POINT('',#57600);
#18335=VERTEX_POINT('',#57602);
#18336=VERTEX_POINT('',#57605);
#18337=VERTEX_POINT('',#57606);
#18338=VERTEX_POINT('',#57608);
#18339=VERTEX_POINT('',#57610);
#18340=VERTEX_POINT('',#57612);
#18341=VERTEX_POINT('',#57614);
#18342=VERTEX_POINT('',#57616);
#18343=VERTEX_POINT('',#57618);
#18344=VERTEX_POINT('',#57620);
#18345=VERTEX_POINT('',#57622);
#18346=VERTEX_POINT('',#57624);
#18347=VERTEX_POINT('',#57626);
#18348=VERTEX_POINT('',#57630);
#18349=VERTEX_POINT('',#57632);
#18350=VERTEX_POINT('',#57634);
#18351=VERTEX_POINT('',#57636);
#18352=VERTEX_POINT('',#57638);
#18353=VERTEX_POINT('',#57640);
#18354=VERTEX_POINT('',#57642);
#18355=VERTEX_POINT('',#57644);
#18356=VERTEX_POINT('',#57646);
#18357=VERTEX_POINT('',#57648);
#18358=VERTEX_POINT('',#57651);
#18359=VERTEX_POINT('',#57652);
#18360=VERTEX_POINT('',#57654);
#18361=VERTEX_POINT('',#57656);
#18362=VERTEX_POINT('',#57658);
#18363=VERTEX_POINT('',#57660);
#18364=VERTEX_POINT('',#57662);
#18365=VERTEX_POINT('',#57664);
#18366=VERTEX_POINT('',#57666);
#18367=VERTEX_POINT('',#57668);
#18368=VERTEX_POINT('',#57670);
#18369=VERTEX_POINT('',#57672);
#18370=VERTEX_POINT('',#57676);
#18371=VERTEX_POINT('',#57677);
#18372=VERTEX_POINT('',#57679);
#18373=VERTEX_POINT('',#57682);
#18374=VERTEX_POINT('',#57686);
#18375=VERTEX_POINT('',#57687);
#18376=VERTEX_POINT('',#57692);
#18377=VERTEX_POINT('',#57693);
#18378=VERTEX_POINT('',#57695);
#18379=VERTEX_POINT('',#57698);
#18380=VERTEX_POINT('',#57702);
#18381=VERTEX_POINT('',#57703);
#18382=VERTEX_POINT('',#57708);
#18383=VERTEX_POINT('',#57711);
#18384=VERTEX_POINT('',#57717);
#18385=VERTEX_POINT('',#57720);
#18386=VERTEX_POINT('',#57726);
#18387=VERTEX_POINT('',#57730);
#18388=VERTEX_POINT('',#57818);
#18389=VERTEX_POINT('',#57819);
#18390=VERTEX_POINT('',#57821);
#18391=VERTEX_POINT('',#57823);
#18392=VERTEX_POINT('',#57826);
#18393=VERTEX_POINT('',#57827);
#18394=VERTEX_POINT('',#57829);
#18395=VERTEX_POINT('',#57831);
#18396=VERTEX_POINT('',#57843);
#18397=VERTEX_POINT('',#57844);
#18398=VERTEX_POINT('',#57846);
#18399=VERTEX_POINT('',#57848);
#18400=VERTEX_POINT('',#57852);
#18401=VERTEX_POINT('',#57854);
#18402=VERTEX_POINT('',#57858);
#18403=VERTEX_POINT('',#57860);
#18404=VERTEX_POINT('',#57872);
#18405=VERTEX_POINT('',#57874);
#18406=VERTEX_POINT('',#57878);
#18407=VERTEX_POINT('',#57882);
#18408=VERTEX_POINT('',#57888);
#18409=VERTEX_POINT('',#57889);
#18410=VERTEX_POINT('',#57891);
#18411=VERTEX_POINT('',#57893);
#18412=VERTEX_POINT('',#57897);
#18413=VERTEX_POINT('',#57898);
#18414=VERTEX_POINT('',#57900);
#18415=VERTEX_POINT('',#57902);
#18416=VERTEX_POINT('',#57906);
#18417=VERTEX_POINT('',#57908);
#18418=VERTEX_POINT('',#57912);
#18419=VERTEX_POINT('',#57913);
#18420=VERTEX_POINT('',#57926);
#18421=VERTEX_POINT('',#57927);
#18422=VERTEX_POINT('',#57929);
#18423=VERTEX_POINT('',#57931);
#18424=VERTEX_POINT('',#57934);
#18425=VERTEX_POINT('',#57935);
#18426=VERTEX_POINT('',#57937);
#18427=VERTEX_POINT('',#57939);
#18428=VERTEX_POINT('',#57951);
#18429=VERTEX_POINT('',#57952);
#18430=VERTEX_POINT('',#57954);
#18431=VERTEX_POINT('',#57956);
#18432=VERTEX_POINT('',#57960);
#18433=VERTEX_POINT('',#57961);
#18434=VERTEX_POINT('',#57966);
#18435=VERTEX_POINT('',#57968);
#18436=VERTEX_POINT('',#57981);
#18437=VERTEX_POINT('',#57982);
#18438=VERTEX_POINT('',#57984);
#18439=VERTEX_POINT('',#57986);
#18440=VERTEX_POINT('',#57990);
#18441=VERTEX_POINT('',#57991);
#18442=VERTEX_POINT('',#57993);
#18443=VERTEX_POINT('',#57995);
#18444=VERTEX_POINT('',#58007);
#18445=VERTEX_POINT('',#58009);
#18446=VERTEX_POINT('',#58013);
#18447=VERTEX_POINT('',#58015);
#18448=VERTEX_POINT('',#58019);
#18449=VERTEX_POINT('',#58020);
#18450=VERTEX_POINT('',#58022);
#18451=VERTEX_POINT('',#58024);
#18452=VERTEX_POINT('',#58028);
#18453=VERTEX_POINT('',#58029);
#18454=VERTEX_POINT('',#58031);
#18455=VERTEX_POINT('',#58033);
#18456=VERTEX_POINT('',#58037);
#18457=VERTEX_POINT('',#58038);
#18458=VERTEX_POINT('',#58040);
#18459=VERTEX_POINT('',#58042);
#18460=VERTEX_POINT('',#58046);
#18461=VERTEX_POINT('',#58048);
#18462=VERTEX_POINT('',#58050);
#18463=VERTEX_POINT('',#58052);
#18464=VERTEX_POINT('',#58056);
#18465=VERTEX_POINT('',#58058);
#18466=VERTEX_POINT('',#58060);
#18467=VERTEX_POINT('',#58062);
#18468=VERTEX_POINT('',#58066);
#18469=VERTEX_POINT('',#58067);
#18470=VERTEX_POINT('',#58069);
#18471=VERTEX_POINT('',#58071);
#18472=VERTEX_POINT('',#58075);
#18473=VERTEX_POINT('',#58076);
#18474=VERTEX_POINT('',#58078);
#18475=VERTEX_POINT('',#58080);
#18476=VERTEX_POINT('',#58084);
#18477=VERTEX_POINT('',#58086);
#18478=VERTEX_POINT('',#58088);
#18479=VERTEX_POINT('',#58090);
#18480=VERTEX_POINT('',#58094);
#18481=VERTEX_POINT('',#58096);
#18482=VERTEX_POINT('',#58098);
#18483=VERTEX_POINT('',#58100);
#18484=VERTEX_POINT('',#58104);
#18485=VERTEX_POINT('',#58105);
#18486=VERTEX_POINT('',#58107);
#18487=VERTEX_POINT('',#58109);
#18488=VERTEX_POINT('',#58112);
#18489=VERTEX_POINT('',#58113);
#18490=VERTEX_POINT('',#58118);
#18491=VERTEX_POINT('',#58119);
#18492=VERTEX_POINT('',#58125);
#18493=VERTEX_POINT('',#58126);
#18494=VERTEX_POINT('',#58128);
#18495=VERTEX_POINT('',#58130);
#18496=VERTEX_POINT('',#58133);
#18497=VERTEX_POINT('',#58134);
#18498=VERTEX_POINT('',#58136);
#18499=VERTEX_POINT('',#58138);
#18500=VERTEX_POINT('',#58140);
#18501=VERTEX_POINT('',#58142);
#18502=VERTEX_POINT('',#58144);
#18503=VERTEX_POINT('',#58146);
#18504=VERTEX_POINT('',#58148);
#18505=VERTEX_POINT('',#58150);
#18506=VERTEX_POINT('',#58154);
#18507=VERTEX_POINT('',#58156);
#18508=VERTEX_POINT('',#58160);
#18509=VERTEX_POINT('',#58164);
#18510=VERTEX_POINT('',#58170);
#18511=VERTEX_POINT('',#58171);
#18512=VERTEX_POINT('',#58173);
#18513=VERTEX_POINT('',#58175);
#18514=VERTEX_POINT('',#58179);
#18515=VERTEX_POINT('',#58182);
#18516=VERTEX_POINT('',#58184);
#18517=VERTEX_POINT('',#58187);
#18518=VERTEX_POINT('',#58189);
#18519=VERTEX_POINT('',#58192);
#18520=VERTEX_POINT('',#58194);
#18521=VERTEX_POINT('',#58197);
#18522=VERTEX_POINT('',#58199);
#18523=VERTEX_POINT('',#58203);
#18524=VERTEX_POINT('',#58207);
#18525=VERTEX_POINT('',#58210);
#18526=VERTEX_POINT('',#58212);
#18527=VERTEX_POINT('',#58215);
#18528=VERTEX_POINT('',#58217);
#18529=VERTEX_POINT('',#58220);
#18530=VERTEX_POINT('',#58223);
#18531=VERTEX_POINT('',#58225);
#18532=VERTEX_POINT('',#58233);
#18533=VERTEX_POINT('',#58237);
#18534=VERTEX_POINT('',#58241);
#18535=VERTEX_POINT('',#58243);
#18536=VERTEX_POINT('',#58247);
#18537=VERTEX_POINT('',#58249);
#18538=VERTEX_POINT('',#58256);
#18539=VERTEX_POINT('',#58260);
#18540=VERTEX_POINT('',#58264);
#18541=VERTEX_POINT('',#58266);
#18542=VERTEX_POINT('',#58270);
#18543=VERTEX_POINT('',#58272);
#18544=VERTEX_POINT('',#58278);
#18545=VERTEX_POINT('',#58280);
#18546=VERTEX_POINT('',#58285);
#18547=VERTEX_POINT('',#58287);
#18548=VERTEX_POINT('',#58295);
#18549=VERTEX_POINT('',#58297);
#18550=VERTEX_POINT('',#58302);
#18551=VERTEX_POINT('',#58304);
#18552=VERTEX_POINT('',#58343);
#18553=VERTEX_POINT('',#58346);
#18554=VERTEX_POINT('',#58350);
#18555=VERTEX_POINT('',#58352);
#18556=VERTEX_POINT('',#58356);
#18557=VERTEX_POINT('',#58358);
#18558=VERTEX_POINT('',#58362);
#18559=VERTEX_POINT('',#58366);
#18560=VERTEX_POINT('',#58370);
#18561=VERTEX_POINT('',#58371);
#18562=VERTEX_POINT('',#58373);
#18563=VERTEX_POINT('',#58375);
#18564=VERTEX_POINT('',#58377);
#18565=VERTEX_POINT('',#58379);
#18566=VERTEX_POINT('',#58381);
#18567=VERTEX_POINT('',#58383);
#18568=VERTEX_POINT('',#58385);
#18569=VERTEX_POINT('',#58387);
#18570=VERTEX_POINT('',#58389);
#18571=VERTEX_POINT('',#58391);
#18572=VERTEX_POINT('',#58395);
#18573=VERTEX_POINT('',#58396);
#18574=VERTEX_POINT('',#58398);
#18575=VERTEX_POINT('',#58400);
#18576=VERTEX_POINT('',#58402);
#18577=VERTEX_POINT('',#58404);
#18578=VERTEX_POINT('',#58406);
#18579=VERTEX_POINT('',#58408);
#18580=VERTEX_POINT('',#58410);
#18581=VERTEX_POINT('',#58412);
#18582=VERTEX_POINT('',#58414);
#18583=VERTEX_POINT('',#58416);
#18584=VERTEX_POINT('',#58440);
#18585=VERTEX_POINT('',#58441);
#18586=VERTEX_POINT('',#58446);
#18587=VERTEX_POINT('',#58448);
#18588=VERTEX_POINT('',#58456);
#18589=VERTEX_POINT('',#58458);
#18590=VERTEX_POINT('',#58462);
#18591=VERTEX_POINT('',#58463);
#18592=VERTEX_POINT('',#58472);
#18593=VERTEX_POINT('',#58473);
#18594=VERTEX_POINT('',#58475);
#18595=VERTEX_POINT('',#58477);
#18596=VERTEX_POINT('',#58481);
#18597=VERTEX_POINT('',#58482);
#18598=VERTEX_POINT('',#58484);
#18599=VERTEX_POINT('',#58486);
#18600=VERTEX_POINT('',#58490);
#18601=VERTEX_POINT('',#58491);
#18602=VERTEX_POINT('',#58493);
#18603=VERTEX_POINT('',#58495);
#18604=VERTEX_POINT('',#58516);
#18605=VERTEX_POINT('',#58517);
#18606=VERTEX_POINT('',#58522);
#18607=VERTEX_POINT('',#58524);
#18608=VERTEX_POINT('',#58532);
#18609=VERTEX_POINT('',#58534);
#18610=VERTEX_POINT('',#58538);
#18611=VERTEX_POINT('',#58539);
#18612=VERTEX_POINT('',#58548);
#18613=VERTEX_POINT('',#58549);
#18614=VERTEX_POINT('',#58551);
#18615=VERTEX_POINT('',#58553);
#18616=VERTEX_POINT('',#58557);
#18617=VERTEX_POINT('',#58558);
#18618=VERTEX_POINT('',#58560);
#18619=VERTEX_POINT('',#58562);
#18620=VERTEX_POINT('',#58566);
#18621=VERTEX_POINT('',#58567);
#18622=VERTEX_POINT('',#58569);
#18623=VERTEX_POINT('',#58571);
#18624=VERTEX_POINT('',#58592);
#18625=VERTEX_POINT('',#58593);
#18626=VERTEX_POINT('',#58595);
#18627=VERTEX_POINT('',#58597);
#18628=VERTEX_POINT('',#58599);
#18629=VERTEX_POINT('',#58601);
#18630=VERTEX_POINT('',#58604);
#18631=VERTEX_POINT('',#58605);
#18632=VERTEX_POINT('',#58607);
#18633=VERTEX_POINT('',#58609);
#18634=VERTEX_POINT('',#58611);
#18635=VERTEX_POINT('',#58613);
#18636=VERTEX_POINT('',#58616);
#18637=VERTEX_POINT('',#58617);
#18638=VERTEX_POINT('',#58619);
#18639=VERTEX_POINT('',#58621);
#18640=VERTEX_POINT('',#58623);
#18641=VERTEX_POINT('',#58625);
#18642=VERTEX_POINT('',#58628);
#18643=VERTEX_POINT('',#58629);
#18644=VERTEX_POINT('',#58631);
#18645=VERTEX_POINT('',#58633);
#18646=VERTEX_POINT('',#58635);
#18647=VERTEX_POINT('',#58637);
#18648=VERTEX_POINT('',#58640);
#18649=VERTEX_POINT('',#58641);
#18650=VERTEX_POINT('',#58643);
#18651=VERTEX_POINT('',#58645);
#18652=VERTEX_POINT('',#58647);
#18653=VERTEX_POINT('',#58649);
#18654=VERTEX_POINT('',#58652);
#18655=VERTEX_POINT('',#58653);
#18656=VERTEX_POINT('',#58655);
#18657=VERTEX_POINT('',#58657);
#18658=VERTEX_POINT('',#58659);
#18659=VERTEX_POINT('',#58661);
#18660=VERTEX_POINT('',#58664);
#18661=VERTEX_POINT('',#58665);
#18662=VERTEX_POINT('',#58667);
#18663=VERTEX_POINT('',#58669);
#18664=VERTEX_POINT('',#58671);
#18665=VERTEX_POINT('',#58673);
#18666=VERTEX_POINT('',#58676);
#18667=VERTEX_POINT('',#58677);
#18668=VERTEX_POINT('',#58679);
#18669=VERTEX_POINT('',#58681);
#18670=VERTEX_POINT('',#58683);
#18671=VERTEX_POINT('',#58685);
#18672=VERTEX_POINT('',#58688);
#18673=VERTEX_POINT('',#58689);
#18674=VERTEX_POINT('',#58691);
#18675=VERTEX_POINT('',#58693);
#18676=VERTEX_POINT('',#58695);
#18677=VERTEX_POINT('',#58697);
#18678=VERTEX_POINT('',#58700);
#18679=VERTEX_POINT('',#58701);
#18680=VERTEX_POINT('',#58703);
#18681=VERTEX_POINT('',#58705);
#18682=VERTEX_POINT('',#58707);
#18683=VERTEX_POINT('',#58709);
#18684=VERTEX_POINT('',#58712);
#18685=VERTEX_POINT('',#58713);
#18686=VERTEX_POINT('',#58715);
#18687=VERTEX_POINT('',#58717);
#18688=VERTEX_POINT('',#58719);
#18689=VERTEX_POINT('',#58721);
#18690=VERTEX_POINT('',#58724);
#18691=VERTEX_POINT('',#58725);
#18692=VERTEX_POINT('',#58727);
#18693=VERTEX_POINT('',#58729);
#18694=VERTEX_POINT('',#58731);
#18695=VERTEX_POINT('',#58733);
#18696=VERTEX_POINT('',#58736);
#18697=VERTEX_POINT('',#58737);
#18698=VERTEX_POINT('',#58739);
#18699=VERTEX_POINT('',#58741);
#18700=VERTEX_POINT('',#58743);
#18701=VERTEX_POINT('',#58745);
#18702=VERTEX_POINT('',#58748);
#18703=VERTEX_POINT('',#58749);
#18704=VERTEX_POINT('',#58751);
#18705=VERTEX_POINT('',#58753);
#18706=VERTEX_POINT('',#58755);
#18707=VERTEX_POINT('',#58757);
#18708=VERTEX_POINT('',#58760);
#18709=VERTEX_POINT('',#58761);
#18710=VERTEX_POINT('',#58763);
#18711=VERTEX_POINT('',#58765);
#18712=VERTEX_POINT('',#58767);
#18713=VERTEX_POINT('',#58769);
#18714=VERTEX_POINT('',#58772);
#18715=VERTEX_POINT('',#58773);
#18716=VERTEX_POINT('',#58775);
#18717=VERTEX_POINT('',#58777);
#18718=VERTEX_POINT('',#58779);
#18719=VERTEX_POINT('',#58781);
#18720=VERTEX_POINT('',#58784);
#18721=VERTEX_POINT('',#58785);
#18722=VERTEX_POINT('',#58787);
#18723=VERTEX_POINT('',#58789);
#18724=VERTEX_POINT('',#58791);
#18725=VERTEX_POINT('',#58793);
#18726=VERTEX_POINT('',#58796);
#18727=VERTEX_POINT('',#58797);
#18728=VERTEX_POINT('',#58799);
#18729=VERTEX_POINT('',#58801);
#18730=VERTEX_POINT('',#58803);
#18731=VERTEX_POINT('',#58805);
#18732=VERTEX_POINT('',#58808);
#18733=VERTEX_POINT('',#58809);
#18734=VERTEX_POINT('',#58811);
#18735=VERTEX_POINT('',#58813);
#18736=VERTEX_POINT('',#58815);
#18737=VERTEX_POINT('',#58817);
#18738=VERTEX_POINT('',#58820);
#18739=VERTEX_POINT('',#58821);
#18740=VERTEX_POINT('',#58823);
#18741=VERTEX_POINT('',#58825);
#18742=VERTEX_POINT('',#58827);
#18743=VERTEX_POINT('',#58829);
#18744=VERTEX_POINT('',#58832);
#18745=VERTEX_POINT('',#58833);
#18746=VERTEX_POINT('',#58835);
#18747=VERTEX_POINT('',#58837);
#18748=VERTEX_POINT('',#58839);
#18749=VERTEX_POINT('',#58841);
#18750=VERTEX_POINT('',#58844);
#18751=VERTEX_POINT('',#58845);
#18752=VERTEX_POINT('',#58847);
#18753=VERTEX_POINT('',#58849);
#18754=VERTEX_POINT('',#58851);
#18755=VERTEX_POINT('',#58853);
#18756=VERTEX_POINT('',#58856);
#18757=VERTEX_POINT('',#58857);
#18758=VERTEX_POINT('',#58859);
#18759=VERTEX_POINT('',#58861);
#18760=VERTEX_POINT('',#58863);
#18761=VERTEX_POINT('',#58865);
#18762=VERTEX_POINT('',#58868);
#18763=VERTEX_POINT('',#58869);
#18764=VERTEX_POINT('',#58871);
#18765=VERTEX_POINT('',#58873);
#18766=VERTEX_POINT('',#58875);
#18767=VERTEX_POINT('',#58877);
#18768=VERTEX_POINT('',#58880);
#18769=VERTEX_POINT('',#58881);
#18770=VERTEX_POINT('',#58883);
#18771=VERTEX_POINT('',#58885);
#18772=VERTEX_POINT('',#58887);
#18773=VERTEX_POINT('',#58889);
#18774=VERTEX_POINT('',#58892);
#18775=VERTEX_POINT('',#58893);
#18776=VERTEX_POINT('',#58895);
#18777=VERTEX_POINT('',#58897);
#18778=VERTEX_POINT('',#58899);
#18779=VERTEX_POINT('',#58901);
#18780=VERTEX_POINT('',#58904);
#18781=VERTEX_POINT('',#58905);
#18782=VERTEX_POINT('',#58907);
#18783=VERTEX_POINT('',#58909);
#18784=VERTEX_POINT('',#58911);
#18785=VERTEX_POINT('',#58913);
#18786=VERTEX_POINT('',#58916);
#18787=VERTEX_POINT('',#58917);
#18788=VERTEX_POINT('',#58919);
#18789=VERTEX_POINT('',#58921);
#18790=VERTEX_POINT('',#58923);
#18791=VERTEX_POINT('',#58925);
#18792=VERTEX_POINT('',#58928);
#18793=VERTEX_POINT('',#58929);
#18794=VERTEX_POINT('',#58931);
#18795=VERTEX_POINT('',#58933);
#18796=VERTEX_POINT('',#58935);
#18797=VERTEX_POINT('',#58937);
#18798=VERTEX_POINT('',#58940);
#18799=VERTEX_POINT('',#58941);
#18800=VERTEX_POINT('',#58943);
#18801=VERTEX_POINT('',#58945);
#18802=VERTEX_POINT('',#58947);
#18803=VERTEX_POINT('',#58949);
#18804=VERTEX_POINT('',#58952);
#18805=VERTEX_POINT('',#58953);
#18806=VERTEX_POINT('',#58955);
#18807=VERTEX_POINT('',#58957);
#18808=VERTEX_POINT('',#58959);
#18809=VERTEX_POINT('',#58961);
#18810=VERTEX_POINT('',#58964);
#18811=VERTEX_POINT('',#58965);
#18812=VERTEX_POINT('',#58967);
#18813=VERTEX_POINT('',#58969);
#18814=VERTEX_POINT('',#58971);
#18815=VERTEX_POINT('',#58973);
#18816=VERTEX_POINT('',#58976);
#18817=VERTEX_POINT('',#58977);
#18818=VERTEX_POINT('',#58979);
#18819=VERTEX_POINT('',#58981);
#18820=VERTEX_POINT('',#58983);
#18821=VERTEX_POINT('',#58985);
#18822=VERTEX_POINT('',#58988);
#18823=VERTEX_POINT('',#58989);
#18824=VERTEX_POINT('',#58991);
#18825=VERTEX_POINT('',#58993);
#18826=VERTEX_POINT('',#58995);
#18827=VERTEX_POINT('',#58997);
#18828=VERTEX_POINT('',#59000);
#18829=VERTEX_POINT('',#59001);
#18830=VERTEX_POINT('',#59003);
#18831=VERTEX_POINT('',#59005);
#18832=VERTEX_POINT('',#59007);
#18833=VERTEX_POINT('',#59009);
#18834=VERTEX_POINT('',#59012);
#18835=VERTEX_POINT('',#59013);
#18836=VERTEX_POINT('',#59015);
#18837=VERTEX_POINT('',#59017);
#18838=VERTEX_POINT('',#59019);
#18839=VERTEX_POINT('',#59021);
#18840=VERTEX_POINT('',#59024);
#18841=VERTEX_POINT('',#59025);
#18842=VERTEX_POINT('',#59027);
#18843=VERTEX_POINT('',#59029);
#18844=VERTEX_POINT('',#59031);
#18845=VERTEX_POINT('',#59033);
#18846=VERTEX_POINT('',#59036);
#18847=VERTEX_POINT('',#59037);
#18848=VERTEX_POINT('',#59039);
#18849=VERTEX_POINT('',#59041);
#18850=VERTEX_POINT('',#59043);
#18851=VERTEX_POINT('',#59045);
#18852=VERTEX_POINT('',#59048);
#18853=VERTEX_POINT('',#59049);
#18854=VERTEX_POINT('',#59051);
#18855=VERTEX_POINT('',#59053);
#18856=VERTEX_POINT('',#59055);
#18857=VERTEX_POINT('',#59057);
#18858=VERTEX_POINT('',#59060);
#18859=VERTEX_POINT('',#59061);
#18860=VERTEX_POINT('',#59063);
#18861=VERTEX_POINT('',#59065);
#18862=VERTEX_POINT('',#59067);
#18863=VERTEX_POINT('',#59069);
#18864=VERTEX_POINT('',#59072);
#18865=VERTEX_POINT('',#59073);
#18866=VERTEX_POINT('',#59075);
#18867=VERTEX_POINT('',#59077);
#18868=VERTEX_POINT('',#59079);
#18869=VERTEX_POINT('',#59081);
#18870=VERTEX_POINT('',#59084);
#18871=VERTEX_POINT('',#59085);
#18872=VERTEX_POINT('',#59087);
#18873=VERTEX_POINT('',#59089);
#18874=VERTEX_POINT('',#59091);
#18875=VERTEX_POINT('',#59093);
#18876=VERTEX_POINT('',#59096);
#18877=VERTEX_POINT('',#59097);
#18878=VERTEX_POINT('',#59099);
#18879=VERTEX_POINT('',#59101);
#18880=VERTEX_POINT('',#59103);
#18881=VERTEX_POINT('',#59105);
#18882=VERTEX_POINT('',#59108);
#18883=VERTEX_POINT('',#59109);
#18884=VERTEX_POINT('',#59111);
#18885=VERTEX_POINT('',#59113);
#18886=VERTEX_POINT('',#59115);
#18887=VERTEX_POINT('',#59117);
#18888=VERTEX_POINT('',#59120);
#18889=VERTEX_POINT('',#59121);
#18890=VERTEX_POINT('',#59123);
#18891=VERTEX_POINT('',#59125);
#18892=VERTEX_POINT('',#59127);
#18893=VERTEX_POINT('',#59129);
#18894=VERTEX_POINT('',#59132);
#18895=VERTEX_POINT('',#59133);
#18896=VERTEX_POINT('',#59135);
#18897=VERTEX_POINT('',#59137);
#18898=VERTEX_POINT('',#59139);
#18899=VERTEX_POINT('',#59141);
#18900=VERTEX_POINT('',#59144);
#18901=VERTEX_POINT('',#59145);
#18902=VERTEX_POINT('',#59147);
#18903=VERTEX_POINT('',#59149);
#18904=VERTEX_POINT('',#59151);
#18905=VERTEX_POINT('',#59153);
#18906=VERTEX_POINT('',#59156);
#18907=VERTEX_POINT('',#59157);
#18908=VERTEX_POINT('',#59159);
#18909=VERTEX_POINT('',#59161);
#18910=VERTEX_POINT('',#59163);
#18911=VERTEX_POINT('',#59165);
#18912=VERTEX_POINT('',#59168);
#18913=VERTEX_POINT('',#59169);
#18914=VERTEX_POINT('',#59171);
#18915=VERTEX_POINT('',#59173);
#18916=VERTEX_POINT('',#59175);
#18917=VERTEX_POINT('',#59177);
#18918=VERTEX_POINT('',#59180);
#18919=VERTEX_POINT('',#59181);
#18920=VERTEX_POINT('',#59183);
#18921=VERTEX_POINT('',#59185);
#18922=VERTEX_POINT('',#59187);
#18923=VERTEX_POINT('',#59189);
#18924=VERTEX_POINT('',#59192);
#18925=VERTEX_POINT('',#59193);
#18926=VERTEX_POINT('',#59195);
#18927=VERTEX_POINT('',#59197);
#18928=VERTEX_POINT('',#59199);
#18929=VERTEX_POINT('',#59201);
#18930=VERTEX_POINT('',#59204);
#18931=VERTEX_POINT('',#59205);
#18932=VERTEX_POINT('',#59207);
#18933=VERTEX_POINT('',#59209);
#18934=VERTEX_POINT('',#59211);
#18935=VERTEX_POINT('',#59213);
#18936=VERTEX_POINT('',#59216);
#18937=VERTEX_POINT('',#59217);
#18938=VERTEX_POINT('',#59219);
#18939=VERTEX_POINT('',#59221);
#18940=VERTEX_POINT('',#59223);
#18941=VERTEX_POINT('',#59225);
#18942=VERTEX_POINT('',#59228);
#18943=VERTEX_POINT('',#59229);
#18944=VERTEX_POINT('',#59231);
#18945=VERTEX_POINT('',#59233);
#18946=VERTEX_POINT('',#59235);
#18947=VERTEX_POINT('',#59237);
#18948=VERTEX_POINT('',#59240);
#18949=VERTEX_POINT('',#59241);
#18950=VERTEX_POINT('',#59243);
#18951=VERTEX_POINT('',#59245);
#18952=VERTEX_POINT('',#59247);
#18953=VERTEX_POINT('',#59249);
#18954=VERTEX_POINT('',#59252);
#18955=VERTEX_POINT('',#59253);
#18956=VERTEX_POINT('',#59255);
#18957=VERTEX_POINT('',#59257);
#18958=VERTEX_POINT('',#59259);
#18959=VERTEX_POINT('',#59261);
#18960=VERTEX_POINT('',#59264);
#18961=VERTEX_POINT('',#59265);
#18962=VERTEX_POINT('',#59267);
#18963=VERTEX_POINT('',#59269);
#18964=VERTEX_POINT('',#59271);
#18965=VERTEX_POINT('',#59273);
#18966=VERTEX_POINT('',#59276);
#18967=VERTEX_POINT('',#59277);
#18968=VERTEX_POINT('',#59279);
#18969=VERTEX_POINT('',#59281);
#18970=VERTEX_POINT('',#59283);
#18971=VERTEX_POINT('',#59285);
#18972=VERTEX_POINT('',#59288);
#18973=VERTEX_POINT('',#59289);
#18974=VERTEX_POINT('',#59291);
#18975=VERTEX_POINT('',#59293);
#18976=VERTEX_POINT('',#59295);
#18977=VERTEX_POINT('',#59297);
#18978=VERTEX_POINT('',#59300);
#18979=VERTEX_POINT('',#59301);
#18980=VERTEX_POINT('',#59303);
#18981=VERTEX_POINT('',#59305);
#18982=VERTEX_POINT('',#59307);
#18983=VERTEX_POINT('',#59309);
#18984=VERTEX_POINT('',#59312);
#18985=VERTEX_POINT('',#59313);
#18986=VERTEX_POINT('',#59315);
#18987=VERTEX_POINT('',#59317);
#18988=VERTEX_POINT('',#59319);
#18989=VERTEX_POINT('',#59321);
#18990=VERTEX_POINT('',#59324);
#18991=VERTEX_POINT('',#59325);
#18992=VERTEX_POINT('',#59327);
#18993=VERTEX_POINT('',#59329);
#18994=VERTEX_POINT('',#59331);
#18995=VERTEX_POINT('',#59333);
#18996=VERTEX_POINT('',#59336);
#18997=VERTEX_POINT('',#59337);
#18998=VERTEX_POINT('',#59339);
#18999=VERTEX_POINT('',#59341);
#19000=VERTEX_POINT('',#59343);
#19001=VERTEX_POINT('',#59345);
#19002=VERTEX_POINT('',#59348);
#19003=VERTEX_POINT('',#59349);
#19004=VERTEX_POINT('',#59351);
#19005=VERTEX_POINT('',#59353);
#19006=VERTEX_POINT('',#59355);
#19007=VERTEX_POINT('',#59357);
#19008=VERTEX_POINT('',#59360);
#19009=VERTEX_POINT('',#59361);
#19010=VERTEX_POINT('',#59363);
#19011=VERTEX_POINT('',#59365);
#19012=VERTEX_POINT('',#59367);
#19013=VERTEX_POINT('',#59369);
#19014=VERTEX_POINT('',#59372);
#19015=VERTEX_POINT('',#59373);
#19016=VERTEX_POINT('',#59375);
#19017=VERTEX_POINT('',#59377);
#19018=VERTEX_POINT('',#59379);
#19019=VERTEX_POINT('',#59381);
#19020=VERTEX_POINT('',#59384);
#19021=VERTEX_POINT('',#59385);
#19022=VERTEX_POINT('',#59387);
#19023=VERTEX_POINT('',#59389);
#19024=VERTEX_POINT('',#59391);
#19025=VERTEX_POINT('',#59393);
#19026=VERTEX_POINT('',#59396);
#19027=VERTEX_POINT('',#59397);
#19028=VERTEX_POINT('',#59399);
#19029=VERTEX_POINT('',#59401);
#19030=VERTEX_POINT('',#59403);
#19031=VERTEX_POINT('',#59405);
#19032=VERTEX_POINT('',#59408);
#19033=VERTEX_POINT('',#59409);
#19034=VERTEX_POINT('',#59411);
#19035=VERTEX_POINT('',#59413);
#19036=VERTEX_POINT('',#59415);
#19037=VERTEX_POINT('',#59417);
#19038=VERTEX_POINT('',#59420);
#19039=VERTEX_POINT('',#59421);
#19040=VERTEX_POINT('',#59423);
#19041=VERTEX_POINT('',#59425);
#19042=VERTEX_POINT('',#59427);
#19043=VERTEX_POINT('',#59429);
#19044=VERTEX_POINT('',#59432);
#19045=VERTEX_POINT('',#59433);
#19046=VERTEX_POINT('',#59435);
#19047=VERTEX_POINT('',#59437);
#19048=VERTEX_POINT('',#59439);
#19049=VERTEX_POINT('',#59441);
#19050=VERTEX_POINT('',#59444);
#19051=VERTEX_POINT('',#59445);
#19052=VERTEX_POINT('',#59447);
#19053=VERTEX_POINT('',#59449);
#19054=VERTEX_POINT('',#59451);
#19055=VERTEX_POINT('',#59453);
#19056=VERTEX_POINT('',#59456);
#19057=VERTEX_POINT('',#59457);
#19058=VERTEX_POINT('',#59459);
#19059=VERTEX_POINT('',#59461);
#19060=VERTEX_POINT('',#59463);
#19061=VERTEX_POINT('',#59465);
#19062=VERTEX_POINT('',#59468);
#19063=VERTEX_POINT('',#59469);
#19064=VERTEX_POINT('',#59471);
#19065=VERTEX_POINT('',#59473);
#19066=VERTEX_POINT('',#59475);
#19067=VERTEX_POINT('',#59477);
#19068=VERTEX_POINT('',#59480);
#19069=VERTEX_POINT('',#59481);
#19070=VERTEX_POINT('',#59483);
#19071=VERTEX_POINT('',#59485);
#19072=VERTEX_POINT('',#59487);
#19073=VERTEX_POINT('',#59489);
#19074=VERTEX_POINT('',#59492);
#19075=VERTEX_POINT('',#59493);
#19076=VERTEX_POINT('',#59495);
#19077=VERTEX_POINT('',#59497);
#19078=VERTEX_POINT('',#59499);
#19079=VERTEX_POINT('',#59501);
#19080=VERTEX_POINT('',#59504);
#19081=VERTEX_POINT('',#59505);
#19082=VERTEX_POINT('',#59507);
#19083=VERTEX_POINT('',#59509);
#19084=VERTEX_POINT('',#59511);
#19085=VERTEX_POINT('',#59513);
#19086=VERTEX_POINT('',#59516);
#19087=VERTEX_POINT('',#59517);
#19088=VERTEX_POINT('',#59519);
#19089=VERTEX_POINT('',#59521);
#19090=VERTEX_POINT('',#59523);
#19091=VERTEX_POINT('',#59525);
#19092=VERTEX_POINT('',#59528);
#19093=VERTEX_POINT('',#59529);
#19094=VERTEX_POINT('',#59531);
#19095=VERTEX_POINT('',#59533);
#19096=VERTEX_POINT('',#59535);
#19097=VERTEX_POINT('',#59537);
#19098=VERTEX_POINT('',#59540);
#19099=VERTEX_POINT('',#59541);
#19100=VERTEX_POINT('',#59543);
#19101=VERTEX_POINT('',#59545);
#19102=VERTEX_POINT('',#59547);
#19103=VERTEX_POINT('',#59549);
#19104=VERTEX_POINT('',#59552);
#19105=VERTEX_POINT('',#59553);
#19106=VERTEX_POINT('',#59555);
#19107=VERTEX_POINT('',#59557);
#19108=VERTEX_POINT('',#59559);
#19109=VERTEX_POINT('',#59561);
#19110=VERTEX_POINT('',#59564);
#19111=VERTEX_POINT('',#59565);
#19112=VERTEX_POINT('',#59567);
#19113=VERTEX_POINT('',#59569);
#19114=VERTEX_POINT('',#59571);
#19115=VERTEX_POINT('',#59573);
#19116=VERTEX_POINT('',#59576);
#19117=VERTEX_POINT('',#59577);
#19118=VERTEX_POINT('',#59579);
#19119=VERTEX_POINT('',#59581);
#19120=VERTEX_POINT('',#59583);
#19121=VERTEX_POINT('',#59585);
#19122=VERTEX_POINT('',#59588);
#19123=VERTEX_POINT('',#59589);
#19124=VERTEX_POINT('',#59591);
#19125=VERTEX_POINT('',#59593);
#19126=VERTEX_POINT('',#59595);
#19127=VERTEX_POINT('',#59597);
#19128=VERTEX_POINT('',#59600);
#19129=VERTEX_POINT('',#59601);
#19130=VERTEX_POINT('',#59603);
#19131=VERTEX_POINT('',#59605);
#19132=VERTEX_POINT('',#59607);
#19133=VERTEX_POINT('',#59609);
#19134=VERTEX_POINT('',#59612);
#19135=VERTEX_POINT('',#59613);
#19136=VERTEX_POINT('',#59615);
#19137=VERTEX_POINT('',#59617);
#19138=VERTEX_POINT('',#59619);
#19139=VERTEX_POINT('',#59621);
#19140=VERTEX_POINT('',#59624);
#19141=VERTEX_POINT('',#59625);
#19142=VERTEX_POINT('',#59627);
#19143=VERTEX_POINT('',#59629);
#19144=VERTEX_POINT('',#59631);
#19145=VERTEX_POINT('',#59633);
#19146=VERTEX_POINT('',#59636);
#19147=VERTEX_POINT('',#59637);
#19148=VERTEX_POINT('',#59639);
#19149=VERTEX_POINT('',#59641);
#19150=VERTEX_POINT('',#59643);
#19151=VERTEX_POINT('',#59645);
#19152=VERTEX_POINT('',#59648);
#19153=VERTEX_POINT('',#59649);
#19154=VERTEX_POINT('',#59651);
#19155=VERTEX_POINT('',#59653);
#19156=VERTEX_POINT('',#59655);
#19157=VERTEX_POINT('',#59657);
#19158=VERTEX_POINT('',#59660);
#19159=VERTEX_POINT('',#59661);
#19160=VERTEX_POINT('',#59663);
#19161=VERTEX_POINT('',#59665);
#19162=VERTEX_POINT('',#59667);
#19163=VERTEX_POINT('',#59669);
#19164=VERTEX_POINT('',#59672);
#19165=VERTEX_POINT('',#59673);
#19166=VERTEX_POINT('',#59675);
#19167=VERTEX_POINT('',#59677);
#19168=VERTEX_POINT('',#59679);
#19169=VERTEX_POINT('',#59681);
#19170=VERTEX_POINT('',#59684);
#19171=VERTEX_POINT('',#59685);
#19172=VERTEX_POINT('',#59687);
#19173=VERTEX_POINT('',#59689);
#19174=VERTEX_POINT('',#59691);
#19175=VERTEX_POINT('',#59693);
#19176=VERTEX_POINT('',#59696);
#19177=VERTEX_POINT('',#59697);
#19178=VERTEX_POINT('',#59699);
#19179=VERTEX_POINT('',#59701);
#19180=VERTEX_POINT('',#59703);
#19181=VERTEX_POINT('',#59705);
#19182=VERTEX_POINT('',#59708);
#19183=VERTEX_POINT('',#59709);
#19184=VERTEX_POINT('',#59711);
#19185=VERTEX_POINT('',#59713);
#19186=VERTEX_POINT('',#59715);
#19187=VERTEX_POINT('',#59717);
#19188=VERTEX_POINT('',#59720);
#19189=VERTEX_POINT('',#59721);
#19190=VERTEX_POINT('',#59723);
#19191=VERTEX_POINT('',#59725);
#19192=VERTEX_POINT('',#59727);
#19193=VERTEX_POINT('',#59729);
#19194=VERTEX_POINT('',#59732);
#19195=VERTEX_POINT('',#59733);
#19196=VERTEX_POINT('',#59735);
#19197=VERTEX_POINT('',#59737);
#19198=VERTEX_POINT('',#59739);
#19199=VERTEX_POINT('',#59741);
#19200=VERTEX_POINT('',#59744);
#19201=VERTEX_POINT('',#59745);
#19202=VERTEX_POINT('',#59747);
#19203=VERTEX_POINT('',#59749);
#19204=VERTEX_POINT('',#59751);
#19205=VERTEX_POINT('',#59753);
#19206=VERTEX_POINT('',#59756);
#19207=VERTEX_POINT('',#59757);
#19208=VERTEX_POINT('',#59759);
#19209=VERTEX_POINT('',#59761);
#19210=VERTEX_POINT('',#59763);
#19211=VERTEX_POINT('',#59765);
#19212=VERTEX_POINT('',#59768);
#19213=VERTEX_POINT('',#59769);
#19214=VERTEX_POINT('',#59771);
#19215=VERTEX_POINT('',#59773);
#19216=VERTEX_POINT('',#59775);
#19217=VERTEX_POINT('',#59777);
#19218=VERTEX_POINT('',#59780);
#19219=VERTEX_POINT('',#59781);
#19220=VERTEX_POINT('',#59783);
#19221=VERTEX_POINT('',#59785);
#19222=VERTEX_POINT('',#59787);
#19223=VERTEX_POINT('',#59789);
#19224=VERTEX_POINT('',#59792);
#19225=VERTEX_POINT('',#59793);
#19226=VERTEX_POINT('',#59795);
#19227=VERTEX_POINT('',#59797);
#19228=VERTEX_POINT('',#59799);
#19229=VERTEX_POINT('',#59801);
#19230=VERTEX_POINT('',#59804);
#19231=VERTEX_POINT('',#59805);
#19232=VERTEX_POINT('',#59807);
#19233=VERTEX_POINT('',#59809);
#19234=VERTEX_POINT('',#59811);
#19235=VERTEX_POINT('',#59813);
#19236=VERTEX_POINT('',#59816);
#19237=VERTEX_POINT('',#59817);
#19238=VERTEX_POINT('',#59819);
#19239=VERTEX_POINT('',#59821);
#19240=VERTEX_POINT('',#59823);
#19241=VERTEX_POINT('',#59825);
#19242=VERTEX_POINT('',#59828);
#19243=VERTEX_POINT('',#59829);
#19244=VERTEX_POINT('',#59831);
#19245=VERTEX_POINT('',#59833);
#19246=VERTEX_POINT('',#59835);
#19247=VERTEX_POINT('',#59837);
#19248=VERTEX_POINT('',#59840);
#19249=VERTEX_POINT('',#59841);
#19250=VERTEX_POINT('',#59843);
#19251=VERTEX_POINT('',#59845);
#19252=VERTEX_POINT('',#59847);
#19253=VERTEX_POINT('',#59849);
#19254=VERTEX_POINT('',#59852);
#19255=VERTEX_POINT('',#59853);
#19256=VERTEX_POINT('',#59855);
#19257=VERTEX_POINT('',#59857);
#19258=VERTEX_POINT('',#59859);
#19259=VERTEX_POINT('',#59861);
#19260=VERTEX_POINT('',#59864);
#19261=VERTEX_POINT('',#59865);
#19262=VERTEX_POINT('',#59867);
#19263=VERTEX_POINT('',#59869);
#19264=VERTEX_POINT('',#59871);
#19265=VERTEX_POINT('',#59873);
#19266=VERTEX_POINT('',#59876);
#19267=VERTEX_POINT('',#59877);
#19268=VERTEX_POINT('',#59879);
#19269=VERTEX_POINT('',#59881);
#19270=VERTEX_POINT('',#59883);
#19271=VERTEX_POINT('',#59885);
#19272=VERTEX_POINT('',#59888);
#19273=VERTEX_POINT('',#59889);
#19274=VERTEX_POINT('',#59891);
#19275=VERTEX_POINT('',#59893);
#19276=VERTEX_POINT('',#59895);
#19277=VERTEX_POINT('',#59897);
#19278=VERTEX_POINT('',#59900);
#19279=VERTEX_POINT('',#59901);
#19280=VERTEX_POINT('',#59903);
#19281=VERTEX_POINT('',#59905);
#19282=VERTEX_POINT('',#59907);
#19283=VERTEX_POINT('',#59909);
#19284=VERTEX_POINT('',#59912);
#19285=VERTEX_POINT('',#59913);
#19286=VERTEX_POINT('',#59915);
#19287=VERTEX_POINT('',#59917);
#19288=VERTEX_POINT('',#59919);
#19289=VERTEX_POINT('',#59921);
#19290=VERTEX_POINT('',#59924);
#19291=VERTEX_POINT('',#59925);
#19292=VERTEX_POINT('',#59927);
#19293=VERTEX_POINT('',#59929);
#19294=VERTEX_POINT('',#59931);
#19295=VERTEX_POINT('',#59933);
#19296=VERTEX_POINT('',#59936);
#19297=VERTEX_POINT('',#59937);
#19298=VERTEX_POINT('',#59939);
#19299=VERTEX_POINT('',#59941);
#19300=VERTEX_POINT('',#59943);
#19301=VERTEX_POINT('',#59945);
#19302=VERTEX_POINT('',#59948);
#19303=VERTEX_POINT('',#59949);
#19304=VERTEX_POINT('',#59951);
#19305=VERTEX_POINT('',#59953);
#19306=VERTEX_POINT('',#59955);
#19307=VERTEX_POINT('',#59957);
#19308=VERTEX_POINT('',#59960);
#19309=VERTEX_POINT('',#59961);
#19310=VERTEX_POINT('',#59963);
#19311=VERTEX_POINT('',#59965);
#19312=VERTEX_POINT('',#59967);
#19313=VERTEX_POINT('',#59969);
#19314=VERTEX_POINT('',#59972);
#19315=VERTEX_POINT('',#59973);
#19316=VERTEX_POINT('',#59975);
#19317=VERTEX_POINT('',#59977);
#19318=VERTEX_POINT('',#59979);
#19319=VERTEX_POINT('',#59981);
#19320=VERTEX_POINT('',#59984);
#19321=VERTEX_POINT('',#59985);
#19322=VERTEX_POINT('',#59987);
#19323=VERTEX_POINT('',#59989);
#19324=VERTEX_POINT('',#59991);
#19325=VERTEX_POINT('',#59993);
#19326=VERTEX_POINT('',#59996);
#19327=VERTEX_POINT('',#59997);
#19328=VERTEX_POINT('',#59999);
#19329=VERTEX_POINT('',#60001);
#19330=VERTEX_POINT('',#60003);
#19331=VERTEX_POINT('',#60005);
#19332=VERTEX_POINT('',#60008);
#19333=VERTEX_POINT('',#60009);
#19334=VERTEX_POINT('',#60011);
#19335=VERTEX_POINT('',#60013);
#19336=VERTEX_POINT('',#60015);
#19337=VERTEX_POINT('',#60017);
#19338=VERTEX_POINT('',#60020);
#19339=VERTEX_POINT('',#60021);
#19340=VERTEX_POINT('',#60023);
#19341=VERTEX_POINT('',#60025);
#19342=VERTEX_POINT('',#60027);
#19343=VERTEX_POINT('',#60029);
#19344=VERTEX_POINT('',#60032);
#19345=VERTEX_POINT('',#60033);
#19346=VERTEX_POINT('',#60035);
#19347=VERTEX_POINT('',#60037);
#19348=VERTEX_POINT('',#60039);
#19349=VERTEX_POINT('',#60041);
#19350=VERTEX_POINT('',#60044);
#19351=VERTEX_POINT('',#60045);
#19352=VERTEX_POINT('',#60047);
#19353=VERTEX_POINT('',#60049);
#19354=VERTEX_POINT('',#60051);
#19355=VERTEX_POINT('',#60053);
#19356=VERTEX_POINT('',#60056);
#19357=VERTEX_POINT('',#60057);
#19358=VERTEX_POINT('',#60059);
#19359=VERTEX_POINT('',#60061);
#19360=VERTEX_POINT('',#60063);
#19361=VERTEX_POINT('',#60065);
#19362=VERTEX_POINT('',#60068);
#19363=VERTEX_POINT('',#60069);
#19364=VERTEX_POINT('',#60071);
#19365=VERTEX_POINT('',#60073);
#19366=VERTEX_POINT('',#60075);
#19367=VERTEX_POINT('',#60077);
#19368=VERTEX_POINT('',#60080);
#19369=VERTEX_POINT('',#60081);
#19370=VERTEX_POINT('',#60083);
#19371=VERTEX_POINT('',#60085);
#19372=VERTEX_POINT('',#60087);
#19373=VERTEX_POINT('',#60089);
#19374=VERTEX_POINT('',#60092);
#19375=VERTEX_POINT('',#60093);
#19376=VERTEX_POINT('',#60095);
#19377=VERTEX_POINT('',#60097);
#19378=VERTEX_POINT('',#60099);
#19379=VERTEX_POINT('',#60101);
#19380=VERTEX_POINT('',#60104);
#19381=VERTEX_POINT('',#60105);
#19382=VERTEX_POINT('',#60107);
#19383=VERTEX_POINT('',#60109);
#19384=VERTEX_POINT('',#60111);
#19385=VERTEX_POINT('',#60113);
#19386=VERTEX_POINT('',#60116);
#19387=VERTEX_POINT('',#60117);
#19388=VERTEX_POINT('',#60119);
#19389=VERTEX_POINT('',#60121);
#19390=VERTEX_POINT('',#60123);
#19391=VERTEX_POINT('',#60125);
#19392=VERTEX_POINT('',#60128);
#19393=VERTEX_POINT('',#60129);
#19394=VERTEX_POINT('',#60131);
#19395=VERTEX_POINT('',#60133);
#19396=VERTEX_POINT('',#60135);
#19397=VERTEX_POINT('',#60137);
#19398=VERTEX_POINT('',#60140);
#19399=VERTEX_POINT('',#60141);
#19400=VERTEX_POINT('',#60143);
#19401=VERTEX_POINT('',#60145);
#19402=VERTEX_POINT('',#60147);
#19403=VERTEX_POINT('',#60149);
#19404=VERTEX_POINT('',#60152);
#19405=VERTEX_POINT('',#60153);
#19406=VERTEX_POINT('',#60155);
#19407=VERTEX_POINT('',#60157);
#19408=VERTEX_POINT('',#60159);
#19409=VERTEX_POINT('',#60161);
#19410=VERTEX_POINT('',#60164);
#19411=VERTEX_POINT('',#60165);
#19412=VERTEX_POINT('',#60167);
#19413=VERTEX_POINT('',#60169);
#19414=VERTEX_POINT('',#60171);
#19415=VERTEX_POINT('',#60173);
#19416=VERTEX_POINT('',#60176);
#19417=VERTEX_POINT('',#60177);
#19418=VERTEX_POINT('',#60179);
#19419=VERTEX_POINT('',#60181);
#19420=VERTEX_POINT('',#60183);
#19421=VERTEX_POINT('',#60185);
#19422=VERTEX_POINT('',#60188);
#19423=VERTEX_POINT('',#60189);
#19424=VERTEX_POINT('',#60191);
#19425=VERTEX_POINT('',#60193);
#19426=VERTEX_POINT('',#60195);
#19427=VERTEX_POINT('',#60197);
#19428=VERTEX_POINT('',#60200);
#19429=VERTEX_POINT('',#60201);
#19430=VERTEX_POINT('',#60203);
#19431=VERTEX_POINT('',#60205);
#19432=VERTEX_POINT('',#60207);
#19433=VERTEX_POINT('',#60209);
#19434=VERTEX_POINT('',#60212);
#19435=VERTEX_POINT('',#60213);
#19436=VERTEX_POINT('',#60215);
#19437=VERTEX_POINT('',#60217);
#19438=VERTEX_POINT('',#60219);
#19439=VERTEX_POINT('',#60221);
#19440=VERTEX_POINT('',#60224);
#19441=VERTEX_POINT('',#60225);
#19442=VERTEX_POINT('',#60227);
#19443=VERTEX_POINT('',#60229);
#19444=VERTEX_POINT('',#60231);
#19445=VERTEX_POINT('',#60233);
#19446=VERTEX_POINT('',#60236);
#19447=VERTEX_POINT('',#60237);
#19448=VERTEX_POINT('',#60239);
#19449=VERTEX_POINT('',#60241);
#19450=VERTEX_POINT('',#60243);
#19451=VERTEX_POINT('',#60245);
#19452=VERTEX_POINT('',#60248);
#19453=VERTEX_POINT('',#60249);
#19454=VERTEX_POINT('',#60251);
#19455=VERTEX_POINT('',#60253);
#19456=VERTEX_POINT('',#60255);
#19457=VERTEX_POINT('',#60257);
#19458=VERTEX_POINT('',#60260);
#19459=VERTEX_POINT('',#60261);
#19460=VERTEX_POINT('',#60263);
#19461=VERTEX_POINT('',#60265);
#19462=VERTEX_POINT('',#60267);
#19463=VERTEX_POINT('',#60269);
#19464=VERTEX_POINT('',#60272);
#19465=VERTEX_POINT('',#60273);
#19466=VERTEX_POINT('',#60275);
#19467=VERTEX_POINT('',#60277);
#19468=VERTEX_POINT('',#60279);
#19469=VERTEX_POINT('',#60281);
#19470=VERTEX_POINT('',#60284);
#19471=VERTEX_POINT('',#60285);
#19472=VERTEX_POINT('',#60287);
#19473=VERTEX_POINT('',#60289);
#19474=VERTEX_POINT('',#60291);
#19475=VERTEX_POINT('',#60293);
#19476=VERTEX_POINT('',#60296);
#19477=VERTEX_POINT('',#60297);
#19478=VERTEX_POINT('',#60299);
#19479=VERTEX_POINT('',#60301);
#19480=VERTEX_POINT('',#60303);
#19481=VERTEX_POINT('',#60305);
#19482=VERTEX_POINT('',#60308);
#19483=VERTEX_POINT('',#60309);
#19484=VERTEX_POINT('',#60311);
#19485=VERTEX_POINT('',#60313);
#19486=VERTEX_POINT('',#60315);
#19487=VERTEX_POINT('',#60317);
#19488=VERTEX_POINT('',#60320);
#19489=VERTEX_POINT('',#60321);
#19490=VERTEX_POINT('',#60323);
#19491=VERTEX_POINT('',#60325);
#19492=VERTEX_POINT('',#60327);
#19493=VERTEX_POINT('',#60329);
#19494=VERTEX_POINT('',#60332);
#19495=VERTEX_POINT('',#60333);
#19496=VERTEX_POINT('',#60335);
#19497=VERTEX_POINT('',#60337);
#19498=VERTEX_POINT('',#60339);
#19499=VERTEX_POINT('',#60341);
#19500=VERTEX_POINT('',#60344);
#19501=VERTEX_POINT('',#60345);
#19502=VERTEX_POINT('',#60347);
#19503=VERTEX_POINT('',#60349);
#19504=VERTEX_POINT('',#60351);
#19505=VERTEX_POINT('',#60353);
#19506=VERTEX_POINT('',#60356);
#19507=VERTEX_POINT('',#60357);
#19508=VERTEX_POINT('',#60359);
#19509=VERTEX_POINT('',#60361);
#19510=VERTEX_POINT('',#60363);
#19511=VERTEX_POINT('',#60365);
#19512=VERTEX_POINT('',#60368);
#19513=VERTEX_POINT('',#60369);
#19514=VERTEX_POINT('',#60371);
#19515=VERTEX_POINT('',#60373);
#19516=VERTEX_POINT('',#60375);
#19517=VERTEX_POINT('',#60377);
#19518=VERTEX_POINT('',#60380);
#19519=VERTEX_POINT('',#60381);
#19520=VERTEX_POINT('',#60383);
#19521=VERTEX_POINT('',#60385);
#19522=VERTEX_POINT('',#60387);
#19523=VERTEX_POINT('',#60389);
#19524=VERTEX_POINT('',#60392);
#19525=VERTEX_POINT('',#60393);
#19526=VERTEX_POINT('',#60395);
#19527=VERTEX_POINT('',#60397);
#19528=VERTEX_POINT('',#60399);
#19529=VERTEX_POINT('',#60401);
#19530=VERTEX_POINT('',#60404);
#19531=VERTEX_POINT('',#60405);
#19532=VERTEX_POINT('',#60407);
#19533=VERTEX_POINT('',#60409);
#19534=VERTEX_POINT('',#60411);
#19535=VERTEX_POINT('',#60413);
#19536=VERTEX_POINT('',#60416);
#19537=VERTEX_POINT('',#60417);
#19538=VERTEX_POINT('',#60419);
#19539=VERTEX_POINT('',#60421);
#19540=VERTEX_POINT('',#60423);
#19541=VERTEX_POINT('',#60425);
#19542=VERTEX_POINT('',#60428);
#19543=VERTEX_POINT('',#60429);
#19544=VERTEX_POINT('',#60431);
#19545=VERTEX_POINT('',#60433);
#19546=VERTEX_POINT('',#60435);
#19547=VERTEX_POINT('',#60437);
#19548=VERTEX_POINT('',#60440);
#19549=VERTEX_POINT('',#60441);
#19550=VERTEX_POINT('',#60443);
#19551=VERTEX_POINT('',#60445);
#19552=VERTEX_POINT('',#60447);
#19553=VERTEX_POINT('',#60449);
#19554=VERTEX_POINT('',#60452);
#19555=VERTEX_POINT('',#60453);
#19556=VERTEX_POINT('',#60455);
#19557=VERTEX_POINT('',#60457);
#19558=VERTEX_POINT('',#60459);
#19559=VERTEX_POINT('',#60461);
#19560=VERTEX_POINT('',#60464);
#19561=VERTEX_POINT('',#60465);
#19562=VERTEX_POINT('',#60467);
#19563=VERTEX_POINT('',#60469);
#19564=VERTEX_POINT('',#60471);
#19565=VERTEX_POINT('',#60473);
#19566=VERTEX_POINT('',#60476);
#19567=VERTEX_POINT('',#60477);
#19568=VERTEX_POINT('',#60479);
#19569=VERTEX_POINT('',#60481);
#19570=VERTEX_POINT('',#60483);
#19571=VERTEX_POINT('',#60485);
#19572=VERTEX_POINT('',#60488);
#19573=VERTEX_POINT('',#60489);
#19574=VERTEX_POINT('',#60491);
#19575=VERTEX_POINT('',#60493);
#19576=VERTEX_POINT('',#60495);
#19577=VERTEX_POINT('',#60497);
#19578=VERTEX_POINT('',#60500);
#19579=VERTEX_POINT('',#60501);
#19580=VERTEX_POINT('',#60503);
#19581=VERTEX_POINT('',#60505);
#19582=VERTEX_POINT('',#60507);
#19583=VERTEX_POINT('',#60509);
#19584=VERTEX_POINT('',#60512);
#19585=VERTEX_POINT('',#60513);
#19586=VERTEX_POINT('',#60515);
#19587=VERTEX_POINT('',#60517);
#19588=VERTEX_POINT('',#60519);
#19589=VERTEX_POINT('',#60521);
#19590=VERTEX_POINT('',#60524);
#19591=VERTEX_POINT('',#60525);
#19592=VERTEX_POINT('',#60527);
#19593=VERTEX_POINT('',#60529);
#19594=VERTEX_POINT('',#60531);
#19595=VERTEX_POINT('',#60533);
#19596=VERTEX_POINT('',#60536);
#19597=VERTEX_POINT('',#60537);
#19598=VERTEX_POINT('',#60539);
#19599=VERTEX_POINT('',#60541);
#19600=VERTEX_POINT('',#60543);
#19601=VERTEX_POINT('',#60545);
#19602=VERTEX_POINT('',#60548);
#19603=VERTEX_POINT('',#60549);
#19604=VERTEX_POINT('',#60551);
#19605=VERTEX_POINT('',#60553);
#19606=VERTEX_POINT('',#60555);
#19607=VERTEX_POINT('',#60557);
#19608=VERTEX_POINT('',#60560);
#19609=VERTEX_POINT('',#60561);
#19610=VERTEX_POINT('',#60563);
#19611=VERTEX_POINT('',#60565);
#19612=VERTEX_POINT('',#60567);
#19613=VERTEX_POINT('',#60569);
#19614=VERTEX_POINT('',#60572);
#19615=VERTEX_POINT('',#60573);
#19616=VERTEX_POINT('',#60575);
#19617=VERTEX_POINT('',#60577);
#19618=VERTEX_POINT('',#60579);
#19619=VERTEX_POINT('',#60581);
#19620=VERTEX_POINT('',#60584);
#19621=VERTEX_POINT('',#60585);
#19622=VERTEX_POINT('',#60587);
#19623=VERTEX_POINT('',#60589);
#19624=VERTEX_POINT('',#60591);
#19625=VERTEX_POINT('',#60593);
#19626=VERTEX_POINT('',#60596);
#19627=VERTEX_POINT('',#60597);
#19628=VERTEX_POINT('',#60599);
#19629=VERTEX_POINT('',#60601);
#19630=VERTEX_POINT('',#60603);
#19631=VERTEX_POINT('',#60605);
#19632=VERTEX_POINT('',#60608);
#19633=VERTEX_POINT('',#60609);
#19634=VERTEX_POINT('',#60611);
#19635=VERTEX_POINT('',#60613);
#19636=VERTEX_POINT('',#60615);
#19637=VERTEX_POINT('',#60617);
#19638=VERTEX_POINT('',#60620);
#19639=VERTEX_POINT('',#60621);
#19640=VERTEX_POINT('',#60623);
#19641=VERTEX_POINT('',#60625);
#19642=VERTEX_POINT('',#60627);
#19643=VERTEX_POINT('',#60629);
#19644=VERTEX_POINT('',#60632);
#19645=VERTEX_POINT('',#60633);
#19646=VERTEX_POINT('',#60635);
#19647=VERTEX_POINT('',#60637);
#19648=VERTEX_POINT('',#60639);
#19649=VERTEX_POINT('',#60641);
#19650=VERTEX_POINT('',#60644);
#19651=VERTEX_POINT('',#60645);
#19652=VERTEX_POINT('',#60647);
#19653=VERTEX_POINT('',#60649);
#19654=VERTEX_POINT('',#60651);
#19655=VERTEX_POINT('',#60653);
#19656=VERTEX_POINT('',#60656);
#19657=VERTEX_POINT('',#60657);
#19658=VERTEX_POINT('',#60659);
#19659=VERTEX_POINT('',#60661);
#19660=VERTEX_POINT('',#60663);
#19661=VERTEX_POINT('',#60665);
#19662=VERTEX_POINT('',#60668);
#19663=VERTEX_POINT('',#60669);
#19664=VERTEX_POINT('',#60671);
#19665=VERTEX_POINT('',#60673);
#19666=VERTEX_POINT('',#60675);
#19667=VERTEX_POINT('',#60677);
#19668=VERTEX_POINT('',#60680);
#19669=VERTEX_POINT('',#60681);
#19670=VERTEX_POINT('',#60683);
#19671=VERTEX_POINT('',#60685);
#19672=VERTEX_POINT('',#60687);
#19673=VERTEX_POINT('',#60689);
#19674=VERTEX_POINT('',#60692);
#19675=VERTEX_POINT('',#60693);
#19676=VERTEX_POINT('',#60695);
#19677=VERTEX_POINT('',#60697);
#19678=VERTEX_POINT('',#60699);
#19679=VERTEX_POINT('',#60701);
#19680=VERTEX_POINT('',#60704);
#19681=VERTEX_POINT('',#60705);
#19682=VERTEX_POINT('',#60707);
#19683=VERTEX_POINT('',#60709);
#19684=VERTEX_POINT('',#60711);
#19685=VERTEX_POINT('',#60713);
#19686=VERTEX_POINT('',#60716);
#19687=VERTEX_POINT('',#60717);
#19688=VERTEX_POINT('',#60719);
#19689=VERTEX_POINT('',#60721);
#19690=VERTEX_POINT('',#60723);
#19691=VERTEX_POINT('',#60725);
#19692=VERTEX_POINT('',#60728);
#19693=VERTEX_POINT('',#60729);
#19694=VERTEX_POINT('',#60731);
#19695=VERTEX_POINT('',#60733);
#19696=VERTEX_POINT('',#60735);
#19697=VERTEX_POINT('',#60737);
#19698=VERTEX_POINT('',#60740);
#19699=VERTEX_POINT('',#60741);
#19700=VERTEX_POINT('',#60743);
#19701=VERTEX_POINT('',#60745);
#19702=VERTEX_POINT('',#60747);
#19703=VERTEX_POINT('',#60749);
#19704=VERTEX_POINT('',#60752);
#19705=VERTEX_POINT('',#60753);
#19706=VERTEX_POINT('',#60755);
#19707=VERTEX_POINT('',#60757);
#19708=VERTEX_POINT('',#60759);
#19709=VERTEX_POINT('',#60761);
#19710=VERTEX_POINT('',#60764);
#19711=VERTEX_POINT('',#60765);
#19712=VERTEX_POINT('',#60767);
#19713=VERTEX_POINT('',#60769);
#19714=VERTEX_POINT('',#60771);
#19715=VERTEX_POINT('',#60773);
#19716=VERTEX_POINT('',#60776);
#19717=VERTEX_POINT('',#60777);
#19718=VERTEX_POINT('',#60779);
#19719=VERTEX_POINT('',#60781);
#19720=VERTEX_POINT('',#60783);
#19721=VERTEX_POINT('',#60785);
#19722=VERTEX_POINT('',#60788);
#19723=VERTEX_POINT('',#60789);
#19724=VERTEX_POINT('',#60791);
#19725=VERTEX_POINT('',#60793);
#19726=VERTEX_POINT('',#60795);
#19727=VERTEX_POINT('',#60797);
#19728=VERTEX_POINT('',#60800);
#19729=VERTEX_POINT('',#60801);
#19730=VERTEX_POINT('',#60803);
#19731=VERTEX_POINT('',#60805);
#19732=VERTEX_POINT('',#60807);
#19733=VERTEX_POINT('',#60809);
#19734=VERTEX_POINT('',#60812);
#19735=VERTEX_POINT('',#60813);
#19736=VERTEX_POINT('',#60815);
#19737=VERTEX_POINT('',#60817);
#19738=VERTEX_POINT('',#60819);
#19739=VERTEX_POINT('',#60821);
#19740=VERTEX_POINT('',#60825);
#19741=VERTEX_POINT('',#60826);
#19742=VERTEX_POINT('',#60828);
#19743=VERTEX_POINT('',#60830);
#19744=VERTEX_POINT('',#60832);
#19745=VERTEX_POINT('',#60834);
#19746=VERTEX_POINT('',#60837);
#19747=VERTEX_POINT('',#60838);
#19748=VERTEX_POINT('',#60840);
#19749=VERTEX_POINT('',#60842);
#19750=VERTEX_POINT('',#60844);
#19751=VERTEX_POINT('',#60846);
#19752=VERTEX_POINT('',#60849);
#19753=VERTEX_POINT('',#60850);
#19754=VERTEX_POINT('',#60852);
#19755=VERTEX_POINT('',#60854);
#19756=VERTEX_POINT('',#60856);
#19757=VERTEX_POINT('',#60858);
#19758=VERTEX_POINT('',#60861);
#19759=VERTEX_POINT('',#60862);
#19760=VERTEX_POINT('',#60864);
#19761=VERTEX_POINT('',#60866);
#19762=VERTEX_POINT('',#60868);
#19763=VERTEX_POINT('',#60870);
#19764=VERTEX_POINT('',#60873);
#19765=VERTEX_POINT('',#60874);
#19766=VERTEX_POINT('',#60876);
#19767=VERTEX_POINT('',#60878);
#19768=VERTEX_POINT('',#60880);
#19769=VERTEX_POINT('',#60882);
#19770=VERTEX_POINT('',#60885);
#19771=VERTEX_POINT('',#60886);
#19772=VERTEX_POINT('',#60888);
#19773=VERTEX_POINT('',#60890);
#19774=VERTEX_POINT('',#60892);
#19775=VERTEX_POINT('',#60894);
#19776=VERTEX_POINT('',#60897);
#19777=VERTEX_POINT('',#60898);
#19778=VERTEX_POINT('',#60900);
#19779=VERTEX_POINT('',#60902);
#19780=VERTEX_POINT('',#60904);
#19781=VERTEX_POINT('',#60906);
#19782=VERTEX_POINT('',#60909);
#19783=VERTEX_POINT('',#60910);
#19784=VERTEX_POINT('',#60912);
#19785=VERTEX_POINT('',#60914);
#19786=VERTEX_POINT('',#60916);
#19787=VERTEX_POINT('',#60918);
#19788=VERTEX_POINT('',#60921);
#19789=VERTEX_POINT('',#60922);
#19790=VERTEX_POINT('',#60924);
#19791=VERTEX_POINT('',#60926);
#19792=VERTEX_POINT('',#60928);
#19793=VERTEX_POINT('',#60930);
#19794=VERTEX_POINT('',#60933);
#19795=VERTEX_POINT('',#60934);
#19796=VERTEX_POINT('',#60936);
#19797=VERTEX_POINT('',#60938);
#19798=VERTEX_POINT('',#60940);
#19799=VERTEX_POINT('',#60942);
#19800=VERTEX_POINT('',#60945);
#19801=VERTEX_POINT('',#60946);
#19802=VERTEX_POINT('',#60948);
#19803=VERTEX_POINT('',#60950);
#19804=VERTEX_POINT('',#60952);
#19805=VERTEX_POINT('',#60954);
#19806=VERTEX_POINT('',#60957);
#19807=VERTEX_POINT('',#60958);
#19808=VERTEX_POINT('',#60960);
#19809=VERTEX_POINT('',#60962);
#19810=VERTEX_POINT('',#60964);
#19811=VERTEX_POINT('',#60966);
#19812=VERTEX_POINT('',#60969);
#19813=VERTEX_POINT('',#60970);
#19814=VERTEX_POINT('',#60972);
#19815=VERTEX_POINT('',#60974);
#19816=VERTEX_POINT('',#60976);
#19817=VERTEX_POINT('',#60978);
#19818=VERTEX_POINT('',#60981);
#19819=VERTEX_POINT('',#60982);
#19820=VERTEX_POINT('',#60984);
#19821=VERTEX_POINT('',#60986);
#19822=VERTEX_POINT('',#60988);
#19823=VERTEX_POINT('',#60990);
#19824=VERTEX_POINT('',#60993);
#19825=VERTEX_POINT('',#60994);
#19826=VERTEX_POINT('',#60996);
#19827=VERTEX_POINT('',#60998);
#19828=VERTEX_POINT('',#61000);
#19829=VERTEX_POINT('',#61002);
#19830=VERTEX_POINT('',#61005);
#19831=VERTEX_POINT('',#61006);
#19832=VERTEX_POINT('',#61008);
#19833=VERTEX_POINT('',#61010);
#19834=VERTEX_POINT('',#61012);
#19835=VERTEX_POINT('',#61014);
#19836=VERTEX_POINT('',#61017);
#19837=VERTEX_POINT('',#61018);
#19838=VERTEX_POINT('',#61020);
#19839=VERTEX_POINT('',#61022);
#19840=VERTEX_POINT('',#61024);
#19841=VERTEX_POINT('',#61026);
#19842=VERTEX_POINT('',#61029);
#19843=VERTEX_POINT('',#61030);
#19844=VERTEX_POINT('',#61032);
#19845=VERTEX_POINT('',#61034);
#19846=VERTEX_POINT('',#61036);
#19847=VERTEX_POINT('',#61038);
#19848=VERTEX_POINT('',#61041);
#19849=VERTEX_POINT('',#61042);
#19850=VERTEX_POINT('',#61044);
#19851=VERTEX_POINT('',#61046);
#19852=VERTEX_POINT('',#61048);
#19853=VERTEX_POINT('',#61050);
#19854=VERTEX_POINT('',#61053);
#19855=VERTEX_POINT('',#61054);
#19856=VERTEX_POINT('',#61056);
#19857=VERTEX_POINT('',#61058);
#19858=VERTEX_POINT('',#61060);
#19859=VERTEX_POINT('',#61062);
#19860=VERTEX_POINT('',#61065);
#19861=VERTEX_POINT('',#61066);
#19862=VERTEX_POINT('',#61068);
#19863=VERTEX_POINT('',#61070);
#19864=VERTEX_POINT('',#61072);
#19865=VERTEX_POINT('',#61074);
#19866=VERTEX_POINT('',#61077);
#19867=VERTEX_POINT('',#61078);
#19868=VERTEX_POINT('',#61080);
#19869=VERTEX_POINT('',#61082);
#19870=VERTEX_POINT('',#61084);
#19871=VERTEX_POINT('',#61086);
#19872=VERTEX_POINT('',#61089);
#19873=VERTEX_POINT('',#61090);
#19874=VERTEX_POINT('',#61092);
#19875=VERTEX_POINT('',#61094);
#19876=VERTEX_POINT('',#61096);
#19877=VERTEX_POINT('',#61098);
#19878=VERTEX_POINT('',#61101);
#19879=VERTEX_POINT('',#61102);
#19880=VERTEX_POINT('',#61104);
#19881=VERTEX_POINT('',#61106);
#19882=VERTEX_POINT('',#61108);
#19883=VERTEX_POINT('',#61110);
#19884=VERTEX_POINT('',#61113);
#19885=VERTEX_POINT('',#61114);
#19886=VERTEX_POINT('',#61116);
#19887=VERTEX_POINT('',#61118);
#19888=VERTEX_POINT('',#61120);
#19889=VERTEX_POINT('',#61122);
#19890=VERTEX_POINT('',#61125);
#19891=VERTEX_POINT('',#61126);
#19892=VERTEX_POINT('',#61128);
#19893=VERTEX_POINT('',#61130);
#19894=VERTEX_POINT('',#61132);
#19895=VERTEX_POINT('',#61134);
#19896=VERTEX_POINT('',#61137);
#19897=VERTEX_POINT('',#61138);
#19898=VERTEX_POINT('',#61140);
#19899=VERTEX_POINT('',#61142);
#19900=VERTEX_POINT('',#61144);
#19901=VERTEX_POINT('',#61146);
#19902=VERTEX_POINT('',#61149);
#19903=VERTEX_POINT('',#61150);
#19904=VERTEX_POINT('',#61152);
#19905=VERTEX_POINT('',#61154);
#19906=VERTEX_POINT('',#61156);
#19907=VERTEX_POINT('',#61158);
#19908=VERTEX_POINT('',#61161);
#19909=VERTEX_POINT('',#61162);
#19910=VERTEX_POINT('',#61164);
#19911=VERTEX_POINT('',#61166);
#19912=VERTEX_POINT('',#61168);
#19913=VERTEX_POINT('',#61170);
#19914=VERTEX_POINT('',#61173);
#19915=VERTEX_POINT('',#61174);
#19916=VERTEX_POINT('',#61176);
#19917=VERTEX_POINT('',#61178);
#19918=VERTEX_POINT('',#61180);
#19919=VERTEX_POINT('',#61182);
#19920=VERTEX_POINT('',#61185);
#19921=VERTEX_POINT('',#61186);
#19922=VERTEX_POINT('',#61188);
#19923=VERTEX_POINT('',#61190);
#19924=VERTEX_POINT('',#61192);
#19925=VERTEX_POINT('',#61194);
#19926=VERTEX_POINT('',#61197);
#19927=VERTEX_POINT('',#61198);
#19928=VERTEX_POINT('',#61200);
#19929=VERTEX_POINT('',#61202);
#19930=VERTEX_POINT('',#61204);
#19931=VERTEX_POINT('',#61206);
#19932=VERTEX_POINT('',#61209);
#19933=VERTEX_POINT('',#61210);
#19934=VERTEX_POINT('',#61212);
#19935=VERTEX_POINT('',#61214);
#19936=VERTEX_POINT('',#61216);
#19937=VERTEX_POINT('',#61218);
#19938=VERTEX_POINT('',#61221);
#19939=VERTEX_POINT('',#61222);
#19940=VERTEX_POINT('',#61224);
#19941=VERTEX_POINT('',#61226);
#19942=VERTEX_POINT('',#61228);
#19943=VERTEX_POINT('',#61230);
#19944=VERTEX_POINT('',#61233);
#19945=VERTEX_POINT('',#61234);
#19946=VERTEX_POINT('',#61236);
#19947=VERTEX_POINT('',#61238);
#19948=VERTEX_POINT('',#61240);
#19949=VERTEX_POINT('',#61242);
#19950=VERTEX_POINT('',#61245);
#19951=VERTEX_POINT('',#61246);
#19952=VERTEX_POINT('',#61248);
#19953=VERTEX_POINT('',#61250);
#19954=VERTEX_POINT('',#61252);
#19955=VERTEX_POINT('',#61254);
#19956=VERTEX_POINT('',#61257);
#19957=VERTEX_POINT('',#61258);
#19958=VERTEX_POINT('',#61260);
#19959=VERTEX_POINT('',#61262);
#19960=VERTEX_POINT('',#61264);
#19961=VERTEX_POINT('',#61266);
#19962=VERTEX_POINT('',#61269);
#19963=VERTEX_POINT('',#61270);
#19964=VERTEX_POINT('',#61272);
#19965=VERTEX_POINT('',#61274);
#19966=VERTEX_POINT('',#61276);
#19967=VERTEX_POINT('',#61278);
#19968=VERTEX_POINT('',#61281);
#19969=VERTEX_POINT('',#61282);
#19970=VERTEX_POINT('',#61284);
#19971=VERTEX_POINT('',#61286);
#19972=VERTEX_POINT('',#61288);
#19973=VERTEX_POINT('',#61290);
#19974=VERTEX_POINT('',#61293);
#19975=VERTEX_POINT('',#61294);
#19976=VERTEX_POINT('',#61296);
#19977=VERTEX_POINT('',#61298);
#19978=VERTEX_POINT('',#61300);
#19979=VERTEX_POINT('',#61302);
#19980=VERTEX_POINT('',#61305);
#19981=VERTEX_POINT('',#61306);
#19982=VERTEX_POINT('',#61308);
#19983=VERTEX_POINT('',#61310);
#19984=VERTEX_POINT('',#61312);
#19985=VERTEX_POINT('',#61314);
#19986=VERTEX_POINT('',#61317);
#19987=VERTEX_POINT('',#61318);
#19988=VERTEX_POINT('',#61320);
#19989=VERTEX_POINT('',#61322);
#19990=VERTEX_POINT('',#61324);
#19991=VERTEX_POINT('',#61326);
#19992=VERTEX_POINT('',#61329);
#19993=VERTEX_POINT('',#61330);
#19994=VERTEX_POINT('',#61332);
#19995=VERTEX_POINT('',#61334);
#19996=VERTEX_POINT('',#61336);
#19997=VERTEX_POINT('',#61338);
#19998=VERTEX_POINT('',#61341);
#19999=VERTEX_POINT('',#61342);
#20000=VERTEX_POINT('',#61344);
#20001=VERTEX_POINT('',#61346);
#20002=VERTEX_POINT('',#61348);
#20003=VERTEX_POINT('',#61350);
#20004=VERTEX_POINT('',#61353);
#20005=VERTEX_POINT('',#61354);
#20006=VERTEX_POINT('',#61356);
#20007=VERTEX_POINT('',#61358);
#20008=VERTEX_POINT('',#61360);
#20009=VERTEX_POINT('',#61362);
#20010=VERTEX_POINT('',#61365);
#20011=VERTEX_POINT('',#61366);
#20012=VERTEX_POINT('',#61368);
#20013=VERTEX_POINT('',#61370);
#20014=VERTEX_POINT('',#61372);
#20015=VERTEX_POINT('',#61374);
#20016=VERTEX_POINT('',#61377);
#20017=VERTEX_POINT('',#61378);
#20018=VERTEX_POINT('',#61380);
#20019=VERTEX_POINT('',#61382);
#20020=VERTEX_POINT('',#61384);
#20021=VERTEX_POINT('',#61386);
#20022=VERTEX_POINT('',#61389);
#20023=VERTEX_POINT('',#61390);
#20024=VERTEX_POINT('',#61392);
#20025=VERTEX_POINT('',#61394);
#20026=VERTEX_POINT('',#61396);
#20027=VERTEX_POINT('',#61398);
#20028=VERTEX_POINT('',#61401);
#20029=VERTEX_POINT('',#61402);
#20030=VERTEX_POINT('',#61404);
#20031=VERTEX_POINT('',#61406);
#20032=VERTEX_POINT('',#61408);
#20033=VERTEX_POINT('',#61410);
#20034=VERTEX_POINT('',#61413);
#20035=VERTEX_POINT('',#61414);
#20036=VERTEX_POINT('',#61416);
#20037=VERTEX_POINT('',#61418);
#20038=VERTEX_POINT('',#61420);
#20039=VERTEX_POINT('',#61422);
#20040=VERTEX_POINT('',#61425);
#20041=VERTEX_POINT('',#61426);
#20042=VERTEX_POINT('',#61428);
#20043=VERTEX_POINT('',#61430);
#20044=VERTEX_POINT('',#61432);
#20045=VERTEX_POINT('',#61434);
#20046=VERTEX_POINT('',#61437);
#20047=VERTEX_POINT('',#61438);
#20048=VERTEX_POINT('',#61440);
#20049=VERTEX_POINT('',#61442);
#20050=VERTEX_POINT('',#61444);
#20051=VERTEX_POINT('',#61446);
#20052=VERTEX_POINT('',#61449);
#20053=VERTEX_POINT('',#61450);
#20054=VERTEX_POINT('',#61452);
#20055=VERTEX_POINT('',#61454);
#20056=VERTEX_POINT('',#61456);
#20057=VERTEX_POINT('',#61458);
#20058=VERTEX_POINT('',#61461);
#20059=VERTEX_POINT('',#61462);
#20060=VERTEX_POINT('',#61464);
#20061=VERTEX_POINT('',#61466);
#20062=VERTEX_POINT('',#61468);
#20063=VERTEX_POINT('',#61470);
#20064=VERTEX_POINT('',#61473);
#20065=VERTEX_POINT('',#61474);
#20066=VERTEX_POINT('',#61476);
#20067=VERTEX_POINT('',#61478);
#20068=VERTEX_POINT('',#61480);
#20069=VERTEX_POINT('',#61482);
#20070=VERTEX_POINT('',#61485);
#20071=VERTEX_POINT('',#61486);
#20072=VERTEX_POINT('',#61488);
#20073=VERTEX_POINT('',#61490);
#20074=VERTEX_POINT('',#61492);
#20075=VERTEX_POINT('',#61494);
#20076=VERTEX_POINT('',#61497);
#20077=VERTEX_POINT('',#61498);
#20078=VERTEX_POINT('',#61500);
#20079=VERTEX_POINT('',#61502);
#20080=VERTEX_POINT('',#61504);
#20081=VERTEX_POINT('',#61506);
#20082=VERTEX_POINT('',#61509);
#20083=VERTEX_POINT('',#61510);
#20084=VERTEX_POINT('',#61512);
#20085=VERTEX_POINT('',#61514);
#20086=VERTEX_POINT('',#61516);
#20087=VERTEX_POINT('',#61518);
#20088=VERTEX_POINT('',#61521);
#20089=VERTEX_POINT('',#61522);
#20090=VERTEX_POINT('',#61524);
#20091=VERTEX_POINT('',#61526);
#20092=VERTEX_POINT('',#61528);
#20093=VERTEX_POINT('',#61530);
#20094=VERTEX_POINT('',#61533);
#20095=VERTEX_POINT('',#61534);
#20096=VERTEX_POINT('',#61536);
#20097=VERTEX_POINT('',#61538);
#20098=VERTEX_POINT('',#61540);
#20099=VERTEX_POINT('',#61542);
#20100=VERTEX_POINT('',#61545);
#20101=VERTEX_POINT('',#61546);
#20102=VERTEX_POINT('',#61548);
#20103=VERTEX_POINT('',#61550);
#20104=VERTEX_POINT('',#61552);
#20105=VERTEX_POINT('',#61554);
#20106=VERTEX_POINT('',#61557);
#20107=VERTEX_POINT('',#61558);
#20108=VERTEX_POINT('',#61560);
#20109=VERTEX_POINT('',#61562);
#20110=VERTEX_POINT('',#61564);
#20111=VERTEX_POINT('',#61566);
#20112=VERTEX_POINT('',#61569);
#20113=VERTEX_POINT('',#61570);
#20114=VERTEX_POINT('',#61572);
#20115=VERTEX_POINT('',#61574);
#20116=VERTEX_POINT('',#61576);
#20117=VERTEX_POINT('',#61578);
#20118=VERTEX_POINT('',#61581);
#20119=VERTEX_POINT('',#61582);
#20120=VERTEX_POINT('',#61584);
#20121=VERTEX_POINT('',#61586);
#20122=VERTEX_POINT('',#61588);
#20123=VERTEX_POINT('',#61590);
#20124=VERTEX_POINT('',#61593);
#20125=VERTEX_POINT('',#61594);
#20126=VERTEX_POINT('',#61596);
#20127=VERTEX_POINT('',#61598);
#20128=VERTEX_POINT('',#61600);
#20129=VERTEX_POINT('',#61602);
#20130=VERTEX_POINT('',#61605);
#20131=VERTEX_POINT('',#61606);
#20132=VERTEX_POINT('',#61608);
#20133=VERTEX_POINT('',#61610);
#20134=VERTEX_POINT('',#61612);
#20135=VERTEX_POINT('',#61614);
#20136=VERTEX_POINT('',#61617);
#20137=VERTEX_POINT('',#61618);
#20138=VERTEX_POINT('',#61620);
#20139=VERTEX_POINT('',#61622);
#20140=VERTEX_POINT('',#61624);
#20141=VERTEX_POINT('',#61626);
#20142=VERTEX_POINT('',#61629);
#20143=VERTEX_POINT('',#61630);
#20144=VERTEX_POINT('',#61632);
#20145=VERTEX_POINT('',#61634);
#20146=VERTEX_POINT('',#61636);
#20147=VERTEX_POINT('',#61638);
#20148=VERTEX_POINT('',#61641);
#20149=VERTEX_POINT('',#61642);
#20150=VERTEX_POINT('',#61644);
#20151=VERTEX_POINT('',#61646);
#20152=VERTEX_POINT('',#61648);
#20153=VERTEX_POINT('',#61650);
#20154=VERTEX_POINT('',#61653);
#20155=VERTEX_POINT('',#61654);
#20156=VERTEX_POINT('',#61656);
#20157=VERTEX_POINT('',#61658);
#20158=VERTEX_POINT('',#61660);
#20159=VERTEX_POINT('',#61662);
#20160=VERTEX_POINT('',#61665);
#20161=VERTEX_POINT('',#61666);
#20162=VERTEX_POINT('',#61668);
#20163=VERTEX_POINT('',#61670);
#20164=VERTEX_POINT('',#61672);
#20165=VERTEX_POINT('',#61674);
#20166=VERTEX_POINT('',#61677);
#20167=VERTEX_POINT('',#61678);
#20168=VERTEX_POINT('',#61680);
#20169=VERTEX_POINT('',#61682);
#20170=VERTEX_POINT('',#61684);
#20171=VERTEX_POINT('',#61686);
#20172=VERTEX_POINT('',#61689);
#20173=VERTEX_POINT('',#61690);
#20174=VERTEX_POINT('',#61692);
#20175=VERTEX_POINT('',#61694);
#20176=VERTEX_POINT('',#61696);
#20177=VERTEX_POINT('',#61698);
#20178=VERTEX_POINT('',#61701);
#20179=VERTEX_POINT('',#61702);
#20180=VERTEX_POINT('',#61704);
#20181=VERTEX_POINT('',#61706);
#20182=VERTEX_POINT('',#61708);
#20183=VERTEX_POINT('',#61710);
#20184=VERTEX_POINT('',#61713);
#20185=VERTEX_POINT('',#61714);
#20186=VERTEX_POINT('',#61716);
#20187=VERTEX_POINT('',#61718);
#20188=VERTEX_POINT('',#61720);
#20189=VERTEX_POINT('',#61722);
#20190=VERTEX_POINT('',#61725);
#20191=VERTEX_POINT('',#61726);
#20192=VERTEX_POINT('',#61728);
#20193=VERTEX_POINT('',#61730);
#20194=VERTEX_POINT('',#61732);
#20195=VERTEX_POINT('',#61734);
#20196=VERTEX_POINT('',#61737);
#20197=VERTEX_POINT('',#61738);
#20198=VERTEX_POINT('',#61740);
#20199=VERTEX_POINT('',#61742);
#20200=VERTEX_POINT('',#61744);
#20201=VERTEX_POINT('',#61746);
#20202=VERTEX_POINT('',#61749);
#20203=VERTEX_POINT('',#61750);
#20204=VERTEX_POINT('',#61752);
#20205=VERTEX_POINT('',#61754);
#20206=VERTEX_POINT('',#61756);
#20207=VERTEX_POINT('',#61758);
#20208=VERTEX_POINT('',#61761);
#20209=VERTEX_POINT('',#61762);
#20210=VERTEX_POINT('',#61764);
#20211=VERTEX_POINT('',#61766);
#20212=VERTEX_POINT('',#61768);
#20213=VERTEX_POINT('',#61770);
#20214=VERTEX_POINT('',#61773);
#20215=VERTEX_POINT('',#61774);
#20216=VERTEX_POINT('',#61776);
#20217=VERTEX_POINT('',#61778);
#20218=VERTEX_POINT('',#61780);
#20219=VERTEX_POINT('',#61782);
#20220=VERTEX_POINT('',#61785);
#20221=VERTEX_POINT('',#61786);
#20222=VERTEX_POINT('',#61788);
#20223=VERTEX_POINT('',#61790);
#20224=VERTEX_POINT('',#61792);
#20225=VERTEX_POINT('',#61794);
#20226=VERTEX_POINT('',#61797);
#20227=VERTEX_POINT('',#61798);
#20228=VERTEX_POINT('',#61800);
#20229=VERTEX_POINT('',#61802);
#20230=VERTEX_POINT('',#61804);
#20231=VERTEX_POINT('',#61806);
#20232=VERTEX_POINT('',#61809);
#20233=VERTEX_POINT('',#61810);
#20234=VERTEX_POINT('',#61812);
#20235=VERTEX_POINT('',#61814);
#20236=VERTEX_POINT('',#61816);
#20237=VERTEX_POINT('',#61818);
#20238=VERTEX_POINT('',#61821);
#20239=VERTEX_POINT('',#61822);
#20240=VERTEX_POINT('',#61824);
#20241=VERTEX_POINT('',#61826);
#20242=VERTEX_POINT('',#61828);
#20243=VERTEX_POINT('',#61830);
#20244=VERTEX_POINT('',#61833);
#20245=VERTEX_POINT('',#61834);
#20246=VERTEX_POINT('',#61836);
#20247=VERTEX_POINT('',#61838);
#20248=VERTEX_POINT('',#61840);
#20249=VERTEX_POINT('',#61842);
#20250=VERTEX_POINT('',#61845);
#20251=VERTEX_POINT('',#61846);
#20252=VERTEX_POINT('',#61848);
#20253=VERTEX_POINT('',#61850);
#20254=VERTEX_POINT('',#61852);
#20255=VERTEX_POINT('',#61854);
#20256=VERTEX_POINT('',#61857);
#20257=VERTEX_POINT('',#61858);
#20258=VERTEX_POINT('',#61860);
#20259=VERTEX_POINT('',#61862);
#20260=VERTEX_POINT('',#61864);
#20261=VERTEX_POINT('',#61866);
#20262=VERTEX_POINT('',#61869);
#20263=VERTEX_POINT('',#61870);
#20264=VERTEX_POINT('',#61872);
#20265=VERTEX_POINT('',#61874);
#20266=VERTEX_POINT('',#61876);
#20267=VERTEX_POINT('',#61878);
#20268=VERTEX_POINT('',#61881);
#20269=VERTEX_POINT('',#61882);
#20270=VERTEX_POINT('',#61884);
#20271=VERTEX_POINT('',#61886);
#20272=VERTEX_POINT('',#61888);
#20273=VERTEX_POINT('',#61890);
#20274=VERTEX_POINT('',#61893);
#20275=VERTEX_POINT('',#61894);
#20276=VERTEX_POINT('',#61896);
#20277=VERTEX_POINT('',#61898);
#20278=VERTEX_POINT('',#61900);
#20279=VERTEX_POINT('',#61902);
#20280=VERTEX_POINT('',#61905);
#20281=VERTEX_POINT('',#61906);
#20282=VERTEX_POINT('',#61908);
#20283=VERTEX_POINT('',#61910);
#20284=VERTEX_POINT('',#61912);
#20285=VERTEX_POINT('',#61914);
#20286=VERTEX_POINT('',#61917);
#20287=VERTEX_POINT('',#61918);
#20288=VERTEX_POINT('',#61920);
#20289=VERTEX_POINT('',#61922);
#20290=VERTEX_POINT('',#61924);
#20291=VERTEX_POINT('',#61926);
#20292=VERTEX_POINT('',#61929);
#20293=VERTEX_POINT('',#61930);
#20294=VERTEX_POINT('',#61932);
#20295=VERTEX_POINT('',#61934);
#20296=VERTEX_POINT('',#61936);
#20297=VERTEX_POINT('',#61938);
#20298=VERTEX_POINT('',#61941);
#20299=VERTEX_POINT('',#61942);
#20300=VERTEX_POINT('',#61944);
#20301=VERTEX_POINT('',#61946);
#20302=VERTEX_POINT('',#61948);
#20303=VERTEX_POINT('',#61950);
#20304=VERTEX_POINT('',#61953);
#20305=VERTEX_POINT('',#61954);
#20306=VERTEX_POINT('',#61956);
#20307=VERTEX_POINT('',#61958);
#20308=VERTEX_POINT('',#61960);
#20309=VERTEX_POINT('',#61962);
#20310=VERTEX_POINT('',#61965);
#20311=VERTEX_POINT('',#61966);
#20312=VERTEX_POINT('',#61968);
#20313=VERTEX_POINT('',#61970);
#20314=VERTEX_POINT('',#61972);
#20315=VERTEX_POINT('',#61974);
#20316=VERTEX_POINT('',#61977);
#20317=VERTEX_POINT('',#61978);
#20318=VERTEX_POINT('',#61980);
#20319=VERTEX_POINT('',#61982);
#20320=VERTEX_POINT('',#61984);
#20321=VERTEX_POINT('',#61986);
#20322=VERTEX_POINT('',#61989);
#20323=VERTEX_POINT('',#61990);
#20324=VERTEX_POINT('',#61992);
#20325=VERTEX_POINT('',#61994);
#20326=VERTEX_POINT('',#61996);
#20327=VERTEX_POINT('',#61998);
#20328=VERTEX_POINT('',#62001);
#20329=VERTEX_POINT('',#62002);
#20330=VERTEX_POINT('',#62004);
#20331=VERTEX_POINT('',#62006);
#20332=VERTEX_POINT('',#62008);
#20333=VERTEX_POINT('',#62010);
#20334=VERTEX_POINT('',#62013);
#20335=VERTEX_POINT('',#62014);
#20336=VERTEX_POINT('',#62016);
#20337=VERTEX_POINT('',#62018);
#20338=VERTEX_POINT('',#62020);
#20339=VERTEX_POINT('',#62022);
#20340=VERTEX_POINT('',#62025);
#20341=VERTEX_POINT('',#62026);
#20342=VERTEX_POINT('',#62028);
#20343=VERTEX_POINT('',#62030);
#20344=VERTEX_POINT('',#62032);
#20345=VERTEX_POINT('',#62034);
#20346=VERTEX_POINT('',#62037);
#20347=VERTEX_POINT('',#62038);
#20348=VERTEX_POINT('',#62040);
#20349=VERTEX_POINT('',#62042);
#20350=VERTEX_POINT('',#62044);
#20351=VERTEX_POINT('',#62046);
#20352=VERTEX_POINT('',#62049);
#20353=VERTEX_POINT('',#62050);
#20354=VERTEX_POINT('',#62052);
#20355=VERTEX_POINT('',#62054);
#20356=VERTEX_POINT('',#62056);
#20357=VERTEX_POINT('',#62058);
#20358=VERTEX_POINT('',#62061);
#20359=VERTEX_POINT('',#62062);
#20360=VERTEX_POINT('',#62064);
#20361=VERTEX_POINT('',#62066);
#20362=VERTEX_POINT('',#62068);
#20363=VERTEX_POINT('',#62070);
#20364=VERTEX_POINT('',#62073);
#20365=VERTEX_POINT('',#62074);
#20366=VERTEX_POINT('',#62076);
#20367=VERTEX_POINT('',#62078);
#20368=VERTEX_POINT('',#62080);
#20369=VERTEX_POINT('',#62082);
#20370=VERTEX_POINT('',#62085);
#20371=VERTEX_POINT('',#62086);
#20372=VERTEX_POINT('',#62088);
#20373=VERTEX_POINT('',#62090);
#20374=VERTEX_POINT('',#62092);
#20375=VERTEX_POINT('',#62094);
#20376=VERTEX_POINT('',#62097);
#20377=VERTEX_POINT('',#62098);
#20378=VERTEX_POINT('',#62100);
#20379=VERTEX_POINT('',#62102);
#20380=VERTEX_POINT('',#62104);
#20381=VERTEX_POINT('',#62106);
#20382=VERTEX_POINT('',#62109);
#20383=VERTEX_POINT('',#62110);
#20384=VERTEX_POINT('',#62112);
#20385=VERTEX_POINT('',#62114);
#20386=VERTEX_POINT('',#62116);
#20387=VERTEX_POINT('',#62118);
#20388=VERTEX_POINT('',#62121);
#20389=VERTEX_POINT('',#62122);
#20390=VERTEX_POINT('',#62124);
#20391=VERTEX_POINT('',#62126);
#20392=VERTEX_POINT('',#62128);
#20393=VERTEX_POINT('',#62130);
#20394=VERTEX_POINT('',#62133);
#20395=VERTEX_POINT('',#62134);
#20396=VERTEX_POINT('',#62136);
#20397=VERTEX_POINT('',#62138);
#20398=VERTEX_POINT('',#62140);
#20399=VERTEX_POINT('',#62142);
#20400=VERTEX_POINT('',#62145);
#20401=VERTEX_POINT('',#62146);
#20402=VERTEX_POINT('',#62148);
#20403=VERTEX_POINT('',#62150);
#20404=VERTEX_POINT('',#62152);
#20405=VERTEX_POINT('',#62154);
#20406=VERTEX_POINT('',#62157);
#20407=VERTEX_POINT('',#62158);
#20408=VERTEX_POINT('',#62160);
#20409=VERTEX_POINT('',#62162);
#20410=VERTEX_POINT('',#62164);
#20411=VERTEX_POINT('',#62166);
#20412=VERTEX_POINT('',#62169);
#20413=VERTEX_POINT('',#62170);
#20414=VERTEX_POINT('',#62172);
#20415=VERTEX_POINT('',#62174);
#20416=VERTEX_POINT('',#62176);
#20417=VERTEX_POINT('',#62178);
#20418=VERTEX_POINT('',#62181);
#20419=VERTEX_POINT('',#62182);
#20420=VERTEX_POINT('',#62184);
#20421=VERTEX_POINT('',#62186);
#20422=VERTEX_POINT('',#62188);
#20423=VERTEX_POINT('',#62190);
#20424=VERTEX_POINT('',#62193);
#20425=VERTEX_POINT('',#62194);
#20426=VERTEX_POINT('',#62196);
#20427=VERTEX_POINT('',#62198);
#20428=VERTEX_POINT('',#62200);
#20429=VERTEX_POINT('',#62202);
#20430=VERTEX_POINT('',#62205);
#20431=VERTEX_POINT('',#62206);
#20432=VERTEX_POINT('',#62208);
#20433=VERTEX_POINT('',#62210);
#20434=VERTEX_POINT('',#62212);
#20435=VERTEX_POINT('',#62214);
#20436=VERTEX_POINT('',#62217);
#20437=VERTEX_POINT('',#62218);
#20438=VERTEX_POINT('',#62220);
#20439=VERTEX_POINT('',#62222);
#20440=VERTEX_POINT('',#62224);
#20441=VERTEX_POINT('',#62226);
#20442=VERTEX_POINT('',#62229);
#20443=VERTEX_POINT('',#62230);
#20444=VERTEX_POINT('',#62232);
#20445=VERTEX_POINT('',#62234);
#20446=VERTEX_POINT('',#62236);
#20447=VERTEX_POINT('',#62238);
#20448=VERTEX_POINT('',#62241);
#20449=VERTEX_POINT('',#62242);
#20450=VERTEX_POINT('',#62244);
#20451=VERTEX_POINT('',#62246);
#20452=VERTEX_POINT('',#62248);
#20453=VERTEX_POINT('',#62250);
#20454=VERTEX_POINT('',#62253);
#20455=VERTEX_POINT('',#62254);
#20456=VERTEX_POINT('',#62256);
#20457=VERTEX_POINT('',#62258);
#20458=VERTEX_POINT('',#62260);
#20459=VERTEX_POINT('',#62262);
#20460=VERTEX_POINT('',#62265);
#20461=VERTEX_POINT('',#62266);
#20462=VERTEX_POINT('',#62268);
#20463=VERTEX_POINT('',#62270);
#20464=VERTEX_POINT('',#62272);
#20465=VERTEX_POINT('',#62274);
#20466=VERTEX_POINT('',#62277);
#20467=VERTEX_POINT('',#62278);
#20468=VERTEX_POINT('',#62280);
#20469=VERTEX_POINT('',#62282);
#20470=VERTEX_POINT('',#62284);
#20471=VERTEX_POINT('',#62286);
#20472=VERTEX_POINT('',#62289);
#20473=VERTEX_POINT('',#62290);
#20474=VERTEX_POINT('',#62292);
#20475=VERTEX_POINT('',#62294);
#20476=VERTEX_POINT('',#62296);
#20477=VERTEX_POINT('',#62298);
#20478=VERTEX_POINT('',#62301);
#20479=VERTEX_POINT('',#62302);
#20480=VERTEX_POINT('',#62304);
#20481=VERTEX_POINT('',#62306);
#20482=VERTEX_POINT('',#62308);
#20483=VERTEX_POINT('',#62310);
#20484=VERTEX_POINT('',#62313);
#20485=VERTEX_POINT('',#62314);
#20486=VERTEX_POINT('',#62316);
#20487=VERTEX_POINT('',#62318);
#20488=VERTEX_POINT('',#62320);
#20489=VERTEX_POINT('',#62322);
#20490=VERTEX_POINT('',#62325);
#20491=VERTEX_POINT('',#62326);
#20492=VERTEX_POINT('',#62328);
#20493=VERTEX_POINT('',#62330);
#20494=VERTEX_POINT('',#62332);
#20495=VERTEX_POINT('',#62334);
#20496=VERTEX_POINT('',#62337);
#20497=VERTEX_POINT('',#62338);
#20498=VERTEX_POINT('',#62340);
#20499=VERTEX_POINT('',#62342);
#20500=VERTEX_POINT('',#62344);
#20501=VERTEX_POINT('',#62346);
#20502=VERTEX_POINT('',#62349);
#20503=VERTEX_POINT('',#62350);
#20504=VERTEX_POINT('',#62352);
#20505=VERTEX_POINT('',#62354);
#20506=VERTEX_POINT('',#62356);
#20507=VERTEX_POINT('',#62358);
#20508=VERTEX_POINT('',#62361);
#20509=VERTEX_POINT('',#62362);
#20510=VERTEX_POINT('',#62364);
#20511=VERTEX_POINT('',#62366);
#20512=VERTEX_POINT('',#62368);
#20513=VERTEX_POINT('',#62370);
#20514=VERTEX_POINT('',#62373);
#20515=VERTEX_POINT('',#62374);
#20516=VERTEX_POINT('',#62376);
#20517=VERTEX_POINT('',#62378);
#20518=VERTEX_POINT('',#62380);
#20519=VERTEX_POINT('',#62382);
#20520=VERTEX_POINT('',#62385);
#20521=VERTEX_POINT('',#62386);
#20522=VERTEX_POINT('',#62388);
#20523=VERTEX_POINT('',#62390);
#20524=VERTEX_POINT('',#62392);
#20525=VERTEX_POINT('',#62394);
#20526=VERTEX_POINT('',#62397);
#20527=VERTEX_POINT('',#62398);
#20528=VERTEX_POINT('',#62400);
#20529=VERTEX_POINT('',#62402);
#20530=VERTEX_POINT('',#62404);
#20531=VERTEX_POINT('',#62406);
#20532=VERTEX_POINT('',#62409);
#20533=VERTEX_POINT('',#62410);
#20534=VERTEX_POINT('',#62412);
#20535=VERTEX_POINT('',#62414);
#20536=VERTEX_POINT('',#62416);
#20537=VERTEX_POINT('',#62418);
#20538=VERTEX_POINT('',#62421);
#20539=VERTEX_POINT('',#62422);
#20540=VERTEX_POINT('',#62424);
#20541=VERTEX_POINT('',#62426);
#20542=VERTEX_POINT('',#62428);
#20543=VERTEX_POINT('',#62430);
#20544=VERTEX_POINT('',#62433);
#20545=VERTEX_POINT('',#62434);
#20546=VERTEX_POINT('',#62436);
#20547=VERTEX_POINT('',#62438);
#20548=VERTEX_POINT('',#62440);
#20549=VERTEX_POINT('',#62442);
#20550=VERTEX_POINT('',#62445);
#20551=VERTEX_POINT('',#62446);
#20552=VERTEX_POINT('',#62448);
#20553=VERTEX_POINT('',#62450);
#20554=VERTEX_POINT('',#62452);
#20555=VERTEX_POINT('',#62454);
#20556=VERTEX_POINT('',#62457);
#20557=VERTEX_POINT('',#62458);
#20558=VERTEX_POINT('',#62460);
#20559=VERTEX_POINT('',#62462);
#20560=VERTEX_POINT('',#62464);
#20561=VERTEX_POINT('',#62466);
#20562=VERTEX_POINT('',#62469);
#20563=VERTEX_POINT('',#62470);
#20564=VERTEX_POINT('',#62472);
#20565=VERTEX_POINT('',#62474);
#20566=VERTEX_POINT('',#62476);
#20567=VERTEX_POINT('',#62478);
#20568=VERTEX_POINT('',#62481);
#20569=VERTEX_POINT('',#62482);
#20570=VERTEX_POINT('',#62484);
#20571=VERTEX_POINT('',#62486);
#20572=VERTEX_POINT('',#62488);
#20573=VERTEX_POINT('',#62490);
#20574=VERTEX_POINT('',#62493);
#20575=VERTEX_POINT('',#62494);
#20576=VERTEX_POINT('',#62496);
#20577=VERTEX_POINT('',#62498);
#20578=VERTEX_POINT('',#62500);
#20579=VERTEX_POINT('',#62502);
#20580=VERTEX_POINT('',#62505);
#20581=VERTEX_POINT('',#62506);
#20582=VERTEX_POINT('',#62508);
#20583=VERTEX_POINT('',#62510);
#20584=VERTEX_POINT('',#62512);
#20585=VERTEX_POINT('',#62514);
#20586=VERTEX_POINT('',#62517);
#20587=VERTEX_POINT('',#62518);
#20588=VERTEX_POINT('',#62520);
#20589=VERTEX_POINT('',#62522);
#20590=VERTEX_POINT('',#62524);
#20591=VERTEX_POINT('',#62526);
#20592=VERTEX_POINT('',#62529);
#20593=VERTEX_POINT('',#62530);
#20594=VERTEX_POINT('',#62532);
#20595=VERTEX_POINT('',#62534);
#20596=VERTEX_POINT('',#62536);
#20597=VERTEX_POINT('',#62538);
#20598=VERTEX_POINT('',#62541);
#20599=VERTEX_POINT('',#62542);
#20600=VERTEX_POINT('',#62544);
#20601=VERTEX_POINT('',#62546);
#20602=VERTEX_POINT('',#62548);
#20603=VERTEX_POINT('',#62550);
#20604=VERTEX_POINT('',#62553);
#20605=VERTEX_POINT('',#62554);
#20606=VERTEX_POINT('',#62556);
#20607=VERTEX_POINT('',#62558);
#20608=VERTEX_POINT('',#62560);
#20609=VERTEX_POINT('',#62562);
#20610=VERTEX_POINT('',#62565);
#20611=VERTEX_POINT('',#62566);
#20612=VERTEX_POINT('',#62568);
#20613=VERTEX_POINT('',#62570);
#20614=VERTEX_POINT('',#62572);
#20615=VERTEX_POINT('',#62574);
#20616=VERTEX_POINT('',#62577);
#20617=VERTEX_POINT('',#62578);
#20618=VERTEX_POINT('',#62580);
#20619=VERTEX_POINT('',#62582);
#20620=VERTEX_POINT('',#62584);
#20621=VERTEX_POINT('',#62586);
#20622=VERTEX_POINT('',#62589);
#20623=VERTEX_POINT('',#62590);
#20624=VERTEX_POINT('',#62592);
#20625=VERTEX_POINT('',#62594);
#20626=VERTEX_POINT('',#62596);
#20627=VERTEX_POINT('',#62598);
#20628=VERTEX_POINT('',#62601);
#20629=VERTEX_POINT('',#62602);
#20630=VERTEX_POINT('',#62604);
#20631=VERTEX_POINT('',#62606);
#20632=VERTEX_POINT('',#62608);
#20633=VERTEX_POINT('',#62610);
#20634=VERTEX_POINT('',#62613);
#20635=VERTEX_POINT('',#62614);
#20636=VERTEX_POINT('',#62616);
#20637=VERTEX_POINT('',#62618);
#20638=VERTEX_POINT('',#62620);
#20639=VERTEX_POINT('',#62622);
#20640=VERTEX_POINT('',#62625);
#20641=VERTEX_POINT('',#62626);
#20642=VERTEX_POINT('',#62628);
#20643=VERTEX_POINT('',#62630);
#20644=VERTEX_POINT('',#62632);
#20645=VERTEX_POINT('',#62634);
#20646=VERTEX_POINT('',#62637);
#20647=VERTEX_POINT('',#62638);
#20648=VERTEX_POINT('',#62640);
#20649=VERTEX_POINT('',#62642);
#20650=VERTEX_POINT('',#62644);
#20651=VERTEX_POINT('',#62646);
#20652=VERTEX_POINT('',#62649);
#20653=VERTEX_POINT('',#62650);
#20654=VERTEX_POINT('',#62652);
#20655=VERTEX_POINT('',#62654);
#20656=VERTEX_POINT('',#62656);
#20657=VERTEX_POINT('',#62658);
#20658=VERTEX_POINT('',#62661);
#20659=VERTEX_POINT('',#62662);
#20660=VERTEX_POINT('',#62664);
#20661=VERTEX_POINT('',#62666);
#20662=VERTEX_POINT('',#62668);
#20663=VERTEX_POINT('',#62670);
#20664=VERTEX_POINT('',#62673);
#20665=VERTEX_POINT('',#62674);
#20666=VERTEX_POINT('',#62676);
#20667=VERTEX_POINT('',#62678);
#20668=VERTEX_POINT('',#62680);
#20669=VERTEX_POINT('',#62682);
#20670=VERTEX_POINT('',#62685);
#20671=VERTEX_POINT('',#62686);
#20672=VERTEX_POINT('',#62688);
#20673=VERTEX_POINT('',#62690);
#20674=VERTEX_POINT('',#62692);
#20675=VERTEX_POINT('',#62694);
#20676=VERTEX_POINT('',#62697);
#20677=VERTEX_POINT('',#62698);
#20678=VERTEX_POINT('',#62700);
#20679=VERTEX_POINT('',#62702);
#20680=VERTEX_POINT('',#62704);
#20681=VERTEX_POINT('',#62706);
#20682=VERTEX_POINT('',#62709);
#20683=VERTEX_POINT('',#62710);
#20684=VERTEX_POINT('',#62712);
#20685=VERTEX_POINT('',#62714);
#20686=VERTEX_POINT('',#62716);
#20687=VERTEX_POINT('',#62718);
#20688=VERTEX_POINT('',#62721);
#20689=VERTEX_POINT('',#62722);
#20690=VERTEX_POINT('',#62724);
#20691=VERTEX_POINT('',#62726);
#20692=VERTEX_POINT('',#62728);
#20693=VERTEX_POINT('',#62730);
#20694=VERTEX_POINT('',#62733);
#20695=VERTEX_POINT('',#62734);
#20696=VERTEX_POINT('',#62736);
#20697=VERTEX_POINT('',#62738);
#20698=VERTEX_POINT('',#62740);
#20699=VERTEX_POINT('',#62742);
#20700=VERTEX_POINT('',#62745);
#20701=VERTEX_POINT('',#62746);
#20702=VERTEX_POINT('',#62748);
#20703=VERTEX_POINT('',#62750);
#20704=VERTEX_POINT('',#62752);
#20705=VERTEX_POINT('',#62754);
#20706=VERTEX_POINT('',#62757);
#20707=VERTEX_POINT('',#62758);
#20708=VERTEX_POINT('',#62760);
#20709=VERTEX_POINT('',#62762);
#20710=VERTEX_POINT('',#62764);
#20711=VERTEX_POINT('',#62766);
#20712=VERTEX_POINT('',#62769);
#20713=VERTEX_POINT('',#62770);
#20714=VERTEX_POINT('',#62772);
#20715=VERTEX_POINT('',#62774);
#20716=VERTEX_POINT('',#62776);
#20717=VERTEX_POINT('',#62778);
#20718=VERTEX_POINT('',#62781);
#20719=VERTEX_POINT('',#62782);
#20720=VERTEX_POINT('',#62784);
#20721=VERTEX_POINT('',#62786);
#20722=VERTEX_POINT('',#62788);
#20723=VERTEX_POINT('',#62790);
#20724=VERTEX_POINT('',#62793);
#20725=VERTEX_POINT('',#62794);
#20726=VERTEX_POINT('',#62796);
#20727=VERTEX_POINT('',#62798);
#20728=VERTEX_POINT('',#62800);
#20729=VERTEX_POINT('',#62802);
#20730=VERTEX_POINT('',#62805);
#20731=VERTEX_POINT('',#62806);
#20732=VERTEX_POINT('',#62808);
#20733=VERTEX_POINT('',#62810);
#20734=VERTEX_POINT('',#62812);
#20735=VERTEX_POINT('',#62814);
#20736=VERTEX_POINT('',#62817);
#20737=VERTEX_POINT('',#62818);
#20738=VERTEX_POINT('',#62820);
#20739=VERTEX_POINT('',#62822);
#20740=VERTEX_POINT('',#62824);
#20741=VERTEX_POINT('',#62826);
#20742=VERTEX_POINT('',#62829);
#20743=VERTEX_POINT('',#62830);
#20744=VERTEX_POINT('',#62832);
#20745=VERTEX_POINT('',#62834);
#20746=VERTEX_POINT('',#62836);
#20747=VERTEX_POINT('',#62838);
#20748=VERTEX_POINT('',#62841);
#20749=VERTEX_POINT('',#62842);
#20750=VERTEX_POINT('',#62844);
#20751=VERTEX_POINT('',#62846);
#20752=VERTEX_POINT('',#62848);
#20753=VERTEX_POINT('',#62850);
#20754=VERTEX_POINT('',#62853);
#20755=VERTEX_POINT('',#62854);
#20756=VERTEX_POINT('',#62856);
#20757=VERTEX_POINT('',#62858);
#20758=VERTEX_POINT('',#62860);
#20759=VERTEX_POINT('',#62862);
#20760=VERTEX_POINT('',#62865);
#20761=VERTEX_POINT('',#62866);
#20762=VERTEX_POINT('',#62868);
#20763=VERTEX_POINT('',#62870);
#20764=VERTEX_POINT('',#62872);
#20765=VERTEX_POINT('',#62874);
#20766=VERTEX_POINT('',#62877);
#20767=VERTEX_POINT('',#62878);
#20768=VERTEX_POINT('',#62880);
#20769=VERTEX_POINT('',#62882);
#20770=VERTEX_POINT('',#62884);
#20771=VERTEX_POINT('',#62886);
#20772=VERTEX_POINT('',#62889);
#20773=VERTEX_POINT('',#62890);
#20774=VERTEX_POINT('',#62892);
#20775=VERTEX_POINT('',#62894);
#20776=VERTEX_POINT('',#62896);
#20777=VERTEX_POINT('',#62898);
#20778=VERTEX_POINT('',#62901);
#20779=VERTEX_POINT('',#62902);
#20780=VERTEX_POINT('',#62904);
#20781=VERTEX_POINT('',#62906);
#20782=VERTEX_POINT('',#62908);
#20783=VERTEX_POINT('',#62910);
#20784=VERTEX_POINT('',#62913);
#20785=VERTEX_POINT('',#62914);
#20786=VERTEX_POINT('',#62916);
#20787=VERTEX_POINT('',#62918);
#20788=VERTEX_POINT('',#62920);
#20789=VERTEX_POINT('',#62922);
#20790=VERTEX_POINT('',#62925);
#20791=VERTEX_POINT('',#62926);
#20792=VERTEX_POINT('',#62928);
#20793=VERTEX_POINT('',#62930);
#20794=VERTEX_POINT('',#62932);
#20795=VERTEX_POINT('',#62934);
#20796=VERTEX_POINT('',#62937);
#20797=VERTEX_POINT('',#62938);
#20798=VERTEX_POINT('',#62940);
#20799=VERTEX_POINT('',#62942);
#20800=VERTEX_POINT('',#62944);
#20801=VERTEX_POINT('',#62946);
#20802=VERTEX_POINT('',#62949);
#20803=VERTEX_POINT('',#62950);
#20804=VERTEX_POINT('',#62952);
#20805=VERTEX_POINT('',#62954);
#20806=VERTEX_POINT('',#62956);
#20807=VERTEX_POINT('',#62958);
#20808=VERTEX_POINT('',#62961);
#20809=VERTEX_POINT('',#62962);
#20810=VERTEX_POINT('',#62964);
#20811=VERTEX_POINT('',#62966);
#20812=VERTEX_POINT('',#62968);
#20813=VERTEX_POINT('',#62970);
#20814=VERTEX_POINT('',#62973);
#20815=VERTEX_POINT('',#62974);
#20816=VERTEX_POINT('',#62976);
#20817=VERTEX_POINT('',#62978);
#20818=VERTEX_POINT('',#62980);
#20819=VERTEX_POINT('',#62982);
#20820=VERTEX_POINT('',#62985);
#20821=VERTEX_POINT('',#62986);
#20822=VERTEX_POINT('',#62988);
#20823=VERTEX_POINT('',#62990);
#20824=VERTEX_POINT('',#62992);
#20825=VERTEX_POINT('',#62994);
#20826=VERTEX_POINT('',#62997);
#20827=VERTEX_POINT('',#62998);
#20828=VERTEX_POINT('',#63000);
#20829=VERTEX_POINT('',#63002);
#20830=VERTEX_POINT('',#63004);
#20831=VERTEX_POINT('',#63006);
#20832=VERTEX_POINT('',#63009);
#20833=VERTEX_POINT('',#63010);
#20834=VERTEX_POINT('',#63012);
#20835=VERTEX_POINT('',#63014);
#20836=VERTEX_POINT('',#63016);
#20837=VERTEX_POINT('',#63018);
#20838=VERTEX_POINT('',#63021);
#20839=VERTEX_POINT('',#63022);
#20840=VERTEX_POINT('',#63024);
#20841=VERTEX_POINT('',#63026);
#20842=VERTEX_POINT('',#63028);
#20843=VERTEX_POINT('',#63030);
#20844=VERTEX_POINT('',#63033);
#20845=VERTEX_POINT('',#63034);
#20846=VERTEX_POINT('',#63036);
#20847=VERTEX_POINT('',#63038);
#20848=VERTEX_POINT('',#63040);
#20849=VERTEX_POINT('',#63042);
#20850=VERTEX_POINT('',#63045);
#20851=VERTEX_POINT('',#63046);
#20852=VERTEX_POINT('',#63048);
#20853=VERTEX_POINT('',#63050);
#20854=VERTEX_POINT('',#63052);
#20855=VERTEX_POINT('',#63054);
#20856=EDGE_CURVE('',#17144,#17144,#16490,.T.);
#20857=EDGE_CURVE('',#17144,#17145,#6740,.T.);
#20858=EDGE_CURVE('',#17145,#17145,#16491,.T.);
#20859=EDGE_CURVE('',#17146,#17146,#16492,.T.);
#20860=EDGE_CURVE('',#17146,#17147,#6741,.T.);
#20861=EDGE_CURVE('',#17147,#17147,#16493,.T.);
#20862=EDGE_CURVE('',#17148,#17148,#16494,.T.);
#20863=EDGE_CURVE('',#17148,#17149,#6742,.T.);
#20864=EDGE_CURVE('',#17149,#17149,#16495,.T.);
#20865=EDGE_CURVE('',#17150,#17150,#16496,.T.);
#20866=EDGE_CURVE('',#17150,#17151,#6743,.T.);
#20867=EDGE_CURVE('',#17151,#17151,#16497,.T.);
#20868=EDGE_CURVE('',#17152,#17152,#16498,.T.);
#20869=EDGE_CURVE('',#17152,#17153,#6744,.T.);
#20870=EDGE_CURVE('',#17153,#17153,#16499,.T.);
#20871=EDGE_CURVE('',#17154,#17154,#16500,.T.);
#20872=EDGE_CURVE('',#17154,#17155,#6745,.T.);
#20873=EDGE_CURVE('',#17155,#17155,#16501,.T.);
#20874=EDGE_CURVE('',#17156,#17157,#16502,.T.);
#20875=EDGE_CURVE('',#17156,#17158,#6746,.T.);
#20876=EDGE_CURVE('',#17158,#17159,#16503,.T.);
#20877=EDGE_CURVE('',#17157,#17159,#6747,.T.);
#20878=EDGE_CURVE('',#17160,#17161,#16504,.T.);
#20879=EDGE_CURVE('',#17161,#17162,#6748,.T.);
#20880=EDGE_CURVE('',#17163,#17162,#16505,.T.);
#20881=EDGE_CURVE('',#17160,#17163,#6749,.T.);
#20882=EDGE_CURVE('',#17164,#17165,#16506,.T.);
#20883=EDGE_CURVE('',#17165,#17166,#6750,.T.);
#20884=EDGE_CURVE('',#17167,#17166,#16507,.T.);
#20885=EDGE_CURVE('',#17164,#17167,#6751,.T.);
#20886=EDGE_CURVE('',#17168,#17169,#16508,.T.);
#20887=EDGE_CURVE('',#17169,#17170,#6752,.T.);
#20888=EDGE_CURVE('',#17171,#17170,#16509,.T.);
#20889=EDGE_CURVE('',#17168,#17171,#6753,.T.);
#20890=EDGE_CURVE('',#17172,#17173,#16510,.T.);
#20891=EDGE_CURVE('',#17173,#17174,#6754,.T.);
#20892=EDGE_CURVE('',#17175,#17174,#16511,.T.);
#20893=EDGE_CURVE('',#17172,#17175,#6755,.T.);
#20894=EDGE_CURVE('',#17176,#17177,#16512,.T.);
#20895=EDGE_CURVE('',#17177,#17178,#6756,.T.);
#20896=EDGE_CURVE('',#17179,#17178,#16513,.T.);
#20897=EDGE_CURVE('',#17176,#17179,#6757,.T.);
#20898=EDGE_CURVE('',#17180,#17181,#16514,.T.);
#20899=EDGE_CURVE('',#17180,#17182,#6758,.T.);
#20900=EDGE_CURVE('',#17182,#17183,#16515,.T.);
#20901=EDGE_CURVE('',#17181,#17183,#6759,.T.);
#20902=EDGE_CURVE('',#17184,#17185,#16516,.T.);
#20903=EDGE_CURVE('',#17184,#17186,#6760,.T.);
#20904=EDGE_CURVE('',#17186,#17187,#16517,.T.);
#20905=EDGE_CURVE('',#17185,#17187,#6761,.T.);
#20906=EDGE_CURVE('',#17188,#17189,#16518,.T.);
#20907=EDGE_CURVE('',#17188,#17190,#6762,.T.);
#20908=EDGE_CURVE('',#17190,#17191,#16519,.T.);
#20909=EDGE_CURVE('',#17189,#17191,#6763,.T.);
#20910=EDGE_CURVE('',#17192,#17193,#16520,.T.);
#20911=EDGE_CURVE('',#17192,#17194,#6764,.T.);
#20912=EDGE_CURVE('',#17194,#17195,#16521,.T.);
#20913=EDGE_CURVE('',#17193,#17195,#6765,.T.);
#20914=EDGE_CURVE('',#17196,#17197,#16522,.T.);
#20915=EDGE_CURVE('',#17196,#17198,#6766,.T.);
#20916=EDGE_CURVE('',#17198,#17199,#16523,.T.);
#20917=EDGE_CURVE('',#17197,#17199,#6767,.T.);
#20918=EDGE_CURVE('',#17200,#17201,#16524,.T.);
#20919=EDGE_CURVE('',#17200,#17202,#6768,.T.);
#20920=EDGE_CURVE('',#17202,#17203,#16525,.T.);
#20921=EDGE_CURVE('',#17201,#17203,#6769,.T.);
#20922=EDGE_CURVE('',#17204,#17205,#16526,.T.);
#20923=EDGE_CURVE('',#17204,#17206,#6770,.T.);
#20924=EDGE_CURVE('',#17206,#17207,#16527,.T.);
#20925=EDGE_CURVE('',#17205,#17207,#6771,.T.);
#20926=EDGE_CURVE('',#17208,#17209,#16528,.T.);
#20927=EDGE_CURVE('',#17209,#17210,#6772,.T.);
#20928=EDGE_CURVE('',#17211,#17210,#16529,.T.);
#20929=EDGE_CURVE('',#17208,#17211,#6773,.T.);
#20930=EDGE_CURVE('',#17212,#17213,#16530,.T.);
#20931=EDGE_CURVE('',#17213,#17214,#6774,.T.);
#20932=EDGE_CURVE('',#17215,#17214,#16531,.T.);
#20933=EDGE_CURVE('',#17212,#17215,#6775,.T.);
#20934=EDGE_CURVE('',#17216,#17217,#16532,.T.);
#20935=EDGE_CURVE('',#17217,#17218,#6776,.T.);
#20936=EDGE_CURVE('',#17219,#17218,#16533,.T.);
#20937=EDGE_CURVE('',#17216,#17219,#6777,.T.);
#20938=EDGE_CURVE('',#17220,#17221,#16534,.T.);
#20939=EDGE_CURVE('',#17221,#17222,#6778,.T.);
#20940=EDGE_CURVE('',#17223,#17222,#16535,.T.);
#20941=EDGE_CURVE('',#17220,#17223,#6779,.T.);
#20942=EDGE_CURVE('',#17224,#17225,#16536,.T.);
#20943=EDGE_CURVE('',#17224,#17226,#6780,.T.);
#20944=EDGE_CURVE('',#17226,#17227,#16537,.T.);
#20945=EDGE_CURVE('',#17225,#17227,#6781,.T.);
#20946=EDGE_CURVE('',#17228,#17229,#16538,.T.);
#20947=EDGE_CURVE('',#17228,#17230,#6782,.T.);
#20948=EDGE_CURVE('',#17230,#17231,#16539,.T.);
#20949=EDGE_CURVE('',#17229,#17231,#6783,.T.);
#20950=EDGE_CURVE('',#17232,#17233,#16540,.T.);
#20951=EDGE_CURVE('',#17233,#17234,#6784,.T.);
#20952=EDGE_CURVE('',#17235,#17234,#16541,.T.);
#20953=EDGE_CURVE('',#17232,#17235,#6785,.T.);
#20954=EDGE_CURVE('',#17236,#17237,#16542,.T.);
#20955=EDGE_CURVE('',#17236,#17238,#6786,.T.);
#20956=EDGE_CURVE('',#17238,#17239,#16543,.T.);
#20957=EDGE_CURVE('',#17237,#17239,#6787,.T.);
#20958=EDGE_CURVE('',#17240,#17241,#16544,.T.);
#20959=EDGE_CURVE('',#17241,#17242,#6788,.T.);
#20960=EDGE_CURVE('',#17243,#17242,#16545,.T.);
#20961=EDGE_CURVE('',#17240,#17243,#6789,.T.);
#20962=EDGE_CURVE('',#17244,#17245,#16546,.T.);
#20963=EDGE_CURVE('',#17245,#17246,#6790,.T.);
#20964=EDGE_CURVE('',#17247,#17246,#16547,.T.);
#20965=EDGE_CURVE('',#17244,#17247,#6791,.T.);
#20966=EDGE_CURVE('',#17248,#17249,#16548,.T.);
#20967=EDGE_CURVE('',#17248,#17250,#6792,.T.);
#20968=EDGE_CURVE('',#17250,#17251,#16549,.T.);
#20969=EDGE_CURVE('',#17249,#17251,#6793,.T.);
#20970=EDGE_CURVE('',#17252,#17253,#16550,.T.);
#20971=EDGE_CURVE('',#17253,#17254,#6794,.T.);
#20972=EDGE_CURVE('',#17255,#17254,#16551,.T.);
#20973=EDGE_CURVE('',#17252,#17255,#6795,.T.);
#20974=EDGE_CURVE('',#17256,#17257,#16552,.T.);
#20975=EDGE_CURVE('',#17256,#17258,#6796,.T.);
#20976=EDGE_CURVE('',#17258,#17259,#16553,.T.);
#20977=EDGE_CURVE('',#17257,#17259,#6797,.T.);
#20978=EDGE_CURVE('',#17260,#17261,#16554,.T.);
#20979=EDGE_CURVE('',#17260,#17262,#6798,.T.);
#20980=EDGE_CURVE('',#17262,#17263,#16555,.T.);
#20981=EDGE_CURVE('',#17261,#17263,#6799,.T.);
#20982=EDGE_CURVE('',#17264,#17265,#16556,.T.);
#20983=EDGE_CURVE('',#17264,#17266,#6800,.T.);
#20984=EDGE_CURVE('',#17266,#17267,#16557,.T.);
#20985=EDGE_CURVE('',#17265,#17267,#6801,.T.);
#20986=EDGE_CURVE('',#17268,#17269,#16558,.T.);
#20987=EDGE_CURVE('',#17268,#17270,#6802,.T.);
#20988=EDGE_CURVE('',#17270,#17271,#16559,.T.);
#20989=EDGE_CURVE('',#17269,#17271,#6803,.T.);
#20990=EDGE_CURVE('',#17272,#17273,#16560,.T.);
#20991=EDGE_CURVE('',#17272,#17274,#6804,.T.);
#20992=EDGE_CURVE('',#17274,#17275,#16561,.T.);
#20993=EDGE_CURVE('',#17273,#17275,#6805,.T.);
#20994=EDGE_CURVE('',#17276,#17277,#16562,.T.);
#20995=EDGE_CURVE('',#17277,#17278,#6806,.T.);
#20996=EDGE_CURVE('',#17279,#17278,#16563,.T.);
#20997=EDGE_CURVE('',#17276,#17279,#6807,.T.);
#20998=EDGE_CURVE('',#17280,#17281,#16564,.T.);
#20999=EDGE_CURVE('',#17281,#17282,#6808,.T.);
#21000=EDGE_CURVE('',#17283,#17282,#16565,.T.);
#21001=EDGE_CURVE('',#17280,#17283,#6809,.T.);
#21002=EDGE_CURVE('',#17284,#17285,#16566,.T.);
#21003=EDGE_CURVE('',#17285,#17286,#6810,.T.);
#21004=EDGE_CURVE('',#17287,#17286,#16567,.T.);
#21005=EDGE_CURVE('',#17284,#17287,#6811,.T.);
#21006=EDGE_CURVE('',#17288,#17289,#16568,.T.);
#21007=EDGE_CURVE('',#17289,#17290,#6812,.T.);
#21008=EDGE_CURVE('',#17291,#17290,#16569,.T.);
#21009=EDGE_CURVE('',#17288,#17291,#6813,.T.);
#21010=EDGE_CURVE('',#17292,#17293,#16570,.T.);
#21011=EDGE_CURVE('',#17293,#17294,#6814,.T.);
#21012=EDGE_CURVE('',#17295,#17294,#16571,.T.);
#21013=EDGE_CURVE('',#17292,#17295,#6815,.T.);
#21014=EDGE_CURVE('',#17296,#17297,#16572,.T.);
#21015=EDGE_CURVE('',#17297,#17298,#6816,.T.);
#21016=EDGE_CURVE('',#17299,#17298,#16573,.T.);
#21017=EDGE_CURVE('',#17296,#17299,#6817,.T.);
#21018=EDGE_CURVE('',#17300,#17301,#16574,.T.);
#21019=EDGE_CURVE('',#17301,#17302,#6818,.T.);
#21020=EDGE_CURVE('',#17303,#17302,#16575,.T.);
#21021=EDGE_CURVE('',#17300,#17303,#6819,.T.);
#21022=EDGE_CURVE('',#17304,#17305,#16576,.T.);
#21023=EDGE_CURVE('',#17304,#17306,#6820,.T.);
#21024=EDGE_CURVE('',#17306,#17307,#16577,.T.);
#21025=EDGE_CURVE('',#17305,#17307,#6821,.T.);
#21026=EDGE_CURVE('',#17308,#17309,#16578,.T.);
#21027=EDGE_CURVE('',#17308,#17310,#6822,.T.);
#21028=EDGE_CURVE('',#17310,#17311,#16579,.T.);
#21029=EDGE_CURVE('',#17309,#17311,#6823,.T.);
#21030=EDGE_CURVE('',#17312,#17313,#16580,.T.);
#21031=EDGE_CURVE('',#17312,#17314,#6824,.T.);
#21032=EDGE_CURVE('',#17314,#17315,#16581,.T.);
#21033=EDGE_CURVE('',#17313,#17315,#6825,.T.);
#21034=EDGE_CURVE('',#17316,#17317,#16582,.T.);
#21035=EDGE_CURVE('',#17316,#17318,#6826,.T.);
#21036=EDGE_CURVE('',#17318,#17319,#16583,.T.);
#21037=EDGE_CURVE('',#17317,#17319,#6827,.T.);
#21038=EDGE_CURVE('',#17320,#17321,#16584,.T.);
#21039=EDGE_CURVE('',#17321,#17322,#6828,.T.);
#21040=EDGE_CURVE('',#17323,#17322,#16585,.T.);
#21041=EDGE_CURVE('',#17320,#17323,#6829,.T.);
#21042=EDGE_CURVE('',#17324,#17325,#16586,.T.);
#21043=EDGE_CURVE('',#17325,#17326,#6830,.T.);
#21044=EDGE_CURVE('',#17327,#17326,#16587,.T.);
#21045=EDGE_CURVE('',#17324,#17327,#6831,.T.);
#21046=EDGE_CURVE('',#17328,#17329,#16588,.T.);
#21047=EDGE_CURVE('',#17328,#17330,#6832,.T.);
#21048=EDGE_CURVE('',#17330,#17331,#16589,.T.);
#21049=EDGE_CURVE('',#17329,#17331,#6833,.T.);
#21050=EDGE_CURVE('',#17332,#17333,#16590,.T.);
#21051=EDGE_CURVE('',#17333,#17334,#6834,.T.);
#21052=EDGE_CURVE('',#17335,#17334,#16591,.T.);
#21053=EDGE_CURVE('',#17332,#17335,#6835,.T.);
#21054=EDGE_CURVE('',#17336,#17337,#16592,.T.);
#21055=EDGE_CURVE('',#17336,#17338,#6836,.T.);
#21056=EDGE_CURVE('',#17338,#17339,#16593,.T.);
#21057=EDGE_CURVE('',#17337,#17339,#6837,.T.);
#21058=EDGE_CURVE('',#17340,#17341,#16594,.T.);
#21059=EDGE_CURVE('',#17340,#17342,#6838,.T.);
#21060=EDGE_CURVE('',#17342,#17343,#16595,.T.);
#21061=EDGE_CURVE('',#17341,#17343,#6839,.T.);
#21062=EDGE_CURVE('',#17344,#17345,#16596,.T.);
#21063=EDGE_CURVE('',#17345,#17346,#6840,.T.);
#21064=EDGE_CURVE('',#17347,#17346,#16597,.T.);
#21065=EDGE_CURVE('',#17344,#17347,#6841,.T.);
#21066=EDGE_CURVE('',#17348,#17349,#16598,.T.);
#21067=EDGE_CURVE('',#17350,#17348,#6842,.T.);
#21068=EDGE_CURVE('',#17351,#17350,#16599,.T.);
#21069=EDGE_CURVE('',#17349,#17351,#6843,.T.);
#21070=EDGE_CURVE('',#17352,#17353,#16600,.T.);
#21071=EDGE_CURVE('',#17354,#17352,#6844,.T.);
#21072=EDGE_CURVE('',#17355,#17354,#16601,.T.);
#21073=EDGE_CURVE('',#17353,#17355,#6845,.T.);
#21074=EDGE_CURVE('',#17356,#17357,#16602,.T.);
#21075=EDGE_CURVE('',#17358,#17356,#6846,.T.);
#21076=EDGE_CURVE('',#17359,#17358,#16603,.T.);
#21077=EDGE_CURVE('',#17357,#17359,#6847,.T.);
#21078=EDGE_CURVE('',#17360,#17361,#16604,.T.);
#21079=EDGE_CURVE('',#17362,#17360,#6848,.T.);
#21080=EDGE_CURVE('',#17363,#17362,#16605,.T.);
#21081=EDGE_CURVE('',#17361,#17363,#6849,.T.);
#21082=EDGE_CURVE('',#17364,#17365,#16606,.T.);
#21083=EDGE_CURVE('',#17366,#17364,#6850,.T.);
#21084=EDGE_CURVE('',#17367,#17366,#16607,.T.);
#21085=EDGE_CURVE('',#17365,#17367,#6851,.T.);
#21086=EDGE_CURVE('',#17368,#17369,#16608,.T.);
#21087=EDGE_CURVE('',#17370,#17368,#6852,.T.);
#21088=EDGE_CURVE('',#17371,#17370,#16609,.T.);
#21089=EDGE_CURVE('',#17369,#17371,#6853,.T.);
#21090=EDGE_CURVE('',#17372,#17373,#16610,.T.);
#21091=EDGE_CURVE('',#17374,#17372,#6854,.T.);
#21092=EDGE_CURVE('',#17375,#17374,#16611,.T.);
#21093=EDGE_CURVE('',#17373,#17375,#6855,.T.);
#21094=EDGE_CURVE('',#17376,#17377,#16612,.T.);
#21095=EDGE_CURVE('',#17378,#17376,#6856,.T.);
#21096=EDGE_CURVE('',#17379,#17378,#16613,.T.);
#21097=EDGE_CURVE('',#17377,#17379,#6857,.T.);
#21098=EDGE_CURVE('',#17380,#17381,#16614,.T.);
#21099=EDGE_CURVE('',#17382,#17380,#6858,.T.);
#21100=EDGE_CURVE('',#17383,#17382,#16615,.T.);
#21101=EDGE_CURVE('',#17381,#17383,#6859,.T.);
#21102=EDGE_CURVE('',#17384,#17385,#16616,.T.);
#21103=EDGE_CURVE('',#17386,#17384,#6860,.T.);
#21104=EDGE_CURVE('',#17387,#17386,#16617,.T.);
#21105=EDGE_CURVE('',#17385,#17387,#6861,.T.);
#21106=EDGE_CURVE('',#17388,#17389,#16618,.T.);
#21107=EDGE_CURVE('',#17390,#17388,#6862,.T.);
#21108=EDGE_CURVE('',#17391,#17390,#16619,.T.);
#21109=EDGE_CURVE('',#17389,#17391,#6863,.T.);
#21110=EDGE_CURVE('',#17392,#17393,#16620,.T.);
#21111=EDGE_CURVE('',#17394,#17392,#6864,.T.);
#21112=EDGE_CURVE('',#17395,#17394,#16621,.T.);
#21113=EDGE_CURVE('',#17393,#17395,#6865,.T.);
#21114=EDGE_CURVE('',#17396,#17397,#16622,.T.);
#21115=EDGE_CURVE('',#17398,#17396,#6866,.T.);
#21116=EDGE_CURVE('',#17399,#17398,#16623,.T.);
#21117=EDGE_CURVE('',#17397,#17399,#6867,.T.);
#21118=EDGE_CURVE('',#17400,#17401,#16624,.T.);
#21119=EDGE_CURVE('',#17402,#17400,#6868,.T.);
#21120=EDGE_CURVE('',#17403,#17402,#16625,.T.);
#21121=EDGE_CURVE('',#17401,#17403,#6869,.T.);
#21122=EDGE_CURVE('',#17404,#17405,#16626,.T.);
#21123=EDGE_CURVE('',#17406,#17404,#6870,.T.);
#21124=EDGE_CURVE('',#17407,#17406,#16627,.T.);
#21125=EDGE_CURVE('',#17405,#17407,#6871,.T.);
#21126=EDGE_CURVE('',#17408,#17409,#16628,.T.);
#21127=EDGE_CURVE('',#17410,#17408,#6872,.T.);
#21128=EDGE_CURVE('',#17411,#17410,#16629,.T.);
#21129=EDGE_CURVE('',#17409,#17411,#6873,.T.);
#21130=EDGE_CURVE('',#17412,#17413,#16630,.T.);
#21131=EDGE_CURVE('',#17414,#17412,#6874,.T.);
#21132=EDGE_CURVE('',#17415,#17414,#16631,.T.);
#21133=EDGE_CURVE('',#17413,#17415,#6875,.T.);
#21134=EDGE_CURVE('',#17416,#17417,#16632,.T.);
#21135=EDGE_CURVE('',#17418,#17416,#6876,.T.);
#21136=EDGE_CURVE('',#17419,#17418,#16633,.T.);
#21137=EDGE_CURVE('',#17417,#17419,#6877,.T.);
#21138=EDGE_CURVE('',#17420,#17421,#2193,.T.);
#21139=EDGE_CURVE('',#17420,#17422,#6878,.T.);
#21140=EDGE_CURVE('',#17423,#17422,#2194,.T.);
#21141=EDGE_CURVE('',#17423,#17421,#6879,.T.);
#21142=EDGE_CURVE('',#17424,#17425,#2195,.T.);
#21143=EDGE_CURVE('',#17424,#17426,#6880,.T.);
#21144=EDGE_CURVE('',#17427,#17426,#2196,.T.);
#21145=EDGE_CURVE('',#17427,#17425,#6881,.T.);
#21146=EDGE_CURVE('',#17428,#17429,#2197,.T.);
#21147=EDGE_CURVE('',#17429,#17430,#6882,.T.);
#21148=EDGE_CURVE('',#17431,#17430,#2198,.T.);
#21149=EDGE_CURVE('',#17431,#17428,#6883,.T.);
#21150=EDGE_CURVE('',#17432,#17433,#2199,.T.);
#21151=EDGE_CURVE('',#17432,#17434,#6884,.T.);
#21152=EDGE_CURVE('',#17435,#17434,#2200,.T.);
#21153=EDGE_CURVE('',#17435,#17433,#6885,.T.);
#21154=EDGE_CURVE('',#17436,#17437,#2201,.T.);
#21155=EDGE_CURVE('',#17437,#17438,#6886,.T.);
#21156=EDGE_CURVE('',#17439,#17438,#2202,.T.);
#21157=EDGE_CURVE('',#17439,#17436,#6887,.T.);
#21158=EDGE_CURVE('',#17440,#17440,#16634,.T.);
#21159=EDGE_CURVE('',#17440,#17441,#6888,.T.);
#21160=EDGE_CURVE('',#17441,#17441,#16635,.T.);
#21161=EDGE_CURVE('',#17442,#17442,#16636,.T.);
#21162=EDGE_CURVE('',#17442,#17443,#6889,.T.);
#21163=EDGE_CURVE('',#17443,#17443,#16637,.T.);
#21164=EDGE_CURVE('',#17444,#17444,#16638,.T.);
#21165=EDGE_CURVE('',#17444,#17445,#6890,.T.);
#21166=EDGE_CURVE('',#17445,#17445,#16639,.T.);
#21167=EDGE_CURVE('',#17446,#17446,#16640,.T.);
#21168=EDGE_CURVE('',#17446,#17447,#6891,.T.);
#21169=EDGE_CURVE('',#17447,#17447,#16641,.T.);
#21170=EDGE_CURVE('',#17448,#17448,#16642,.T.);
#21171=EDGE_CURVE('',#17448,#17449,#16643,.T.);
#21172=EDGE_CURVE('',#17449,#17449,#16644,.T.);
#21173=EDGE_CURVE('',#17450,#17450,#16645,.T.);
#21174=EDGE_CURVE('',#17450,#17451,#16646,.T.);
#21175=EDGE_CURVE('',#17451,#17451,#16647,.T.);
#21176=EDGE_CURVE('',#17452,#17452,#16648,.T.);
#21177=EDGE_CURVE('',#17452,#17450,#16649,.T.);
#21178=EDGE_CURVE('',#17453,#17453,#16650,.T.);
#21179=EDGE_CURVE('',#17453,#17448,#16651,.T.);
#21180=EDGE_CURVE('',#17454,#17454,#16652,.T.);
#21181=EDGE_CURVE('',#17454,#17455,#6892,.T.);
#21182=EDGE_CURVE('',#17455,#17455,#16653,.T.);
#21183=EDGE_CURVE('',#17456,#17456,#16654,.T.);
#21184=EDGE_CURVE('',#17456,#17457,#6893,.T.);
#21185=EDGE_CURVE('',#17457,#17457,#16655,.T.);
#21186=EDGE_CURVE('',#17458,#17458,#16656,.T.);
#21187=EDGE_CURVE('',#17458,#17459,#6894,.T.);
#21188=EDGE_CURVE('',#17459,#17459,#16657,.T.);
#21189=EDGE_CURVE('',#17460,#17460,#16658,.T.);
#21190=EDGE_CURVE('',#17460,#17461,#6895,.T.);
#21191=EDGE_CURVE('',#17461,#17461,#16659,.T.);
#21192=EDGE_CURVE('',#17462,#17463,#2203,.T.);
#21193=EDGE_CURVE('',#17463,#17464,#6896,.T.);
#21194=EDGE_CURVE('',#17465,#17464,#2204,.T.);
#21195=EDGE_CURVE('',#17465,#17462,#6897,.T.);
#21196=EDGE_CURVE('',#17466,#17467,#6898,.T.);
#21197=EDGE_CURVE('',#17466,#17468,#6899,.T.);
#21198=EDGE_CURVE('',#17469,#17468,#6900,.T.);
#21199=EDGE_CURVE('',#17470,#17469,#16660,.T.);
#21200=EDGE_CURVE('',#17471,#17470,#6901,.T.);
#21201=EDGE_CURVE('',#17472,#17471,#16661,.T.);
#21202=EDGE_CURVE('',#17473,#17472,#6902,.T.);
#21203=EDGE_CURVE('',#17474,#17473,#6903,.T.);
#21204=EDGE_CURVE('',#17475,#17474,#6904,.T.);
#21205=EDGE_CURVE('',#17476,#17475,#6905,.T.);
#21206=EDGE_CURVE('',#17477,#17476,#6906,.T.);
#21207=EDGE_CURVE('',#17478,#17477,#6907,.T.);
#21208=EDGE_CURVE('',#17479,#17478,#6908,.T.);
#21209=EDGE_CURVE('',#17480,#17479,#6909,.T.);
#21210=EDGE_CURVE('',#17481,#17480,#6910,.T.);
#21211=EDGE_CURVE('',#17482,#17481,#6911,.T.);
#21212=EDGE_CURVE('',#17483,#17482,#6912,.T.);
#21213=EDGE_CURVE('',#17484,#17483,#16662,.T.);
#21214=EDGE_CURVE('',#17484,#17485,#6913,.T.);
#21215=EDGE_CURVE('',#17486,#17485,#16663,.T.);
#21216=EDGE_CURVE('',#17487,#17486,#6914,.T.);
#21217=EDGE_CURVE('',#17487,#17488,#6915,.T.);
#21218=EDGE_CURVE('',#17489,#17488,#6916,.T.);
#21219=EDGE_CURVE('',#17490,#17489,#6917,.T.);
#21220=EDGE_CURVE('',#17491,#17490,#6918,.T.);
#21221=EDGE_CURVE('',#17492,#17491,#6919,.T.);
#21222=EDGE_CURVE('',#17493,#17492,#6920,.T.);
#21223=EDGE_CURVE('',#17467,#17493,#6921,.T.);
#21224=EDGE_CURVE('',#17494,#17495,#6922,.T.);
#21225=EDGE_CURVE('',#17494,#17496,#6923,.T.);
#21226=EDGE_CURVE('',#17497,#17496,#6924,.T.);
#21227=EDGE_CURVE('',#17497,#17498,#6925,.T.);
#21228=EDGE_CURVE('',#17499,#17498,#6926,.T.);
#21229=EDGE_CURVE('',#17500,#17499,#6927,.T.);
#21230=EDGE_CURVE('',#17501,#17500,#6928,.T.);
#21231=EDGE_CURVE('',#17501,#17495,#6929,.T.);
#21232=EDGE_CURVE('',#17502,#17503,#6930,.T.);
#21233=EDGE_CURVE('',#17502,#17504,#6931,.T.);
#21234=EDGE_CURVE('',#17505,#17504,#6932,.T.);
#21235=EDGE_CURVE('',#17505,#17506,#6933,.T.);
#21236=EDGE_CURVE('',#17507,#17506,#6934,.T.);
#21237=EDGE_CURVE('',#17508,#17507,#6935,.T.);
#21238=EDGE_CURVE('',#17509,#17508,#6936,.T.);
#21239=EDGE_CURVE('',#17509,#17503,#6937,.T.);
#21240=EDGE_CURVE('',#17510,#17511,#6938,.T.);
#21241=EDGE_CURVE('',#17510,#17512,#6939,.T.);
#21242=EDGE_CURVE('',#17513,#17512,#6940,.T.);
#21243=EDGE_CURVE('',#17513,#17514,#6941,.T.);
#21244=EDGE_CURVE('',#17515,#17514,#6942,.T.);
#21245=EDGE_CURVE('',#17516,#17515,#6943,.T.);
#21246=EDGE_CURVE('',#17517,#17516,#6944,.T.);
#21247=EDGE_CURVE('',#17517,#17511,#6945,.T.);
#21248=EDGE_CURVE('',#17518,#17519,#6946,.T.);
#21249=EDGE_CURVE('',#17518,#17520,#6947,.T.);
#21250=EDGE_CURVE('',#17521,#17520,#6948,.T.);
#21251=EDGE_CURVE('',#17521,#17522,#6949,.T.);
#21252=EDGE_CURVE('',#17523,#17522,#6950,.T.);
#21253=EDGE_CURVE('',#17524,#17523,#6951,.T.);
#21254=EDGE_CURVE('',#17525,#17524,#6952,.T.);
#21255=EDGE_CURVE('',#17525,#17519,#6953,.T.);
#21256=EDGE_CURVE('',#17526,#17527,#6954,.T.);
#21257=EDGE_CURVE('',#17526,#17528,#6955,.T.);
#21258=EDGE_CURVE('',#17528,#17529,#6956,.T.);
#21259=EDGE_CURVE('',#17529,#17530,#6957,.T.);
#21260=EDGE_CURVE('',#17530,#17531,#6958,.T.);
#21261=EDGE_CURVE('',#17531,#17532,#6959,.T.);
#21262=EDGE_CURVE('',#17532,#17533,#6960,.T.);
#21263=EDGE_CURVE('',#17533,#17534,#6961,.T.);
#21264=EDGE_CURVE('',#17535,#17534,#6962,.T.);
#21265=EDGE_CURVE('',#17536,#17535,#6963,.T.);
#21266=EDGE_CURVE('',#17537,#17536,#16664,.T.);
#21267=EDGE_CURVE('',#17538,#17537,#6964,.T.);
#21268=EDGE_CURVE('',#17539,#17538,#16665,.T.);
#21269=EDGE_CURVE('',#17540,#17539,#6965,.T.);
#21270=EDGE_CURVE('',#17540,#17541,#6966,.T.);
#21271=EDGE_CURVE('',#17541,#17542,#6967,.T.);
#21272=EDGE_CURVE('',#17542,#17543,#6968,.T.);
#21273=EDGE_CURVE('',#17543,#17544,#6969,.T.);
#21274=EDGE_CURVE('',#17544,#17545,#6970,.T.);
#21275=EDGE_CURVE('',#17545,#17546,#6971,.T.);
#21276=EDGE_CURVE('',#17546,#17547,#6972,.T.);
#21277=EDGE_CURVE('',#17547,#17548,#6973,.T.);
#21278=EDGE_CURVE('',#17548,#17549,#6974,.T.);
#21279=EDGE_CURVE('',#17550,#17549,#6975,.T.);
#21280=EDGE_CURVE('',#17551,#17550,#16666,.T.);
#21281=EDGE_CURVE('',#17551,#17552,#6976,.T.);
#21282=EDGE_CURVE('',#17553,#17552,#16667,.T.);
#21283=EDGE_CURVE('',#17527,#17553,#6977,.T.);
#21284=EDGE_CURVE('',#17554,#17555,#6978,.T.);
#21285=EDGE_CURVE('',#17556,#17554,#6979,.T.);
#21286=EDGE_CURVE('',#17556,#17557,#6980,.T.);
#21287=EDGE_CURVE('',#17555,#17557,#6981,.T.);
#21288=EDGE_CURVE('',#17558,#17559,#6982,.T.);
#21289=EDGE_CURVE('',#17560,#17558,#6983,.T.);
#21290=EDGE_CURVE('',#17560,#17561,#6984,.T.);
#21291=EDGE_CURVE('',#17559,#17561,#6985,.T.);
#21292=EDGE_CURVE('',#17562,#17563,#6986,.T.);
#21293=EDGE_CURVE('',#17564,#17562,#6987,.T.);
#21294=EDGE_CURVE('',#17564,#17565,#6988,.T.);
#21295=EDGE_CURVE('',#17563,#17565,#6989,.T.);
#21296=EDGE_CURVE('',#17566,#17567,#6990,.T.);
#21297=EDGE_CURVE('',#17568,#17566,#6991,.T.);
#21298=EDGE_CURVE('',#17568,#17569,#6992,.T.);
#21299=EDGE_CURVE('',#17567,#17569,#6993,.T.);
#21300=EDGE_CURVE('',#17466,#17526,#6994,.T.);
#21301=EDGE_CURVE('',#17468,#17527,#6995,.T.);
#21302=EDGE_CURVE('',#17488,#17534,#6996,.T.);
#21303=EDGE_CURVE('',#17535,#17487,#6997,.T.);
#21304=EDGE_CURVE('',#17570,#17571,#6998,.T.);
#21305=EDGE_CURVE('',#17572,#17570,#6999,.T.);
#21306=EDGE_CURVE('',#17573,#17572,#7000,.T.);
#21307=EDGE_CURVE('',#17574,#17573,#16668,.T.);
#21308=EDGE_CURVE('',#17575,#17574,#7001,.T.);
#21309=EDGE_CURVE('',#17571,#17575,#16669,.T.);
#21310=EDGE_CURVE('',#17576,#17577,#7002,.T.);
#21311=EDGE_CURVE('',#17577,#17578,#7003,.T.);
#21312=EDGE_CURVE('',#17579,#17578,#7004,.T.);
#21313=EDGE_CURVE('',#17579,#17580,#7005,.T.);
#21314=EDGE_CURVE('',#17580,#17581,#7006,.T.);
#21315=EDGE_CURVE('',#17581,#17582,#7007,.T.);
#21316=EDGE_CURVE('',#17582,#17583,#7008,.T.);
#21317=EDGE_CURVE('',#17583,#17576,#7009,.T.);
#21318=EDGE_CURVE('',#17584,#17585,#7010,.T.);
#21319=EDGE_CURVE('',#17584,#17586,#7011,.T.);
#21320=EDGE_CURVE('',#17587,#17586,#7012,.T.);
#21321=EDGE_CURVE('',#17587,#17588,#7013,.T.);
#21322=EDGE_CURVE('',#17589,#17588,#7014,.T.);
#21323=EDGE_CURVE('',#17589,#17590,#7015,.T.);
#21324=EDGE_CURVE('',#17590,#17591,#7016,.T.);
#21325=EDGE_CURVE('',#17591,#17585,#7017,.T.);
#21326=EDGE_CURVE('',#17592,#17593,#7018,.T.);
#21327=EDGE_CURVE('',#17592,#17594,#7019,.T.);
#21328=EDGE_CURVE('',#17594,#17595,#16670,.T.);
#21329=EDGE_CURVE('',#17595,#17596,#7020,.T.);
#21330=EDGE_CURVE('',#17596,#17597,#16671,.T.);
#21331=EDGE_CURVE('',#17597,#17593,#7021,.T.);
#21332=EDGE_CURVE('',#17598,#17599,#7022,.T.);
#21333=EDGE_CURVE('',#17600,#17598,#7023,.T.);
#21334=EDGE_CURVE('',#17600,#17601,#7024,.T.);
#21335=EDGE_CURVE('',#17599,#17601,#7025,.T.);
#21336=EDGE_CURVE('',#17602,#17603,#7026,.T.);
#21337=EDGE_CURVE('',#17603,#17604,#7027,.T.);
#21338=EDGE_CURVE('',#17604,#17605,#7028,.T.);
#21339=EDGE_CURVE('',#17602,#17605,#7029,.T.);
#21340=EDGE_CURVE('',#17481,#17541,#7030,.T.);
#21341=EDGE_CURVE('',#17482,#17540,#7031,.T.);
#21342=EDGE_CURVE('',#17474,#17548,#7032,.T.);
#21343=EDGE_CURVE('',#17549,#17473,#7033,.T.);
#21344=EDGE_CURVE('',#17606,#17607,#7034,.T.);
#21345=EDGE_CURVE('',#17606,#17608,#7035,.T.);
#21346=EDGE_CURVE('',#17609,#17608,#7036,.T.);
#21347=EDGE_CURVE('',#17609,#17610,#7037,.T.);
#21348=EDGE_CURVE('',#17610,#17611,#7038,.T.);
#21349=EDGE_CURVE('',#17612,#17611,#7039,.T.);
#21350=EDGE_CURVE('',#17613,#17612,#16672,.T.);
#21351=EDGE_CURVE('',#17613,#17614,#7040,.T.);
#21352=EDGE_CURVE('',#17615,#17614,#16673,.T.);
#21353=EDGE_CURVE('',#17607,#17615,#7041,.T.);
#21354=EDGE_CURVE('',#17616,#17347,#7042,.T.);
#21355=EDGE_CURVE('',#17617,#17346,#7043,.T.);
#21356=EDGE_CURVE('',#17617,#17616,#16674,.T.);
#21357=EDGE_CURVE('',#17618,#17335,#7044,.T.);
#21358=EDGE_CURVE('',#17619,#17334,#7045,.T.);
#21359=EDGE_CURVE('',#17619,#17618,#16675,.T.);
#21360=EDGE_CURVE('',#17620,#17327,#7046,.T.);
#21361=EDGE_CURVE('',#17621,#17326,#7047,.T.);
#21362=EDGE_CURVE('',#17621,#17620,#16676,.T.);
#21363=EDGE_CURVE('',#17622,#17323,#7048,.T.);
#21364=EDGE_CURVE('',#17623,#17322,#7049,.T.);
#21365=EDGE_CURVE('',#17623,#17622,#16677,.T.);
#21366=EDGE_CURVE('',#17624,#17303,#7050,.T.);
#21367=EDGE_CURVE('',#17625,#17302,#7051,.T.);
#21368=EDGE_CURVE('',#17625,#17624,#16678,.T.);
#21369=EDGE_CURVE('',#17626,#17299,#7052,.T.);
#21370=EDGE_CURVE('',#17627,#17298,#7053,.T.);
#21371=EDGE_CURVE('',#17627,#17626,#16679,.T.);
#21372=EDGE_CURVE('',#17628,#17295,#7054,.T.);
#21373=EDGE_CURVE('',#17629,#17294,#7055,.T.);
#21374=EDGE_CURVE('',#17629,#17628,#16680,.T.);
#21375=EDGE_CURVE('',#17630,#17291,#7056,.T.);
#21376=EDGE_CURVE('',#17631,#17290,#7057,.T.);
#21377=EDGE_CURVE('',#17631,#17630,#16681,.T.);
#21378=EDGE_CURVE('',#17632,#17287,#7058,.T.);
#21379=EDGE_CURVE('',#17633,#17286,#7059,.T.);
#21380=EDGE_CURVE('',#17633,#17632,#16682,.T.);
#21381=EDGE_CURVE('',#17634,#17283,#7060,.T.);
#21382=EDGE_CURVE('',#17635,#17282,#7061,.T.);
#21383=EDGE_CURVE('',#17635,#17634,#16683,.T.);
#21384=EDGE_CURVE('',#17636,#17279,#7062,.T.);
#21385=EDGE_CURVE('',#17637,#17278,#7063,.T.);
#21386=EDGE_CURVE('',#17637,#17636,#16684,.T.);
#21387=EDGE_CURVE('',#17638,#17255,#7064,.T.);
#21388=EDGE_CURVE('',#17639,#17254,#7065,.T.);
#21389=EDGE_CURVE('',#17639,#17638,#16685,.T.);
#21390=EDGE_CURVE('',#17246,#17640,#7066,.T.);
#21391=EDGE_CURVE('',#17640,#17641,#16686,.T.);
#21392=EDGE_CURVE('',#17247,#17641,#7067,.T.);
#21393=EDGE_CURVE('',#17242,#17642,#7068,.T.);
#21394=EDGE_CURVE('',#17642,#17643,#16687,.T.);
#21395=EDGE_CURVE('',#17243,#17643,#7069,.T.);
#21396=EDGE_CURVE('',#17234,#17644,#7070,.T.);
#21397=EDGE_CURVE('',#17644,#17645,#16688,.T.);
#21398=EDGE_CURVE('',#17235,#17645,#7071,.T.);
#21399=EDGE_CURVE('',#17222,#17646,#7072,.T.);
#21400=EDGE_CURVE('',#17646,#17647,#16689,.T.);
#21401=EDGE_CURVE('',#17223,#17647,#7073,.T.);
#21402=EDGE_CURVE('',#17218,#17648,#7074,.T.);
#21403=EDGE_CURVE('',#17648,#17649,#16690,.T.);
#21404=EDGE_CURVE('',#17219,#17649,#7075,.T.);
#21405=EDGE_CURVE('',#17214,#17650,#7076,.T.);
#21406=EDGE_CURVE('',#17650,#17651,#16691,.T.);
#21407=EDGE_CURVE('',#17215,#17651,#7077,.T.);
#21408=EDGE_CURVE('',#17210,#17652,#7078,.T.);
#21409=EDGE_CURVE('',#17652,#17653,#16692,.T.);
#21410=EDGE_CURVE('',#17211,#17653,#7079,.T.);
#21411=EDGE_CURVE('',#17178,#17654,#7080,.T.);
#21412=EDGE_CURVE('',#17654,#17655,#16693,.T.);
#21413=EDGE_CURVE('',#17179,#17655,#7081,.T.);
#21414=EDGE_CURVE('',#17174,#17656,#7082,.T.);
#21415=EDGE_CURVE('',#17656,#17657,#16694,.T.);
#21416=EDGE_CURVE('',#17175,#17657,#7083,.T.);
#21417=EDGE_CURVE('',#17170,#17658,#7084,.T.);
#21418=EDGE_CURVE('',#17658,#17659,#16695,.T.);
#21419=EDGE_CURVE('',#17171,#17659,#7085,.T.);
#21420=EDGE_CURVE('',#17166,#17660,#7086,.T.);
#21421=EDGE_CURVE('',#17660,#17661,#16696,.T.);
#21422=EDGE_CURVE('',#17167,#17661,#7087,.T.);
#21423=EDGE_CURVE('',#17162,#17662,#7088,.T.);
#21424=EDGE_CURVE('',#17662,#17663,#16697,.T.);
#21425=EDGE_CURVE('',#17163,#17663,#7089,.T.);
#21426=EDGE_CURVE('',#17664,#17158,#7090,.T.);
#21427=EDGE_CURVE('',#17665,#17664,#16698,.T.);
#21428=EDGE_CURVE('',#17665,#17159,#7091,.T.);
#21429=EDGE_CURVE('',#17666,#17182,#7092,.T.);
#21430=EDGE_CURVE('',#17667,#17666,#16699,.T.);
#21431=EDGE_CURVE('',#17667,#17183,#7093,.T.);
#21432=EDGE_CURVE('',#17668,#17186,#7094,.T.);
#21433=EDGE_CURVE('',#17669,#17668,#16700,.T.);
#21434=EDGE_CURVE('',#17669,#17187,#7095,.T.);
#21435=EDGE_CURVE('',#17670,#17190,#7096,.T.);
#21436=EDGE_CURVE('',#17671,#17670,#16701,.T.);
#21437=EDGE_CURVE('',#17671,#17191,#7097,.T.);
#21438=EDGE_CURVE('',#17672,#17194,#7098,.T.);
#21439=EDGE_CURVE('',#17673,#17672,#16702,.T.);
#21440=EDGE_CURVE('',#17673,#17195,#7099,.T.);
#21441=EDGE_CURVE('',#17674,#17198,#7100,.T.);
#21442=EDGE_CURVE('',#17675,#17674,#16703,.T.);
#21443=EDGE_CURVE('',#17675,#17199,#7101,.T.);
#21444=EDGE_CURVE('',#17676,#17202,#7102,.T.);
#21445=EDGE_CURVE('',#17677,#17676,#16704,.T.);
#21446=EDGE_CURVE('',#17677,#17203,#7103,.T.);
#21447=EDGE_CURVE('',#17678,#17206,#7104,.T.);
#21448=EDGE_CURVE('',#17679,#17678,#16705,.T.);
#21449=EDGE_CURVE('',#17679,#17207,#7105,.T.);
#21450=EDGE_CURVE('',#17680,#17226,#7106,.T.);
#21451=EDGE_CURVE('',#17681,#17680,#16706,.T.);
#21452=EDGE_CURVE('',#17681,#17227,#7107,.T.);
#21453=EDGE_CURVE('',#17682,#17230,#7108,.T.);
#21454=EDGE_CURVE('',#17683,#17682,#16707,.T.);
#21455=EDGE_CURVE('',#17683,#17231,#7109,.T.);
#21456=EDGE_CURVE('',#17684,#17238,#7110,.T.);
#21457=EDGE_CURVE('',#17685,#17684,#16708,.T.);
#21458=EDGE_CURVE('',#17685,#17239,#7111,.T.);
#21459=EDGE_CURVE('',#17686,#17250,#7112,.T.);
#21460=EDGE_CURVE('',#17687,#17686,#16709,.T.);
#21461=EDGE_CURVE('',#17687,#17251,#7113,.T.);
#21462=EDGE_CURVE('',#17259,#17688,#7114,.T.);
#21463=EDGE_CURVE('',#17258,#17689,#7115,.T.);
#21464=EDGE_CURVE('',#17688,#17689,#16710,.T.);
#21465=EDGE_CURVE('',#17263,#17690,#7116,.T.);
#21466=EDGE_CURVE('',#17262,#17691,#7117,.T.);
#21467=EDGE_CURVE('',#17690,#17691,#16711,.T.);
#21468=EDGE_CURVE('',#17267,#17692,#7118,.T.);
#21469=EDGE_CURVE('',#17266,#17693,#7119,.T.);
#21470=EDGE_CURVE('',#17692,#17693,#16712,.T.);
#21471=EDGE_CURVE('',#17271,#17694,#7120,.T.);
#21472=EDGE_CURVE('',#17270,#17695,#7121,.T.);
#21473=EDGE_CURVE('',#17694,#17695,#16713,.T.);
#21474=EDGE_CURVE('',#17275,#17696,#7122,.T.);
#21475=EDGE_CURVE('',#17274,#17697,#7123,.T.);
#21476=EDGE_CURVE('',#17696,#17697,#16714,.T.);
#21477=EDGE_CURVE('',#17307,#17698,#7124,.T.);
#21478=EDGE_CURVE('',#17306,#17699,#7125,.T.);
#21479=EDGE_CURVE('',#17698,#17699,#16715,.T.);
#21480=EDGE_CURVE('',#17311,#17700,#7126,.T.);
#21481=EDGE_CURVE('',#17310,#17701,#7127,.T.);
#21482=EDGE_CURVE('',#17700,#17701,#16716,.T.);
#21483=EDGE_CURVE('',#17315,#17702,#7128,.T.);
#21484=EDGE_CURVE('',#17314,#17703,#7129,.T.);
#21485=EDGE_CURVE('',#17702,#17703,#16717,.T.);
#21486=EDGE_CURVE('',#17319,#17704,#7130,.T.);
#21487=EDGE_CURVE('',#17318,#17705,#7131,.T.);
#21488=EDGE_CURVE('',#17704,#17705,#16718,.T.);
#21489=EDGE_CURVE('',#17331,#17706,#7132,.T.);
#21490=EDGE_CURVE('',#17330,#17707,#7133,.T.);
#21491=EDGE_CURVE('',#17706,#17707,#16719,.T.);
#21492=EDGE_CURVE('',#17339,#17708,#7134,.T.);
#21493=EDGE_CURVE('',#17338,#17709,#7135,.T.);
#21494=EDGE_CURVE('',#17708,#17709,#16720,.T.);
#21495=EDGE_CURVE('',#17343,#17710,#7136,.T.);
#21496=EDGE_CURVE('',#17342,#17711,#7137,.T.);
#21497=EDGE_CURVE('',#17710,#17711,#16721,.T.);
#21498=EDGE_CURVE('',#17712,#17713,#7138,.T.);
#21499=EDGE_CURVE('',#17713,#17714,#7139,.T.);
#21500=EDGE_CURVE('',#17714,#17715,#7140,.T.);
#21501=EDGE_CURVE('',#17716,#17715,#7141,.T.);
#21502=EDGE_CURVE('',#17716,#17717,#16722,.T.);
#21503=EDGE_CURVE('',#17718,#17717,#7142,.T.);
#21504=EDGE_CURVE('',#17719,#17718,#16723,.T.);
#21505=EDGE_CURVE('',#17720,#17719,#7143,.T.);
#21506=EDGE_CURVE('',#17721,#17720,#7144,.T.);
#21507=EDGE_CURVE('',#17721,#17712,#7145,.T.);
#21508=EDGE_CURVE('',#17341,#17722,#7146,.T.);
#21509=EDGE_CURVE('',#17722,#17723,#16724,.T.);
#21510=EDGE_CURVE('',#17340,#17723,#7147,.T.);
#21511=EDGE_CURVE('',#17337,#17724,#7148,.T.);
#21512=EDGE_CURVE('',#17724,#17725,#16725,.T.);
#21513=EDGE_CURVE('',#17336,#17725,#7149,.T.);
#21514=EDGE_CURVE('',#17726,#17332,#7150,.T.);
#21515=EDGE_CURVE('',#17727,#17726,#16726,.T.);
#21516=EDGE_CURVE('',#17727,#17333,#7151,.T.);
#21517=EDGE_CURVE('',#17728,#17320,#7152,.T.);
#21518=EDGE_CURVE('',#17729,#17728,#16727,.T.);
#21519=EDGE_CURVE('',#17729,#17321,#7153,.T.);
#21520=EDGE_CURVE('',#17730,#17296,#7154,.T.);
#21521=EDGE_CURVE('',#17731,#17730,#16728,.T.);
#21522=EDGE_CURVE('',#17731,#17297,#7155,.T.);
#21523=EDGE_CURVE('',#17732,#17288,#7156,.T.);
#21524=EDGE_CURVE('',#17733,#17732,#16729,.T.);
#21525=EDGE_CURVE('',#17733,#17289,#7157,.T.);
#21526=EDGE_CURVE('',#17734,#17280,#7158,.T.);
#21527=EDGE_CURVE('',#17735,#17734,#16730,.T.);
#21528=EDGE_CURVE('',#17735,#17281,#7159,.T.);
#21529=EDGE_CURVE('',#17273,#17736,#7160,.T.);
#21530=EDGE_CURVE('',#17736,#17737,#16731,.T.);
#21531=EDGE_CURVE('',#17272,#17737,#7161,.T.);
#21532=EDGE_CURVE('',#17269,#17738,#7162,.T.);
#21533=EDGE_CURVE('',#17738,#17739,#16732,.T.);
#21534=EDGE_CURVE('',#17268,#17739,#7163,.T.);
#21535=EDGE_CURVE('',#17265,#17740,#7164,.T.);
#21536=EDGE_CURVE('',#17740,#17741,#16733,.T.);
#21537=EDGE_CURVE('',#17264,#17741,#7165,.T.);
#21538=EDGE_CURVE('',#17261,#17742,#7166,.T.);
#21539=EDGE_CURVE('',#17742,#17743,#16734,.T.);
#21540=EDGE_CURVE('',#17260,#17743,#7167,.T.);
#21541=EDGE_CURVE('',#17257,#17744,#7168,.T.);
#21542=EDGE_CURVE('',#17744,#17745,#16735,.T.);
#21543=EDGE_CURVE('',#17256,#17745,#7169,.T.);
#21544=EDGE_CURVE('',#17746,#17252,#7170,.T.);
#21545=EDGE_CURVE('',#17747,#17746,#16736,.T.);
#21546=EDGE_CURVE('',#17747,#17253,#7171,.T.);
#21547=EDGE_CURVE('',#17241,#17748,#7172,.T.);
#21548=EDGE_CURVE('',#17240,#17749,#7173,.T.);
#21549=EDGE_CURVE('',#17748,#17749,#16737,.T.);
#21550=EDGE_CURVE('',#17750,#17228,#7174,.T.);
#21551=EDGE_CURVE('',#17751,#17229,#7175,.T.);
#21552=EDGE_CURVE('',#17751,#17750,#16738,.T.);
#21553=EDGE_CURVE('',#17752,#17224,#7176,.T.);
#21554=EDGE_CURVE('',#17753,#17225,#7177,.T.);
#21555=EDGE_CURVE('',#17753,#17752,#16739,.T.);
#21556=EDGE_CURVE('',#17221,#17754,#7178,.T.);
#21557=EDGE_CURVE('',#17220,#17755,#7179,.T.);
#21558=EDGE_CURVE('',#17754,#17755,#16740,.T.);
#21559=EDGE_CURVE('',#17213,#17756,#7180,.T.);
#21560=EDGE_CURVE('',#17212,#17757,#7181,.T.);
#21561=EDGE_CURVE('',#17756,#17757,#16741,.T.);
#21562=EDGE_CURVE('',#17758,#17204,#7182,.T.);
#21563=EDGE_CURVE('',#17759,#17205,#7183,.T.);
#21564=EDGE_CURVE('',#17759,#17758,#16742,.T.);
#21565=EDGE_CURVE('',#17760,#17200,#7184,.T.);
#21566=EDGE_CURVE('',#17761,#17201,#7185,.T.);
#21567=EDGE_CURVE('',#17761,#17760,#16743,.T.);
#21568=EDGE_CURVE('',#17762,#17196,#7186,.T.);
#21569=EDGE_CURVE('',#17763,#17197,#7187,.T.);
#21570=EDGE_CURVE('',#17763,#17762,#16744,.T.);
#21571=EDGE_CURVE('',#17764,#17192,#7188,.T.);
#21572=EDGE_CURVE('',#17765,#17193,#7189,.T.);
#21573=EDGE_CURVE('',#17765,#17764,#16745,.T.);
#21574=EDGE_CURVE('',#17766,#17188,#7190,.T.);
#21575=EDGE_CURVE('',#17767,#17189,#7191,.T.);
#21576=EDGE_CURVE('',#17767,#17766,#16746,.T.);
#21577=EDGE_CURVE('',#17768,#17184,#7192,.T.);
#21578=EDGE_CURVE('',#17769,#17185,#7193,.T.);
#21579=EDGE_CURVE('',#17769,#17768,#16747,.T.);
#21580=EDGE_CURVE('',#17770,#17180,#7194,.T.);
#21581=EDGE_CURVE('',#17771,#17181,#7195,.T.);
#21582=EDGE_CURVE('',#17771,#17770,#16748,.T.);
#21583=EDGE_CURVE('',#17177,#17772,#7196,.T.);
#21584=EDGE_CURVE('',#17176,#17773,#7197,.T.);
#21585=EDGE_CURVE('',#17772,#17773,#16749,.T.);
#21586=EDGE_CURVE('',#17169,#17774,#7198,.T.);
#21587=EDGE_CURVE('',#17168,#17775,#7199,.T.);
#21588=EDGE_CURVE('',#17774,#17775,#16750,.T.);
#21589=EDGE_CURVE('',#17161,#17776,#7200,.T.);
#21590=EDGE_CURVE('',#17160,#17777,#7201,.T.);
#21591=EDGE_CURVE('',#17776,#17777,#16751,.T.);
#21592=EDGE_CURVE('',#17778,#17156,#7202,.T.);
#21593=EDGE_CURVE('',#17779,#17157,#7203,.T.);
#21594=EDGE_CURVE('',#17779,#17778,#16752,.T.);
#21595=EDGE_CURVE('',#17165,#17780,#7204,.T.);
#21596=EDGE_CURVE('',#17164,#17781,#7205,.T.);
#21597=EDGE_CURVE('',#17780,#17781,#16753,.T.);
#21598=EDGE_CURVE('',#17173,#17782,#7206,.T.);
#21599=EDGE_CURVE('',#17172,#17783,#7207,.T.);
#21600=EDGE_CURVE('',#17782,#17783,#16754,.T.);
#21601=EDGE_CURVE('',#17209,#17784,#7208,.T.);
#21602=EDGE_CURVE('',#17208,#17785,#7209,.T.);
#21603=EDGE_CURVE('',#17784,#17785,#16755,.T.);
#21604=EDGE_CURVE('',#17217,#17786,#7210,.T.);
#21605=EDGE_CURVE('',#17216,#17787,#7211,.T.);
#21606=EDGE_CURVE('',#17786,#17787,#16756,.T.);
#21607=EDGE_CURVE('',#17233,#17788,#7212,.T.);
#21608=EDGE_CURVE('',#17232,#17789,#7213,.T.);
#21609=EDGE_CURVE('',#17788,#17789,#16757,.T.);
#21610=EDGE_CURVE('',#17790,#17236,#7214,.T.);
#21611=EDGE_CURVE('',#17791,#17237,#7215,.T.);
#21612=EDGE_CURVE('',#17791,#17790,#16758,.T.);
#21613=EDGE_CURVE('',#17245,#17792,#7216,.T.);
#21614=EDGE_CURVE('',#17244,#17793,#7217,.T.);
#21615=EDGE_CURVE('',#17792,#17793,#16759,.T.);
#21616=EDGE_CURVE('',#17794,#17248,#7218,.T.);
#21617=EDGE_CURVE('',#17795,#17249,#7219,.T.);
#21618=EDGE_CURVE('',#17795,#17794,#16760,.T.);
#21619=EDGE_CURVE('',#17796,#17276,#7220,.T.);
#21620=EDGE_CURVE('',#17797,#17796,#16761,.T.);
#21621=EDGE_CURVE('',#17797,#17277,#7221,.T.);
#21622=EDGE_CURVE('',#17798,#17284,#7222,.T.);
#21623=EDGE_CURVE('',#17799,#17798,#16762,.T.);
#21624=EDGE_CURVE('',#17799,#17285,#7223,.T.);
#21625=EDGE_CURVE('',#17800,#17292,#7224,.T.);
#21626=EDGE_CURVE('',#17801,#17800,#16763,.T.);
#21627=EDGE_CURVE('',#17801,#17293,#7225,.T.);
#21628=EDGE_CURVE('',#17802,#17300,#7226,.T.);
#21629=EDGE_CURVE('',#17803,#17802,#16764,.T.);
#21630=EDGE_CURVE('',#17803,#17301,#7227,.T.);
#21631=EDGE_CURVE('',#17305,#17804,#7228,.T.);
#21632=EDGE_CURVE('',#17804,#17805,#16765,.T.);
#21633=EDGE_CURVE('',#17304,#17805,#7229,.T.);
#21634=EDGE_CURVE('',#17309,#17806,#7230,.T.);
#21635=EDGE_CURVE('',#17806,#17807,#16766,.T.);
#21636=EDGE_CURVE('',#17308,#17807,#7231,.T.);
#21637=EDGE_CURVE('',#17313,#17808,#7232,.T.);
#21638=EDGE_CURVE('',#17808,#17809,#16767,.T.);
#21639=EDGE_CURVE('',#17312,#17809,#7233,.T.);
#21640=EDGE_CURVE('',#17317,#17810,#7234,.T.);
#21641=EDGE_CURVE('',#17810,#17811,#16768,.T.);
#21642=EDGE_CURVE('',#17316,#17811,#7235,.T.);
#21643=EDGE_CURVE('',#17812,#17324,#7236,.T.);
#21644=EDGE_CURVE('',#17813,#17812,#16769,.T.);
#21645=EDGE_CURVE('',#17813,#17325,#7237,.T.);
#21646=EDGE_CURVE('',#17329,#17814,#7238,.T.);
#21647=EDGE_CURVE('',#17814,#17815,#16770,.T.);
#21648=EDGE_CURVE('',#17328,#17815,#7239,.T.);
#21649=EDGE_CURVE('',#17816,#17344,#7240,.T.);
#21650=EDGE_CURVE('',#17817,#17816,#16771,.T.);
#21651=EDGE_CURVE('',#17817,#17345,#7241,.T.);
#21652=EDGE_CURVE('',#17394,#17818,#7242,.T.);
#21653=EDGE_CURVE('',#17819,#17392,#7243,.T.);
#21654=EDGE_CURVE('',#17819,#17818,#7244,.T.);
#21655=EDGE_CURVE('',#17820,#17376,#7245,.T.);
#21656=EDGE_CURVE('',#17820,#17821,#7246,.T.);
#21657=EDGE_CURVE('',#17378,#17821,#7247,.T.);
#21658=EDGE_CURVE('',#17822,#17823,#7248,.T.);
#21659=EDGE_CURVE('',#17822,#17824,#7249,.T.);
#21660=EDGE_CURVE('',#17825,#17824,#7250,.T.);
#21661=EDGE_CURVE('',#17825,#17823,#7251,.T.);
#21662=EDGE_CURVE('',#17389,#17826,#7252,.T.);
#21663=EDGE_CURVE('',#17827,#17391,#7253,.T.);
#21664=EDGE_CURVE('',#17827,#17826,#7254,.T.);
#21665=EDGE_CURVE('',#17828,#17829,#7255,.T.);
#21666=EDGE_CURVE('',#17828,#17830,#7256,.T.);
#21667=EDGE_CURVE('',#17831,#17830,#7257,.T.);
#21668=EDGE_CURVE('',#17831,#17829,#7258,.T.);
#21669=EDGE_CURVE('',#17385,#17832,#7259,.T.);
#21670=EDGE_CURVE('',#17833,#17387,#7260,.T.);
#21671=EDGE_CURVE('',#17833,#17832,#7261,.T.);
#21672=EDGE_CURVE('',#17382,#17834,#7262,.T.);
#21673=EDGE_CURVE('',#17835,#17380,#7263,.T.);
#21674=EDGE_CURVE('',#17835,#17834,#7264,.T.);
#21675=EDGE_CURVE('',#17836,#17837,#7265,.T.);
#21676=EDGE_CURVE('',#17836,#17838,#7266,.T.);
#21677=EDGE_CURVE('',#17839,#17838,#7267,.T.);
#21678=EDGE_CURVE('',#17839,#17837,#7268,.T.);
#21679=EDGE_CURVE('',#17840,#17841,#7269,.T.);
#21680=EDGE_CURVE('',#17840,#17842,#7270,.T.);
#21681=EDGE_CURVE('',#17843,#17842,#7271,.T.);
#21682=EDGE_CURVE('',#17843,#17841,#7272,.T.);
#21683=EDGE_CURVE('',#17844,#17375,#7273,.T.);
#21684=EDGE_CURVE('',#17844,#17845,#7274,.T.);
#21685=EDGE_CURVE('',#17373,#17845,#7275,.T.);
#21686=EDGE_CURVE('',#17846,#17847,#7276,.T.);
#21687=EDGE_CURVE('',#17846,#17848,#7277,.T.);
#21688=EDGE_CURVE('',#17849,#17848,#7278,.T.);
#21689=EDGE_CURVE('',#17849,#17847,#7279,.T.);
#21690=EDGE_CURVE('',#17850,#17851,#7280,.T.);
#21691=EDGE_CURVE('',#17850,#17852,#7281,.T.);
#21692=EDGE_CURVE('',#17853,#17852,#7282,.T.);
#21693=EDGE_CURVE('',#17853,#17851,#7283,.T.);
#21694=EDGE_CURVE('',#17406,#17854,#7284,.T.);
#21695=EDGE_CURVE('',#17855,#17404,#7285,.T.);
#21696=EDGE_CURVE('',#17855,#17854,#7286,.T.);
#21697=EDGE_CURVE('',#17856,#17400,#7287,.T.);
#21698=EDGE_CURVE('',#17856,#17857,#7288,.T.);
#21699=EDGE_CURVE('',#17402,#17857,#7289,.T.);
#21700=EDGE_CURVE('',#17858,#17859,#7290,.T.);
#21701=EDGE_CURVE('',#17858,#17860,#7291,.T.);
#21702=EDGE_CURVE('',#17861,#17860,#7292,.T.);
#21703=EDGE_CURVE('',#17861,#17859,#7293,.T.);
#21704=EDGE_CURVE('',#17417,#17862,#7294,.T.);
#21705=EDGE_CURVE('',#17863,#17419,#7295,.T.);
#21706=EDGE_CURVE('',#17863,#17862,#7296,.T.);
#21707=EDGE_CURVE('',#17864,#17865,#7297,.T.);
#21708=EDGE_CURVE('',#17864,#17866,#7298,.T.);
#21709=EDGE_CURVE('',#17867,#17866,#7299,.T.);
#21710=EDGE_CURVE('',#17867,#17865,#7300,.T.);
#21711=EDGE_CURVE('',#17413,#17868,#7301,.T.);
#21712=EDGE_CURVE('',#17869,#17415,#7302,.T.);
#21713=EDGE_CURVE('',#17869,#17868,#7303,.T.);
#21714=EDGE_CURVE('',#17410,#17870,#7304,.T.);
#21715=EDGE_CURVE('',#17871,#17408,#7305,.T.);
#21716=EDGE_CURVE('',#17871,#17870,#7306,.T.);
#21717=EDGE_CURVE('',#17872,#17873,#7307,.T.);
#21718=EDGE_CURVE('',#17872,#17874,#7308,.T.);
#21719=EDGE_CURVE('',#17875,#17874,#7309,.T.);
#21720=EDGE_CURVE('',#17875,#17873,#7310,.T.);
#21721=EDGE_CURVE('',#17876,#17877,#7311,.T.);
#21722=EDGE_CURVE('',#17876,#17878,#7312,.T.);
#21723=EDGE_CURVE('',#17879,#17878,#7313,.T.);
#21724=EDGE_CURVE('',#17879,#17877,#7314,.T.);
#21725=EDGE_CURVE('',#17880,#17399,#7315,.T.);
#21726=EDGE_CURVE('',#17880,#17881,#7316,.T.);
#21727=EDGE_CURVE('',#17397,#17881,#7317,.T.);
#21728=EDGE_CURVE('',#17882,#17883,#7318,.T.);
#21729=EDGE_CURVE('',#17882,#17884,#7319,.T.);
#21730=EDGE_CURVE('',#17885,#17884,#7320,.T.);
#21731=EDGE_CURVE('',#17885,#17883,#7321,.T.);
#21732=EDGE_CURVE('',#17886,#17887,#7322,.T.);
#21733=EDGE_CURVE('',#17886,#17888,#7323,.T.);
#21734=EDGE_CURVE('',#17889,#17888,#7324,.T.);
#21735=EDGE_CURVE('',#17889,#17887,#7325,.T.);
#21736=EDGE_CURVE('',#17890,#17891,#2205,.T.);
#21737=EDGE_CURVE('',#17891,#17892,#7326,.T.);
#21738=EDGE_CURVE('',#17893,#17892,#2206,.T.);
#21739=EDGE_CURVE('',#17893,#17890,#7327,.T.);
#21740=EDGE_CURVE('',#17436,#17840,#16772,.T.);
#21741=EDGE_CURVE('',#17841,#17894,#16773,.T.);
#21742=EDGE_CURVE('',#17894,#17424,#2207,.T.);
#21743=EDGE_CURVE('',#17425,#17819,#16774,.T.);
#21744=EDGE_CURVE('',#17437,#17393,#2208,.T.);
#21745=EDGE_CURVE('',#17428,#17895,#16775,.T.);
#21746=EDGE_CURVE('',#17895,#17896,#7328,.T.);
#21747=EDGE_CURVE('',#17896,#17897,#16776,.T.);
#21748=EDGE_CURVE('',#17897,#17420,#2209,.T.);
#21749=EDGE_CURVE('',#17421,#17898,#16777,.T.);
#21750=EDGE_CURVE('',#17898,#17368,#7329,.T.);
#21751=EDGE_CURVE('',#17429,#17369,#2210,.T.);
#21752=EDGE_CURVE('',#17899,#17900,#7330,.T.);
#21753=EDGE_CURVE('',#17900,#17901,#16778,.T.);
#21754=EDGE_CURVE('',#17901,#17348,#2211,.T.);
#21755=EDGE_CURVE('',#17349,#17902,#7331,.T.);
#21756=EDGE_CURVE('',#17902,#17903,#16779,.T.);
#21757=EDGE_CURVE('',#17904,#17903,#2212,.T.);
#21758=EDGE_CURVE('',#17904,#17899,#16780,.T.);
#21759=EDGE_CURVE('',#17905,#17352,#7332,.T.);
#21760=EDGE_CURVE('',#17353,#17906,#2213,.T.);
#21761=EDGE_CURVE('',#17906,#17907,#16781,.T.);
#21762=EDGE_CURVE('',#17907,#17908,#7333,.T.);
#21763=EDGE_CURVE('',#17908,#17909,#16782,.T.);
#21764=EDGE_CURVE('',#17910,#17909,#2214,.T.);
#21765=EDGE_CURVE('',#17910,#17905,#16783,.T.);
#21766=EDGE_CURVE('',#17365,#17911,#7334,.T.);
#21767=EDGE_CURVE('',#17911,#17912,#16784,.T.);
#21768=EDGE_CURVE('',#17912,#17913,#2215,.T.);
#21769=EDGE_CURVE('',#17913,#17914,#16785,.T.);
#21770=EDGE_CURVE('',#17914,#17915,#7335,.T.);
#21771=EDGE_CURVE('',#17915,#17916,#16786,.T.);
#21772=EDGE_CURVE('',#17364,#17916,#2216,.T.);
#21773=EDGE_CURVE('',#17361,#17917,#7336,.T.);
#21774=EDGE_CURVE('',#17917,#17918,#16787,.T.);
#21775=EDGE_CURVE('',#17918,#17919,#2217,.T.);
#21776=EDGE_CURVE('',#17919,#17920,#16788,.T.);
#21777=EDGE_CURVE('',#17920,#17921,#7337,.T.);
#21778=EDGE_CURVE('',#17921,#17922,#16789,.T.);
#21779=EDGE_CURVE('',#17360,#17922,#2218,.T.);
#21780=EDGE_CURVE('',#17923,#17924,#7338,.T.);
#21781=EDGE_CURVE('',#17924,#17925,#16790,.T.);
#21782=EDGE_CURVE('',#17925,#17926,#2219,.T.);
#21783=EDGE_CURVE('',#17926,#17927,#16791,.T.);
#21784=EDGE_CURVE('',#17927,#17356,#7339,.T.);
#21785=EDGE_CURVE('',#17928,#17357,#2220,.T.);
#21786=EDGE_CURVE('',#17928,#17923,#16792,.T.);
#21787=EDGE_CURVE('',#17847,#17929,#16793,.T.);
#21788=EDGE_CURVE('',#17929,#17372,#2221,.T.);
#21789=EDGE_CURVE('',#17845,#17930,#16794,.T.);
#21790=EDGE_CURVE('',#17931,#17930,#2222,.T.);
#21791=EDGE_CURVE('',#17931,#17846,#16795,.T.);
#21792=EDGE_CURVE('',#17377,#17932,#2223,.T.);
#21793=EDGE_CURVE('',#17932,#17850,#16796,.T.);
#21794=EDGE_CURVE('',#17851,#17933,#16797,.T.);
#21795=EDGE_CURVE('',#17934,#17933,#2224,.T.);
#21796=EDGE_CURVE('',#17934,#17820,#16798,.T.);
#21797=EDGE_CURVE('',#17826,#17935,#16799,.T.);
#21798=EDGE_CURVE('',#17935,#17936,#2225,.T.);
#21799=EDGE_CURVE('',#17936,#17825,#16800,.T.);
#21800=EDGE_CURVE('',#17824,#17937,#16801,.T.);
#21801=EDGE_CURVE('',#17388,#17937,#2226,.T.);
#21802=EDGE_CURVE('',#17832,#17938,#16802,.T.);
#21803=EDGE_CURVE('',#17938,#17939,#2227,.T.);
#21804=EDGE_CURVE('',#17939,#17831,#16803,.T.);
#21805=EDGE_CURVE('',#17830,#17940,#16804,.T.);
#21806=EDGE_CURVE('',#17384,#17940,#2228,.T.);
#21807=EDGE_CURVE('',#17837,#17941,#16805,.T.);
#21808=EDGE_CURVE('',#17941,#17942,#2229,.T.);
#21809=EDGE_CURVE('',#17942,#17835,#16806,.T.);
#21810=EDGE_CURVE('',#17943,#17381,#2230,.T.);
#21811=EDGE_CURVE('',#17943,#17836,#16807,.T.);
#21812=EDGE_CURVE('',#17883,#17944,#16808,.T.);
#21813=EDGE_CURVE('',#17944,#17396,#2231,.T.);
#21814=EDGE_CURVE('',#17881,#17891,#16809,.T.);
#21815=EDGE_CURVE('',#17890,#17882,#16810,.T.);
#21816=EDGE_CURVE('',#17401,#17945,#2232,.T.);
#21817=EDGE_CURVE('',#17945,#17886,#16811,.T.);
#21818=EDGE_CURVE('',#17887,#17946,#16812,.T.);
#21819=EDGE_CURVE('',#17947,#17946,#2233,.T.);
#21820=EDGE_CURVE('',#17947,#17856,#16813,.T.);
#21821=EDGE_CURVE('',#17862,#17948,#16814,.T.);
#21822=EDGE_CURVE('',#17948,#17949,#2234,.T.);
#21823=EDGE_CURVE('',#17949,#17861,#16815,.T.);
#21824=EDGE_CURVE('',#17860,#17950,#16816,.T.);
#21825=EDGE_CURVE('',#17416,#17950,#2235,.T.);
#21826=EDGE_CURVE('',#17868,#17951,#16817,.T.);
#21827=EDGE_CURVE('',#17951,#17952,#2236,.T.);
#21828=EDGE_CURVE('',#17952,#17867,#16818,.T.);
#21829=EDGE_CURVE('',#17866,#17953,#16819,.T.);
#21830=EDGE_CURVE('',#17412,#17953,#2237,.T.);
#21831=EDGE_CURVE('',#17873,#17954,#16820,.T.);
#21832=EDGE_CURVE('',#17954,#17955,#2238,.T.);
#21833=EDGE_CURVE('',#17955,#17871,#16821,.T.);
#21834=EDGE_CURVE('',#17956,#17409,#2239,.T.);
#21835=EDGE_CURVE('',#17956,#17872,#16822,.T.);
#21836=EDGE_CURVE('',#17462,#17876,#16823,.T.);
#21837=EDGE_CURVE('',#17877,#17957,#16824,.T.);
#21838=EDGE_CURVE('',#17957,#17432,#2240,.T.);
#21839=EDGE_CURVE('',#17433,#17855,#16825,.T.);
#21840=EDGE_CURVE('',#17463,#17405,#2241,.T.);
#21841=EDGE_CURVE('',#17464,#17407,#2242,.T.);
#21842=EDGE_CURVE('',#17370,#17958,#7340,.T.);
#21843=EDGE_CURVE('',#17898,#17958,#7341,.T.);
#21844=EDGE_CURVE('',#17959,#17411,#2243,.T.);
#21845=EDGE_CURVE('',#17959,#17956,#7342,.T.);
#21846=EDGE_CURVE('',#17953,#17960,#7343,.T.);
#21847=EDGE_CURVE('',#17414,#17960,#2244,.T.);
#21848=EDGE_CURVE('',#17950,#17961,#7344,.T.);
#21849=EDGE_CURVE('',#17418,#17961,#2245,.T.);
#21850=EDGE_CURVE('',#17962,#17963,#7345,.T.);
#21851=EDGE_CURVE('',#17963,#17964,#7346,.T.);
#21852=EDGE_CURVE('',#17965,#17964,#7347,.T.);
#21853=EDGE_CURVE('',#17966,#17965,#7348,.T.);
#21854=EDGE_CURVE('',#17967,#17966,#16826,.T.);
#21855=EDGE_CURVE('',#17968,#17967,#7349,.T.);
#21856=EDGE_CURVE('',#17969,#17968,#16827,.T.);
#21857=EDGE_CURVE('',#17970,#17969,#7350,.T.);
#21858=EDGE_CURVE('',#17970,#17971,#7351,.T.);
#21859=EDGE_CURVE('',#17971,#17962,#7352,.T.);
#21860=EDGE_CURVE('',#17972,#17973,#7353,.T.);
#21861=EDGE_CURVE('',#17974,#17972,#7354,.T.);
#21862=EDGE_CURVE('',#17975,#17974,#7355,.T.);
#21863=EDGE_CURVE('',#17973,#17975,#7356,.T.);
#21864=EDGE_CURVE('',#17976,#17977,#16828,.T.);
#21865=EDGE_CURVE('',#17978,#17976,#7357,.T.);
#21866=EDGE_CURVE('',#17979,#17978,#16829,.T.);
#21867=EDGE_CURVE('',#17980,#17979,#7358,.T.);
#21868=EDGE_CURVE('',#17981,#17980,#16830,.T.);
#21869=EDGE_CURVE('',#17982,#17981,#7359,.T.);
#21870=EDGE_CURVE('',#17983,#17982,#16831,.T.);
#21871=EDGE_CURVE('',#17984,#17983,#7360,.T.);
#21872=EDGE_CURVE('',#17985,#17984,#16832,.T.);
#21873=EDGE_CURVE('',#17986,#17985,#7361,.T.);
#21874=EDGE_CURVE('',#17987,#17986,#16833,.T.);
#21875=EDGE_CURVE('',#17977,#17987,#7362,.T.);
#21876=EDGE_CURVE('',#17988,#17989,#7363,.T.);
#21877=EDGE_CURVE('',#17989,#17990,#7364,.T.);
#21878=EDGE_CURVE('',#17991,#17990,#7365,.T.);
#21879=EDGE_CURVE('',#17991,#17992,#7366,.T.);
#21880=EDGE_CURVE('',#17993,#17992,#7367,.T.);
#21881=EDGE_CURVE('',#17994,#17993,#7368,.T.);
#21882=EDGE_CURVE('',#17994,#17995,#16834,.T.);
#21883=EDGE_CURVE('',#17995,#17996,#7369,.T.);
#21884=EDGE_CURVE('',#17997,#17996,#16835,.T.);
#21885=EDGE_CURVE('',#17988,#17997,#7370,.T.);
#21886=EDGE_CURVE('',#17998,#17999,#7371,.T.);
#21887=EDGE_CURVE('',#17999,#18000,#7372,.T.);
#21888=EDGE_CURVE('',#18000,#18001,#7373,.T.);
#21889=EDGE_CURVE('',#18001,#17998,#7374,.T.);
#21890=EDGE_CURVE('',#18002,#18003,#7375,.T.);
#21891=EDGE_CURVE('',#18003,#18004,#16836,.T.);
#21892=EDGE_CURVE('',#18004,#18005,#7376,.T.);
#21893=EDGE_CURVE('',#18005,#18006,#16837,.T.);
#21894=EDGE_CURVE('',#18006,#18007,#7377,.T.);
#21895=EDGE_CURVE('',#18007,#18008,#16838,.T.);
#21896=EDGE_CURVE('',#18008,#18009,#7378,.T.);
#21897=EDGE_CURVE('',#18009,#18010,#16839,.T.);
#21898=EDGE_CURVE('',#18010,#18011,#7379,.T.);
#21899=EDGE_CURVE('',#18011,#18012,#16840,.T.);
#21900=EDGE_CURVE('',#18012,#18013,#7380,.T.);
#21901=EDGE_CURVE('',#18013,#18002,#16841,.T.);
#21902=EDGE_CURVE('',#17484,#18014,#7381,.T.);
#21903=EDGE_CURVE('',#17539,#17483,#7382,.T.);
#21904=EDGE_CURVE('',#18014,#17538,#7383,.T.);
#21905=EDGE_CURVE('',#17537,#18015,#7384,.T.);
#21906=EDGE_CURVE('',#17536,#17486,#7385,.T.);
#21907=EDGE_CURVE('',#18015,#17485,#7386,.T.);
#21908=EDGE_CURVE('',#17470,#18016,#7387,.T.);
#21909=EDGE_CURVE('',#17553,#17469,#7388,.T.);
#21910=EDGE_CURVE('',#18016,#17552,#7389,.T.);
#21911=EDGE_CURVE('',#17551,#18017,#7390,.T.);
#21912=EDGE_CURVE('',#17550,#17472,#7391,.T.);
#21913=EDGE_CURVE('',#18017,#17471,#7392,.T.);
#21914=EDGE_CURVE('',#17471,#17995,#2246,.T.);
#21915=EDGE_CURVE('',#17995,#18018,#7393,.T.);
#21916=EDGE_CURVE('',#18018,#17968,#7394,.T.);
#21917=EDGE_CURVE('',#17551,#17968,#2247,.T.);
#21918=EDGE_CURVE('',#17967,#18019,#7395,.T.);
#21919=EDGE_CURVE('',#18019,#17996,#7396,.T.);
#21920=EDGE_CURVE('',#17996,#17470,#2248,.T.);
#21921=EDGE_CURVE('',#17967,#17552,#2249,.T.);
#21922=EDGE_CURVE('',#17965,#17988,#7397,.T.);
#21923=EDGE_CURVE('',#17966,#17997,#7398,.T.);
#21924=EDGE_CURVE('',#17964,#17989,#7399,.T.);
#21925=EDGE_CURVE('',#17990,#17963,#7400,.T.);
#21926=EDGE_CURVE('',#17962,#17991,#7401,.T.);
#21927=EDGE_CURVE('',#17992,#17971,#7402,.T.);
#21928=EDGE_CURVE('',#17993,#17970,#7403,.T.);
#21929=EDGE_CURVE('',#17969,#17994,#7404,.T.);
#21930=EDGE_CURVE('',#17613,#18020,#7405,.T.);
#21931=EDGE_CURVE('',#18020,#17718,#7406,.T.);
#21932=EDGE_CURVE('',#17718,#17484,#2250,.T.);
#21933=EDGE_CURVE('',#17613,#17538,#2251,.T.);
#21934=EDGE_CURVE('',#17485,#17717,#2252,.T.);
#21935=EDGE_CURVE('',#17717,#18021,#7407,.T.);
#21936=EDGE_CURVE('',#18021,#17614,#7408,.T.);
#21937=EDGE_CURVE('',#17537,#17614,#2253,.T.);
#21938=EDGE_CURVE('',#17720,#17611,#7409,.T.);
#21939=EDGE_CURVE('',#17612,#17719,#7410,.T.);
#21940=EDGE_CURVE('',#17610,#17721,#7411,.T.);
#21941=EDGE_CURVE('',#17608,#17713,#7412,.T.);
#21942=EDGE_CURVE('',#17712,#17609,#7413,.T.);
#21943=EDGE_CURVE('',#17714,#17606,#7414,.T.);
#21944=EDGE_CURVE('',#17715,#17607,#7415,.T.);
#21945=EDGE_CURVE('',#17615,#17716,#7416,.T.);
#21946=EDGE_CURVE('',#17554,#17507,#16842,.T.);
#21947=EDGE_CURVE('',#17508,#17555,#16843,.T.);
#21948=EDGE_CURVE('',#17557,#17502,#16844,.T.);
#21949=EDGE_CURVE('',#17504,#17556,#16845,.T.);
#21950=EDGE_CURVE('',#17507,#18022,#16846,.T.);
#21951=EDGE_CURVE('',#18022,#18023,#7417,.T.);
#21952=EDGE_CURVE('',#18023,#17504,#16847,.T.);
#21953=EDGE_CURVE('',#17502,#18024,#16848,.T.);
#21954=EDGE_CURVE('',#18024,#18025,#7418,.T.);
#21955=EDGE_CURVE('',#18025,#17508,#16849,.T.);
#21956=EDGE_CURVE('',#18026,#17505,#16850,.T.);
#21957=EDGE_CURVE('',#18027,#18023,#7419,.T.);
#21958=EDGE_CURVE('',#18028,#18027,#16851,.T.);
#21959=EDGE_CURVE('',#18029,#18028,#7420,.T.);
#21960=EDGE_CURVE('',#18030,#18029,#16852,.T.);
#21961=EDGE_CURVE('',#18024,#18030,#7421,.T.);
#21962=EDGE_CURVE('',#17503,#18031,#16853,.T.);
#21963=EDGE_CURVE('',#18031,#18032,#7422,.T.);
#21964=EDGE_CURVE('',#18032,#18033,#16854,.T.);
#21965=EDGE_CURVE('',#18033,#18034,#7423,.T.);
#21966=EDGE_CURVE('',#18034,#18035,#16855,.T.);
#21967=EDGE_CURVE('',#18035,#18026,#7424,.T.);
#21968=EDGE_CURVE('',#18036,#17509,#16856,.T.);
#21969=EDGE_CURVE('',#18025,#18037,#7425,.T.);
#21970=EDGE_CURVE('',#18038,#18037,#16857,.T.);
#21971=EDGE_CURVE('',#18038,#18039,#7426,.T.);
#21972=EDGE_CURVE('',#18040,#18039,#16858,.T.);
#21973=EDGE_CURVE('',#18040,#18022,#7427,.T.);
#21974=EDGE_CURVE('',#17506,#18041,#16859,.T.);
#21975=EDGE_CURVE('',#18042,#18041,#7428,.T.);
#21976=EDGE_CURVE('',#18042,#18043,#16860,.T.);
#21977=EDGE_CURVE('',#18044,#18043,#7429,.T.);
#21978=EDGE_CURVE('',#18044,#18045,#16861,.T.);
#21979=EDGE_CURVE('',#18036,#18045,#7430,.T.);
#21980=EDGE_CURVE('',#18039,#18028,#7431,.T.);
#21981=EDGE_CURVE('',#18027,#18040,#7432,.T.);
#21982=EDGE_CURVE('',#18037,#18030,#7433,.T.);
#21983=EDGE_CURVE('',#18029,#18038,#7434,.T.);
#21984=EDGE_CURVE('',#18035,#18042,#7435,.T.);
#21985=EDGE_CURVE('',#18043,#18034,#7436,.T.);
#21986=EDGE_CURVE('',#18033,#18044,#7437,.T.);
#21987=EDGE_CURVE('',#18045,#18032,#7438,.T.);
#21988=EDGE_CURVE('',#18031,#18036,#7439,.T.);
#21989=EDGE_CURVE('',#18041,#18026,#7440,.T.);
#21990=EDGE_CURVE('',#17558,#17515,#16862,.T.);
#21991=EDGE_CURVE('',#17516,#17559,#16863,.T.);
#21992=EDGE_CURVE('',#17561,#17510,#16864,.T.);
#21993=EDGE_CURVE('',#17512,#17560,#16865,.T.);
#21994=EDGE_CURVE('',#17515,#18046,#16866,.T.);
#21995=EDGE_CURVE('',#18046,#18047,#7441,.T.);
#21996=EDGE_CURVE('',#18047,#17512,#16867,.T.);
#21997=EDGE_CURVE('',#17510,#18048,#16868,.T.);
#21998=EDGE_CURVE('',#18048,#18049,#7442,.T.);
#21999=EDGE_CURVE('',#18049,#17516,#16869,.T.);
#22000=EDGE_CURVE('',#18050,#17513,#16870,.T.);
#22001=EDGE_CURVE('',#18051,#18047,#7443,.T.);
#22002=EDGE_CURVE('',#18052,#18051,#16871,.T.);
#22003=EDGE_CURVE('',#18053,#18052,#7444,.T.);
#22004=EDGE_CURVE('',#18054,#18053,#16872,.T.);
#22005=EDGE_CURVE('',#18048,#18054,#7445,.T.);
#22006=EDGE_CURVE('',#17511,#18055,#16873,.T.);
#22007=EDGE_CURVE('',#18055,#18056,#7446,.T.);
#22008=EDGE_CURVE('',#18056,#18057,#16874,.T.);
#22009=EDGE_CURVE('',#18057,#18058,#7447,.T.);
#22010=EDGE_CURVE('',#18058,#18059,#16875,.T.);
#22011=EDGE_CURVE('',#18059,#18050,#7448,.T.);
#22012=EDGE_CURVE('',#18060,#17517,#16876,.T.);
#22013=EDGE_CURVE('',#18049,#18061,#7449,.T.);
#22014=EDGE_CURVE('',#18062,#18061,#16877,.T.);
#22015=EDGE_CURVE('',#18062,#18063,#7450,.T.);
#22016=EDGE_CURVE('',#18064,#18063,#16878,.T.);
#22017=EDGE_CURVE('',#18064,#18046,#7451,.T.);
#22018=EDGE_CURVE('',#17514,#18065,#16879,.T.);
#22019=EDGE_CURVE('',#18066,#18065,#7452,.T.);
#22020=EDGE_CURVE('',#18066,#18067,#16880,.T.);
#22021=EDGE_CURVE('',#18068,#18067,#7453,.T.);
#22022=EDGE_CURVE('',#18068,#18069,#16881,.T.);
#22023=EDGE_CURVE('',#18060,#18069,#7454,.T.);
#22024=EDGE_CURVE('',#18063,#18052,#7455,.T.);
#22025=EDGE_CURVE('',#18051,#18064,#7456,.T.);
#22026=EDGE_CURVE('',#18061,#18054,#7457,.T.);
#22027=EDGE_CURVE('',#18053,#18062,#7458,.T.);
#22028=EDGE_CURVE('',#18059,#18066,#7459,.T.);
#22029=EDGE_CURVE('',#18067,#18058,#7460,.T.);
#22030=EDGE_CURVE('',#18057,#18068,#7461,.T.);
#22031=EDGE_CURVE('',#18069,#18056,#7462,.T.);
#22032=EDGE_CURVE('',#18055,#18060,#7463,.T.);
#22033=EDGE_CURVE('',#18065,#18050,#7464,.T.);
#22034=EDGE_CURVE('',#17562,#17499,#16882,.T.);
#22035=EDGE_CURVE('',#17500,#17563,#16883,.T.);
#22036=EDGE_CURVE('',#17565,#17494,#16884,.T.);
#22037=EDGE_CURVE('',#17496,#17564,#16885,.T.);
#22038=EDGE_CURVE('',#17499,#18070,#16886,.T.);
#22039=EDGE_CURVE('',#18070,#18071,#7465,.T.);
#22040=EDGE_CURVE('',#18071,#17496,#16887,.T.);
#22041=EDGE_CURVE('',#17494,#18072,#16888,.T.);
#22042=EDGE_CURVE('',#18072,#18073,#7466,.T.);
#22043=EDGE_CURVE('',#18073,#17500,#16889,.T.);
#22044=EDGE_CURVE('',#18074,#17497,#16890,.T.);
#22045=EDGE_CURVE('',#18075,#18071,#7467,.T.);
#22046=EDGE_CURVE('',#18076,#18075,#16891,.T.);
#22047=EDGE_CURVE('',#18077,#18076,#7468,.T.);
#22048=EDGE_CURVE('',#18078,#18077,#16892,.T.);
#22049=EDGE_CURVE('',#18072,#18078,#7469,.T.);
#22050=EDGE_CURVE('',#17495,#18079,#16893,.T.);
#22051=EDGE_CURVE('',#18079,#18080,#7470,.T.);
#22052=EDGE_CURVE('',#18080,#18081,#16894,.T.);
#22053=EDGE_CURVE('',#18081,#18082,#7471,.T.);
#22054=EDGE_CURVE('',#18082,#18083,#16895,.T.);
#22055=EDGE_CURVE('',#18083,#18074,#7472,.T.);
#22056=EDGE_CURVE('',#18084,#17501,#16896,.T.);
#22057=EDGE_CURVE('',#18073,#18085,#7473,.T.);
#22058=EDGE_CURVE('',#18086,#18085,#16897,.T.);
#22059=EDGE_CURVE('',#18086,#18087,#7474,.T.);
#22060=EDGE_CURVE('',#18088,#18087,#16898,.T.);
#22061=EDGE_CURVE('',#18088,#18070,#7475,.T.);
#22062=EDGE_CURVE('',#17498,#18089,#16899,.T.);
#22063=EDGE_CURVE('',#18090,#18089,#7476,.T.);
#22064=EDGE_CURVE('',#18090,#18091,#16900,.T.);
#22065=EDGE_CURVE('',#18092,#18091,#7477,.T.);
#22066=EDGE_CURVE('',#18092,#18093,#16901,.T.);
#22067=EDGE_CURVE('',#18084,#18093,#7478,.T.);
#22068=EDGE_CURVE('',#18087,#18076,#7479,.T.);
#22069=EDGE_CURVE('',#18075,#18088,#7480,.T.);
#22070=EDGE_CURVE('',#18085,#18078,#7481,.T.);
#22071=EDGE_CURVE('',#18077,#18086,#7482,.T.);
#22072=EDGE_CURVE('',#18083,#18090,#7483,.T.);
#22073=EDGE_CURVE('',#18091,#18082,#7484,.T.);
#22074=EDGE_CURVE('',#18081,#18092,#7485,.T.);
#22075=EDGE_CURVE('',#18093,#18080,#7486,.T.);
#22076=EDGE_CURVE('',#18079,#18084,#7487,.T.);
#22077=EDGE_CURVE('',#18089,#18074,#7488,.T.);
#22078=EDGE_CURVE('',#17566,#17523,#16902,.T.);
#22079=EDGE_CURVE('',#17524,#17567,#16903,.T.);
#22080=EDGE_CURVE('',#17569,#17518,#16904,.T.);
#22081=EDGE_CURVE('',#17520,#17568,#16905,.T.);
#22082=EDGE_CURVE('',#17523,#18094,#16906,.T.);
#22083=EDGE_CURVE('',#18094,#18095,#7489,.T.);
#22084=EDGE_CURVE('',#18095,#17520,#16907,.T.);
#22085=EDGE_CURVE('',#17518,#18096,#16908,.T.);
#22086=EDGE_CURVE('',#18096,#18097,#7490,.T.);
#22087=EDGE_CURVE('',#18097,#17524,#16909,.T.);
#22088=EDGE_CURVE('',#18098,#17521,#16910,.T.);
#22089=EDGE_CURVE('',#18099,#18095,#7491,.T.);
#22090=EDGE_CURVE('',#18100,#18099,#16911,.T.);
#22091=EDGE_CURVE('',#18101,#18100,#7492,.T.);
#22092=EDGE_CURVE('',#18102,#18101,#16912,.T.);
#22093=EDGE_CURVE('',#18096,#18102,#7493,.T.);
#22094=EDGE_CURVE('',#17519,#18103,#16913,.T.);
#22095=EDGE_CURVE('',#18103,#18104,#7494,.T.);
#22096=EDGE_CURVE('',#18104,#18105,#16914,.T.);
#22097=EDGE_CURVE('',#18105,#18106,#7495,.T.);
#22098=EDGE_CURVE('',#18106,#18107,#16915,.T.);
#22099=EDGE_CURVE('',#18107,#18098,#7496,.T.);
#22100=EDGE_CURVE('',#18108,#17525,#16916,.T.);
#22101=EDGE_CURVE('',#18097,#18109,#7497,.T.);
#22102=EDGE_CURVE('',#18110,#18109,#16917,.T.);
#22103=EDGE_CURVE('',#18110,#18111,#7498,.T.);
#22104=EDGE_CURVE('',#18112,#18111,#16918,.T.);
#22105=EDGE_CURVE('',#18112,#18094,#7499,.T.);
#22106=EDGE_CURVE('',#17522,#18113,#16919,.T.);
#22107=EDGE_CURVE('',#18114,#18113,#7500,.T.);
#22108=EDGE_CURVE('',#18114,#18115,#16920,.T.);
#22109=EDGE_CURVE('',#18116,#18115,#7501,.T.);
#22110=EDGE_CURVE('',#18116,#18117,#16921,.T.);
#22111=EDGE_CURVE('',#18108,#18117,#7502,.T.);
#22112=EDGE_CURVE('',#18111,#18100,#7503,.T.);
#22113=EDGE_CURVE('',#18099,#18112,#7504,.T.);
#22114=EDGE_CURVE('',#18109,#18102,#7505,.T.);
#22115=EDGE_CURVE('',#18101,#18110,#7506,.T.);
#22116=EDGE_CURVE('',#18107,#18114,#7507,.T.);
#22117=EDGE_CURVE('',#18115,#18106,#7508,.T.);
#22118=EDGE_CURVE('',#18105,#18116,#7509,.T.);
#22119=EDGE_CURVE('',#18117,#18104,#7510,.T.);
#22120=EDGE_CURVE('',#18103,#18108,#7511,.T.);
#22121=EDGE_CURVE('',#18113,#18098,#7512,.T.);
#22122=EDGE_CURVE('',#17430,#17371,#2254,.T.);
#22123=EDGE_CURVE('',#17958,#17423,#16922,.T.);
#22124=EDGE_CURVE('',#17422,#18118,#2255,.T.);
#22125=EDGE_CURVE('',#18118,#18119,#16923,.T.);
#22126=EDGE_CURVE('',#18119,#18120,#7513,.T.);
#22127=EDGE_CURVE('',#18120,#17431,#16924,.T.);
#22128=EDGE_CURVE('',#18121,#18122,#2256,.T.);
#22129=EDGE_CURVE('',#18122,#18123,#16925,.T.);
#22130=EDGE_CURVE('',#18123,#17351,#7514,.T.);
#22131=EDGE_CURVE('',#17350,#18124,#2257,.T.);
#22132=EDGE_CURVE('',#18124,#18125,#16926,.T.);
#22133=EDGE_CURVE('',#18125,#18126,#7515,.T.);
#22134=EDGE_CURVE('',#18126,#18121,#16927,.T.);
#22135=EDGE_CURVE('',#18127,#18128,#2258,.T.);
#22136=EDGE_CURVE('',#18128,#18129,#16928,.T.);
#22137=EDGE_CURVE('',#18129,#18130,#7516,.T.);
#22138=EDGE_CURVE('',#18130,#18131,#16929,.T.);
#22139=EDGE_CURVE('',#18131,#17355,#2259,.T.);
#22140=EDGE_CURVE('',#17354,#18132,#7517,.T.);
#22141=EDGE_CURVE('',#18132,#18127,#16930,.T.);
#22142=EDGE_CURVE('',#17366,#18133,#2260,.T.);
#22143=EDGE_CURVE('',#18133,#18134,#16931,.T.);
#22144=EDGE_CURVE('',#18134,#18135,#7518,.T.);
#22145=EDGE_CURVE('',#18135,#18136,#16932,.T.);
#22146=EDGE_CURVE('',#18136,#18137,#2261,.T.);
#22147=EDGE_CURVE('',#18137,#18138,#16933,.T.);
#22148=EDGE_CURVE('',#18138,#17367,#7519,.T.);
#22149=EDGE_CURVE('',#17362,#18139,#2262,.T.);
#22150=EDGE_CURVE('',#18139,#18140,#16934,.T.);
#22151=EDGE_CURVE('',#18140,#18141,#7520,.T.);
#22152=EDGE_CURVE('',#18141,#18142,#16935,.T.);
#22153=EDGE_CURVE('',#18142,#18143,#2263,.T.);
#22154=EDGE_CURVE('',#18143,#18144,#16936,.T.);
#22155=EDGE_CURVE('',#18144,#17363,#7521,.T.);
#22156=EDGE_CURVE('',#18145,#17359,#2264,.T.);
#22157=EDGE_CURVE('',#17358,#18146,#7522,.T.);
#22158=EDGE_CURVE('',#18146,#18147,#16937,.T.);
#22159=EDGE_CURVE('',#18147,#18148,#2265,.T.);
#22160=EDGE_CURVE('',#18148,#18149,#16938,.T.);
#22161=EDGE_CURVE('',#18149,#18150,#7523,.T.);
#22162=EDGE_CURVE('',#18150,#18145,#16939,.T.);
#22163=EDGE_CURVE('',#17438,#17395,#2266,.T.);
#22164=EDGE_CURVE('',#17818,#17427,#16940,.T.);
#22165=EDGE_CURVE('',#17426,#18151,#2267,.T.);
#22166=EDGE_CURVE('',#18151,#17843,#16941,.T.);
#22167=EDGE_CURVE('',#17842,#17439,#16942,.T.);
#22168=EDGE_CURVE('',#18152,#18153,#2268,.T.);
#22169=EDGE_CURVE('',#18153,#17844,#16943,.T.);
#22170=EDGE_CURVE('',#17374,#18154,#2269,.T.);
#22171=EDGE_CURVE('',#18154,#17849,#16944,.T.);
#22172=EDGE_CURVE('',#17848,#18152,#16945,.T.);
#22173=EDGE_CURVE('',#18155,#18156,#2270,.T.);
#22174=EDGE_CURVE('',#18156,#17853,#16946,.T.);
#22175=EDGE_CURVE('',#17852,#18157,#16947,.T.);
#22176=EDGE_CURVE('',#18157,#17379,#2271,.T.);
#22177=EDGE_CURVE('',#17821,#18155,#16948,.T.);
#22178=EDGE_CURVE('',#17390,#18158,#2272,.T.);
#22179=EDGE_CURVE('',#18158,#17822,#16949,.T.);
#22180=EDGE_CURVE('',#17823,#18159,#16950,.T.);
#22181=EDGE_CURVE('',#18159,#18160,#2273,.T.);
#22182=EDGE_CURVE('',#18160,#17827,#16951,.T.);
#22183=EDGE_CURVE('',#17386,#18161,#2274,.T.);
#22184=EDGE_CURVE('',#18161,#17828,#16952,.T.);
#22185=EDGE_CURVE('',#17829,#18162,#16953,.T.);
#22186=EDGE_CURVE('',#18162,#18163,#2275,.T.);
#22187=EDGE_CURVE('',#18163,#17833,#16954,.T.);
#22188=EDGE_CURVE('',#18164,#17383,#2276,.T.);
#22189=EDGE_CURVE('',#17834,#18165,#16955,.T.);
#22190=EDGE_CURVE('',#18165,#18166,#2277,.T.);
#22191=EDGE_CURVE('',#18166,#17839,#16956,.T.);
#22192=EDGE_CURVE('',#17838,#18164,#16957,.T.);
#22193=EDGE_CURVE('',#17854,#17435,#16958,.T.);
#22194=EDGE_CURVE('',#17434,#18167,#2278,.T.);
#22195=EDGE_CURVE('',#18167,#17879,#16959,.T.);
#22196=EDGE_CURVE('',#17878,#17465,#16960,.T.);
#22197=EDGE_CURVE('',#17892,#17880,#16961,.T.);
#22198=EDGE_CURVE('',#17398,#18168,#2279,.T.);
#22199=EDGE_CURVE('',#18168,#17885,#16962,.T.);
#22200=EDGE_CURVE('',#17884,#17893,#16963,.T.);
#22201=EDGE_CURVE('',#18169,#18170,#2280,.T.);
#22202=EDGE_CURVE('',#18170,#17889,#16964,.T.);
#22203=EDGE_CURVE('',#17888,#18171,#16965,.T.);
#22204=EDGE_CURVE('',#18171,#17403,#2281,.T.);
#22205=EDGE_CURVE('',#17857,#18169,#16966,.T.);
#22206=EDGE_CURVE('',#17961,#17858,#16967,.T.);
#22207=EDGE_CURVE('',#17859,#18172,#16968,.T.);
#22208=EDGE_CURVE('',#18172,#18173,#2282,.T.);
#22209=EDGE_CURVE('',#18173,#17863,#16969,.T.);
#22210=EDGE_CURVE('',#17960,#17864,#16970,.T.);
#22211=EDGE_CURVE('',#17865,#18174,#16971,.T.);
#22212=EDGE_CURVE('',#18174,#18175,#2283,.T.);
#22213=EDGE_CURVE('',#18175,#17869,#16972,.T.);
#22214=EDGE_CURVE('',#17870,#18176,#16973,.T.);
#22215=EDGE_CURVE('',#18176,#18177,#2284,.T.);
#22216=EDGE_CURVE('',#18177,#17875,#16974,.T.);
#22217=EDGE_CURVE('',#17874,#17959,#16975,.T.);
#22218=EDGE_CURVE('',#18169,#17947,#7524,.T.);
#22219=EDGE_CURVE('',#17946,#18170,#7525,.T.);
#22220=EDGE_CURVE('',#17905,#18132,#7526,.T.);
#22221=EDGE_CURVE('',#18134,#17915,#7527,.T.);
#22222=EDGE_CURVE('',#17914,#18135,#7528,.T.);
#22223=EDGE_CURVE('',#18138,#17911,#7529,.T.);
#22224=EDGE_CURVE('',#18140,#17921,#7530,.T.);
#22225=EDGE_CURVE('',#17920,#18141,#7531,.T.);
#22226=EDGE_CURVE('',#18144,#17917,#7532,.T.);
#22227=EDGE_CURVE('',#17927,#18146,#7533,.T.);
#22228=EDGE_CURVE('',#17923,#18150,#7534,.T.);
#22229=EDGE_CURVE('',#18149,#17924,#7535,.T.);
#22230=EDGE_CURVE('',#17895,#18120,#7536,.T.);
#22231=EDGE_CURVE('',#18119,#17896,#7537,.T.);
#22232=EDGE_CURVE('',#18123,#17902,#7538,.T.);
#22233=EDGE_CURVE('',#17899,#18126,#7539,.T.);
#22234=EDGE_CURVE('',#18125,#17900,#7540,.T.);
#22235=EDGE_CURVE('',#17907,#18130,#7541,.T.);
#22236=EDGE_CURVE('',#18129,#17908,#7542,.T.);
#22237=EDGE_CURVE('',#17933,#18156,#7543,.T.);
#22238=EDGE_CURVE('',#18155,#17934,#7544,.T.);
#22239=EDGE_CURVE('',#18171,#17945,#7545,.T.);
#22240=EDGE_CURVE('',#17930,#18153,#7546,.T.);
#22241=EDGE_CURVE('',#18152,#17931,#7547,.T.);
#22242=EDGE_CURVE('',#17944,#18168,#7548,.T.);
#22243=EDGE_CURVE('',#17957,#18167,#7549,.T.);
#22244=EDGE_CURVE('',#18164,#17943,#7550,.T.);
#22245=EDGE_CURVE('',#18176,#17955,#7551,.T.);
#22246=EDGE_CURVE('',#17954,#18177,#7552,.T.);
#22247=EDGE_CURVE('',#17940,#18161,#7553,.T.);
#22248=EDGE_CURVE('',#18174,#17952,#7554,.T.);
#22249=EDGE_CURVE('',#17951,#18175,#7555,.T.);
#22250=EDGE_CURVE('',#18172,#17949,#7556,.T.);
#22251=EDGE_CURVE('',#17948,#18173,#7557,.T.);
#22252=EDGE_CURVE('',#17937,#18158,#7558,.T.);
#22253=EDGE_CURVE('',#17909,#18128,#7559,.T.);
#22254=EDGE_CURVE('',#18127,#17910,#7560,.T.);
#22255=EDGE_CURVE('',#18157,#17932,#7561,.T.);
#22256=EDGE_CURVE('',#17903,#18122,#7562,.T.);
#22257=EDGE_CURVE('',#18121,#17904,#7563,.T.);
#22258=EDGE_CURVE('',#17929,#18154,#7564,.T.);
#22259=EDGE_CURVE('',#17894,#18151,#7565,.T.);
#22260=EDGE_CURVE('',#18145,#17928,#7566,.T.);
#22261=EDGE_CURVE('',#18165,#17942,#7567,.T.);
#22262=EDGE_CURVE('',#17941,#18166,#7568,.T.);
#22263=EDGE_CURVE('',#17922,#18139,#7569,.T.);
#22264=EDGE_CURVE('',#18162,#17939,#7570,.T.);
#22265=EDGE_CURVE('',#17938,#18163,#7571,.T.);
#22266=EDGE_CURVE('',#18159,#17936,#7572,.T.);
#22267=EDGE_CURVE('',#17935,#18160,#7573,.T.);
#22268=EDGE_CURVE('',#17916,#18133,#7574,.T.);
#22269=EDGE_CURVE('',#18131,#17906,#7575,.T.);
#22270=EDGE_CURVE('',#17901,#18124,#7576,.T.);
#22271=EDGE_CURVE('',#17897,#18118,#7577,.T.);
#22272=EDGE_CURVE('',#18147,#17926,#7578,.T.);
#22273=EDGE_CURVE('',#17925,#18148,#7579,.T.);
#22274=EDGE_CURVE('',#18142,#17919,#7580,.T.);
#22275=EDGE_CURVE('',#17918,#18143,#7581,.T.);
#22276=EDGE_CURVE('',#18136,#17913,#7582,.T.);
#22277=EDGE_CURVE('',#17912,#18137,#7583,.T.);
#22278=EDGE_CURVE('',#18003,#17976,#7584,.T.);
#22279=EDGE_CURVE('',#18004,#17977,#7585,.T.);
#22280=EDGE_CURVE('',#18002,#17978,#7586,.T.);
#22281=EDGE_CURVE('',#18013,#17979,#7587,.T.);
#22282=EDGE_CURVE('',#18012,#17980,#7588,.T.);
#22283=EDGE_CURVE('',#18011,#17981,#7589,.T.);
#22284=EDGE_CURVE('',#18010,#17982,#7590,.T.);
#22285=EDGE_CURVE('',#18009,#17983,#7591,.T.);
#22286=EDGE_CURVE('',#18008,#17984,#7592,.T.);
#22287=EDGE_CURVE('',#18007,#17985,#7593,.T.);
#22288=EDGE_CURVE('',#18006,#17986,#7594,.T.);
#22289=EDGE_CURVE('',#18005,#17987,#7595,.T.);
#22290=EDGE_CURVE('',#17999,#17972,#7596,.T.);
#22291=EDGE_CURVE('',#18000,#17973,#7597,.T.);
#22292=EDGE_CURVE('',#17998,#17974,#7598,.T.);
#22293=EDGE_CURVE('',#18001,#17975,#7599,.T.);
#22294=EDGE_CURVE('',#17817,#17617,#7600,.T.);
#22295=EDGE_CURVE('',#17816,#17616,#7601,.T.);
#22296=EDGE_CURVE('',#17722,#17710,#7602,.T.);
#22297=EDGE_CURVE('',#17723,#17711,#7603,.T.);
#22298=EDGE_CURVE('',#17724,#17708,#7604,.T.);
#22299=EDGE_CURVE('',#17725,#17709,#7605,.T.);
#22300=EDGE_CURVE('',#17727,#17619,#7606,.T.);
#22301=EDGE_CURVE('',#17726,#17618,#7607,.T.);
#22302=EDGE_CURVE('',#17814,#17706,#7608,.T.);
#22303=EDGE_CURVE('',#17815,#17707,#7609,.T.);
#22304=EDGE_CURVE('',#17813,#17621,#7610,.T.);
#22305=EDGE_CURVE('',#17812,#17620,#7611,.T.);
#22306=EDGE_CURVE('',#17729,#17623,#7612,.T.);
#22307=EDGE_CURVE('',#17728,#17622,#7613,.T.);
#22308=EDGE_CURVE('',#17810,#17704,#7614,.T.);
#22309=EDGE_CURVE('',#17811,#17705,#7615,.T.);
#22310=EDGE_CURVE('',#17808,#17702,#7616,.T.);
#22311=EDGE_CURVE('',#17809,#17703,#7617,.T.);
#22312=EDGE_CURVE('',#17806,#17700,#7618,.T.);
#22313=EDGE_CURVE('',#17807,#17701,#7619,.T.);
#22314=EDGE_CURVE('',#17804,#17698,#7620,.T.);
#22315=EDGE_CURVE('',#17805,#17699,#7621,.T.);
#22316=EDGE_CURVE('',#17803,#17625,#7622,.T.);
#22317=EDGE_CURVE('',#17802,#17624,#7623,.T.);
#22318=EDGE_CURVE('',#17731,#17627,#7624,.T.);
#22319=EDGE_CURVE('',#17730,#17626,#7625,.T.);
#22320=EDGE_CURVE('',#17801,#17629,#7626,.T.);
#22321=EDGE_CURVE('',#17800,#17628,#7627,.T.);
#22322=EDGE_CURVE('',#17733,#17631,#7628,.T.);
#22323=EDGE_CURVE('',#17732,#17630,#7629,.T.);
#22324=EDGE_CURVE('',#17799,#17633,#7630,.T.);
#22325=EDGE_CURVE('',#17798,#17632,#7631,.T.);
#22326=EDGE_CURVE('',#17735,#17635,#7632,.T.);
#22327=EDGE_CURVE('',#17734,#17634,#7633,.T.);
#22328=EDGE_CURVE('',#17797,#17637,#7634,.T.);
#22329=EDGE_CURVE('',#17796,#17636,#7635,.T.);
#22330=EDGE_CURVE('',#17736,#17696,#7636,.T.);
#22331=EDGE_CURVE('',#17737,#17697,#7637,.T.);
#22332=EDGE_CURVE('',#17738,#17694,#7638,.T.);
#22333=EDGE_CURVE('',#17739,#17695,#7639,.T.);
#22334=EDGE_CURVE('',#17740,#17692,#7640,.T.);
#22335=EDGE_CURVE('',#17741,#17693,#7641,.T.);
#22336=EDGE_CURVE('',#17742,#17690,#7642,.T.);
#22337=EDGE_CURVE('',#17743,#17691,#7643,.T.);
#22338=EDGE_CURVE('',#17744,#17688,#7644,.T.);
#22339=EDGE_CURVE('',#17745,#17689,#7645,.T.);
#22340=EDGE_CURVE('',#17747,#17639,#7646,.T.);
#22341=EDGE_CURVE('',#17746,#17638,#7647,.T.);
#22342=EDGE_CURVE('',#17794,#17686,#7648,.T.);
#22343=EDGE_CURVE('',#17795,#17687,#7649,.T.);
#22344=EDGE_CURVE('',#17792,#17640,#7650,.T.);
#22345=EDGE_CURVE('',#17793,#17641,#7651,.T.);
#22346=EDGE_CURVE('',#17748,#17642,#7652,.T.);
#22347=EDGE_CURVE('',#17749,#17643,#7653,.T.);
#22348=EDGE_CURVE('',#17790,#17684,#7654,.T.);
#22349=EDGE_CURVE('',#17791,#17685,#7655,.T.);
#22350=EDGE_CURVE('',#17788,#17644,#7656,.T.);
#22351=EDGE_CURVE('',#17789,#17645,#7657,.T.);
#22352=EDGE_CURVE('',#17750,#17682,#7658,.T.);
#22353=EDGE_CURVE('',#17751,#17683,#7659,.T.);
#22354=EDGE_CURVE('',#17752,#17680,#7660,.T.);
#22355=EDGE_CURVE('',#17753,#17681,#7661,.T.);
#22356=EDGE_CURVE('',#17754,#17646,#7662,.T.);
#22357=EDGE_CURVE('',#17755,#17647,#7663,.T.);
#22358=EDGE_CURVE('',#17786,#17648,#7664,.T.);
#22359=EDGE_CURVE('',#17787,#17649,#7665,.T.);
#22360=EDGE_CURVE('',#17756,#17650,#7666,.T.);
#22361=EDGE_CURVE('',#17757,#17651,#7667,.T.);
#22362=EDGE_CURVE('',#17784,#17652,#7668,.T.);
#22363=EDGE_CURVE('',#17785,#17653,#7669,.T.);
#22364=EDGE_CURVE('',#17758,#17678,#7670,.T.);
#22365=EDGE_CURVE('',#17759,#17679,#7671,.T.);
#22366=EDGE_CURVE('',#17760,#17676,#7672,.T.);
#22367=EDGE_CURVE('',#17761,#17677,#7673,.T.);
#22368=EDGE_CURVE('',#17762,#17674,#7674,.T.);
#22369=EDGE_CURVE('',#17763,#17675,#7675,.T.);
#22370=EDGE_CURVE('',#17764,#17672,#7676,.T.);
#22371=EDGE_CURVE('',#17765,#17673,#7677,.T.);
#22372=EDGE_CURVE('',#17766,#17670,#7678,.T.);
#22373=EDGE_CURVE('',#17767,#17671,#7679,.T.);
#22374=EDGE_CURVE('',#17768,#17668,#7680,.T.);
#22375=EDGE_CURVE('',#17769,#17669,#7681,.T.);
#22376=EDGE_CURVE('',#17770,#17666,#7682,.T.);
#22377=EDGE_CURVE('',#17771,#17667,#7683,.T.);
#22378=EDGE_CURVE('',#17772,#17654,#7684,.T.);
#22379=EDGE_CURVE('',#17773,#17655,#7685,.T.);
#22380=EDGE_CURVE('',#17782,#17656,#7686,.T.);
#22381=EDGE_CURVE('',#17783,#17657,#7687,.T.);
#22382=EDGE_CURVE('',#17774,#17658,#7688,.T.);
#22383=EDGE_CURVE('',#17775,#17659,#7689,.T.);
#22384=EDGE_CURVE('',#17780,#17660,#7690,.T.);
#22385=EDGE_CURVE('',#17781,#17661,#7691,.T.);
#22386=EDGE_CURVE('',#17776,#17662,#7692,.T.);
#22387=EDGE_CURVE('',#17777,#17663,#7693,.T.);
#22388=EDGE_CURVE('',#17778,#17664,#7694,.T.);
#22389=EDGE_CURVE('',#17779,#17665,#7695,.T.);
#22390=EDGE_CURVE('',#17480,#17542,#7696,.T.);
#22391=EDGE_CURVE('',#17479,#17543,#7697,.T.);
#22392=EDGE_CURVE('',#17478,#17544,#7698,.T.);
#22393=EDGE_CURVE('',#17477,#17545,#7699,.T.);
#22394=EDGE_CURVE('',#17476,#17546,#7700,.T.);
#22395=EDGE_CURVE('',#17475,#17547,#7701,.T.);
#22396=EDGE_CURVE('',#17572,#17593,#7702,.T.);
#22397=EDGE_CURVE('',#17477,#17572,#16976,.T.);
#22398=EDGE_CURVE('',#17545,#17593,#16977,.T.);
#22399=EDGE_CURVE('',#17570,#17478,#16978,.T.);
#22400=EDGE_CURVE('',#17570,#17592,#7703,.T.);
#22401=EDGE_CURVE('',#17592,#17544,#16979,.T.);
#22402=EDGE_CURVE('',#17594,#17571,#7704,.T.);
#22403=EDGE_CURVE('',#17597,#17573,#7705,.T.);
#22404=EDGE_CURVE('',#17595,#17575,#7706,.T.);
#22405=EDGE_CURVE('',#17596,#17574,#7707,.T.);
#22406=EDGE_CURVE('',#17598,#17582,#16980,.T.);
#22407=EDGE_CURVE('',#17583,#17599,#16981,.T.);
#22408=EDGE_CURVE('',#17601,#17578,#16982,.T.);
#22409=EDGE_CURVE('',#17579,#17600,#16983,.T.);
#22410=EDGE_CURVE('',#17582,#18178,#16984,.T.);
#22411=EDGE_CURVE('',#18178,#18179,#7708,.T.);
#22412=EDGE_CURVE('',#18179,#17579,#16985,.T.);
#22413=EDGE_CURVE('',#17578,#18180,#16986,.T.);
#22414=EDGE_CURVE('',#18180,#18181,#7709,.T.);
#22415=EDGE_CURVE('',#18181,#17583,#16987,.T.);
#22416=EDGE_CURVE('',#17577,#18182,#16988,.T.);
#22417=EDGE_CURVE('',#18182,#18183,#7710,.T.);
#22418=EDGE_CURVE('',#18183,#18184,#16989,.T.);
#22419=EDGE_CURVE('',#18184,#18185,#7711,.T.);
#22420=EDGE_CURVE('',#18185,#18186,#16990,.T.);
#22421=EDGE_CURVE('',#18186,#18187,#7712,.T.);
#22422=EDGE_CURVE('',#18187,#17580,#16991,.T.);
#22423=EDGE_CURVE('',#18188,#18179,#7713,.T.);
#22424=EDGE_CURVE('',#18189,#18188,#16992,.T.);
#22425=EDGE_CURVE('',#18190,#18189,#7714,.T.);
#22426=EDGE_CURVE('',#18191,#18190,#16993,.T.);
#22427=EDGE_CURVE('',#18180,#18191,#7715,.T.);
#22428=EDGE_CURVE('',#17581,#18192,#16994,.T.);
#22429=EDGE_CURVE('',#18193,#18192,#7716,.T.);
#22430=EDGE_CURVE('',#18193,#18194,#16995,.T.);
#22431=EDGE_CURVE('',#18195,#18194,#7717,.T.);
#22432=EDGE_CURVE('',#18195,#18196,#16996,.T.);
#22433=EDGE_CURVE('',#18197,#18196,#7718,.T.);
#22434=EDGE_CURVE('',#18197,#17576,#16997,.T.);
#22435=EDGE_CURVE('',#18181,#18198,#7719,.T.);
#22436=EDGE_CURVE('',#18199,#18198,#16998,.T.);
#22437=EDGE_CURVE('',#18199,#18200,#7720,.T.);
#22438=EDGE_CURVE('',#18201,#18200,#16999,.T.);
#22439=EDGE_CURVE('',#18201,#18178,#7721,.T.);
#22440=EDGE_CURVE('',#18200,#18189,#7722,.T.);
#22441=EDGE_CURVE('',#18188,#18201,#7723,.T.);
#22442=EDGE_CURVE('',#18198,#18191,#7724,.T.);
#22443=EDGE_CURVE('',#18190,#18199,#7725,.T.);
#22444=EDGE_CURVE('',#18186,#18193,#7726,.T.);
#22445=EDGE_CURVE('',#18194,#18185,#7727,.T.);
#22446=EDGE_CURVE('',#18184,#18195,#7728,.T.);
#22447=EDGE_CURVE('',#18196,#18183,#7729,.T.);
#22448=EDGE_CURVE('',#18182,#18197,#7730,.T.);
#22449=EDGE_CURVE('',#18192,#18187,#7731,.T.);
#22450=EDGE_CURVE('',#17590,#17604,#17000,.T.);
#22451=EDGE_CURVE('',#17603,#17591,#17001,.T.);
#22452=EDGE_CURVE('',#17586,#17602,#17002,.T.);
#22453=EDGE_CURVE('',#17605,#17587,#17003,.T.);
#22454=EDGE_CURVE('',#18202,#17586,#17004,.T.);
#22455=EDGE_CURVE('',#18203,#18202,#7732,.T.);
#22456=EDGE_CURVE('',#17591,#18203,#17005,.T.);
#22457=EDGE_CURVE('',#18204,#17590,#17006,.T.);
#22458=EDGE_CURVE('',#18205,#18204,#7733,.T.);
#22459=EDGE_CURVE('',#17587,#18205,#17007,.T.);
#22460=EDGE_CURVE('',#18206,#17584,#17008,.T.);
#22461=EDGE_CURVE('',#18207,#18206,#7734,.T.);
#22462=EDGE_CURVE('',#18208,#18207,#17009,.T.);
#22463=EDGE_CURVE('',#18209,#18208,#7735,.T.);
#22464=EDGE_CURVE('',#18210,#18209,#17010,.T.);
#22465=EDGE_CURVE('',#18211,#18210,#7736,.T.);
#22466=EDGE_CURVE('',#17588,#18211,#17011,.T.);
#22467=EDGE_CURVE('',#18205,#18212,#7737,.T.);
#22468=EDGE_CURVE('',#18212,#18213,#17012,.T.);
#22469=EDGE_CURVE('',#18213,#18214,#7738,.T.);
#22470=EDGE_CURVE('',#18214,#18215,#17013,.T.);
#22471=EDGE_CURVE('',#18215,#18202,#7739,.T.);
#22472=EDGE_CURVE('',#18216,#17589,#17014,.T.);
#22473=EDGE_CURVE('',#18216,#18217,#7740,.T.);
#22474=EDGE_CURVE('',#18218,#18217,#17015,.T.);
#22475=EDGE_CURVE('',#18218,#18219,#7741,.T.);
#22476=EDGE_CURVE('',#18220,#18219,#17016,.T.);
#22477=EDGE_CURVE('',#18220,#18221,#7742,.T.);
#22478=EDGE_CURVE('',#17585,#18221,#17017,.T.);
#22479=EDGE_CURVE('',#18222,#18203,#7743,.T.);
#22480=EDGE_CURVE('',#18222,#18223,#17018,.T.);
#22481=EDGE_CURVE('',#18224,#18223,#7744,.T.);
#22482=EDGE_CURVE('',#18224,#18225,#17019,.T.);
#22483=EDGE_CURVE('',#18204,#18225,#7745,.T.);
#22484=EDGE_CURVE('',#18215,#18222,#7746,.T.);
#22485=EDGE_CURVE('',#18223,#18214,#7747,.T.);
#22486=EDGE_CURVE('',#18213,#18224,#7748,.T.);
#22487=EDGE_CURVE('',#18225,#18212,#7749,.T.);
#22488=EDGE_CURVE('',#18219,#18208,#7750,.T.);
#22489=EDGE_CURVE('',#18207,#18220,#7751,.T.);
#22490=EDGE_CURVE('',#18217,#18210,#7752,.T.);
#22491=EDGE_CURVE('',#18209,#18218,#7753,.T.);
#22492=EDGE_CURVE('',#18211,#18216,#7754,.T.);
#22493=EDGE_CURVE('',#18221,#18206,#7755,.T.);
#22494=EDGE_CURVE('',#17467,#17528,#7756,.T.);
#22495=EDGE_CURVE('',#17493,#17529,#7757,.T.);
#22496=EDGE_CURVE('',#17492,#17530,#7758,.T.);
#22497=EDGE_CURVE('',#17491,#17531,#7759,.T.);
#22498=EDGE_CURVE('',#17490,#17532,#7760,.T.);
#22499=EDGE_CURVE('',#17489,#17533,#7761,.T.);
#22500=EDGE_CURVE('',#18226,#18227,#7762,.T.);
#22501=EDGE_CURVE('',#17491,#18226,#17020,.T.);
#22502=EDGE_CURVE('',#17531,#18227,#17021,.T.);
#22503=EDGE_CURVE('',#18228,#17492,#17022,.T.);
#22504=EDGE_CURVE('',#18228,#18229,#7763,.T.);
#22505=EDGE_CURVE('',#18229,#17530,#17023,.T.);
#22506=EDGE_CURVE('',#18229,#18227,#7764,.T.);
#22507=EDGE_CURVE('',#18226,#18228,#7765,.T.);
#22508=EDGE_CURVE('',#18226,#18230,#7766,.T.);
#22509=EDGE_CURVE('',#18227,#18231,#7767,.T.);
#22510=EDGE_CURVE('',#18231,#18230,#7768,.T.);
#22511=EDGE_CURVE('',#18232,#18229,#7769,.T.);
#22512=EDGE_CURVE('',#18233,#18228,#7770,.T.);
#22513=EDGE_CURVE('',#18232,#18233,#7771,.T.);
#22514=EDGE_CURVE('',#18234,#18232,#17024,.T.);
#22515=EDGE_CURVE('',#18235,#18234,#7772,.T.);
#22516=EDGE_CURVE('',#18231,#18235,#17025,.T.);
#22517=EDGE_CURVE('',#18230,#18236,#17026,.T.);
#22518=EDGE_CURVE('',#18236,#18237,#7773,.T.);
#22519=EDGE_CURVE('',#18237,#18233,#17027,.T.);
#22520=EDGE_CURVE('',#18234,#18237,#7774,.T.);
#22521=EDGE_CURVE('',#18235,#18236,#7775,.T.);
#22522=EDGE_CURVE('',#18238,#18238,#17028,.T.);
#22523=EDGE_CURVE('',#18238,#18239,#7776,.T.);
#22524=EDGE_CURVE('',#18239,#18239,#17029,.T.);
#22525=EDGE_CURVE('',#18240,#18240,#17030,.T.);
#22526=EDGE_CURVE('',#18240,#18241,#7777,.T.);
#22527=EDGE_CURVE('',#18241,#18241,#17031,.T.);
#22528=EDGE_CURVE('',#18242,#18242,#17032,.T.);
#22529=EDGE_CURVE('',#18242,#18243,#7778,.T.);
#22530=EDGE_CURVE('',#18243,#18243,#17033,.T.);
#22531=EDGE_CURVE('',#18244,#18245,#17034,.T.);
#22532=EDGE_CURVE('',#18245,#18244,#17035,.T.);
#22533=EDGE_CURVE('',#18245,#18246,#7779,.T.);
#22534=EDGE_CURVE('',#18246,#18246,#17036,.T.);
#22535=EDGE_CURVE('',#18247,#18248,#17037,.T.);
#22536=EDGE_CURVE('',#18248,#18247,#17038,.T.);
#22537=EDGE_CURVE('',#18248,#18249,#7780,.T.);
#22538=EDGE_CURVE('',#18249,#18249,#17039,.T.);
#22539=EDGE_CURVE('',#18244,#18250,#7781,.T.);
#22540=EDGE_CURVE('',#18250,#18250,#17040,.T.);
#22541=EDGE_CURVE('',#18251,#18252,#17041,.T.);
#22542=EDGE_CURVE('',#18251,#18253,#7782,.T.);
#22543=EDGE_CURVE('',#18253,#18254,#17042,.T.);
#22544=EDGE_CURVE('',#18252,#18254,#7783,.T.);
#22545=EDGE_CURVE('',#18247,#18255,#7784,.T.);
#22546=EDGE_CURVE('',#18255,#18255,#17043,.T.);
#22547=EDGE_CURVE('',#18256,#18257,#17044,.T.);
#22548=EDGE_CURVE('',#18257,#18258,#7785,.T.);
#22549=EDGE_CURVE('',#18259,#18258,#17045,.T.);
#22550=EDGE_CURVE('',#18260,#18259,#7786,.T.);
#22551=EDGE_CURVE('',#18260,#18261,#17046,.T.);
#22552=EDGE_CURVE('',#18261,#18262,#7787,.T.);
#22553=EDGE_CURVE('',#18263,#18262,#17047,.T.);
#22554=EDGE_CURVE('',#18263,#18264,#7788,.T.);
#22555=EDGE_CURVE('',#18264,#18265,#17048,.T.);
#22556=EDGE_CURVE('',#18266,#18265,#7789,.T.);
#22557=EDGE_CURVE('',#18267,#18266,#17049,.T.);
#22558=EDGE_CURVE('',#18256,#18267,#7790,.T.);
#22559=EDGE_CURVE('',#18268,#18269,#7791,.T.);
#22560=EDGE_CURVE('',#18270,#18269,#7792,.T.);
#22561=EDGE_CURVE('',#18270,#18271,#7793,.T.);
#22562=EDGE_CURVE('',#18268,#18271,#7794,.T.);
#22563=EDGE_CURVE('',#18272,#18273,#7795,.T.);
#22564=EDGE_CURVE('',#18274,#18273,#7796,.T.);
#22565=EDGE_CURVE('',#18274,#18275,#7797,.T.);
#22566=EDGE_CURVE('',#18272,#18275,#7798,.T.);
#22567=EDGE_CURVE('',#18276,#18277,#7799,.T.);
#22568=EDGE_CURVE('',#18278,#18277,#7800,.T.);
#22569=EDGE_CURVE('',#18278,#18279,#7801,.T.);
#22570=EDGE_CURVE('',#18276,#18279,#7802,.T.);
#22571=EDGE_CURVE('',#18280,#18281,#7803,.T.);
#22572=EDGE_CURVE('',#18280,#18282,#7804,.T.);
#22573=EDGE_CURVE('',#18282,#18283,#7805,.T.);
#22574=EDGE_CURVE('',#18281,#18283,#7806,.T.);
#22575=EDGE_CURVE('',#18284,#18285,#7807,.T.);
#22576=EDGE_CURVE('',#18284,#18286,#7808,.T.);
#22577=EDGE_CURVE('',#18286,#18281,#7809,.T.);
#22578=EDGE_CURVE('',#18287,#18283,#7810,.T.);
#22579=EDGE_CURVE('',#18285,#18287,#7811,.T.);
#22580=EDGE_CURVE('',#18288,#18289,#7812,.T.);
#22581=EDGE_CURVE('',#18289,#18290,#7813,.T.);
#22582=EDGE_CURVE('',#18282,#18290,#7814,.T.);
#22583=EDGE_CURVE('',#18291,#18280,#7815,.T.);
#22584=EDGE_CURVE('',#18291,#18288,#7816,.T.);
#22585=EDGE_CURVE('',#18284,#18288,#7817,.T.);
#22586=EDGE_CURVE('',#18286,#18291,#7818,.T.);
#22587=EDGE_CURVE('',#18292,#18293,#7819,.T.);
#22588=EDGE_CURVE('',#18294,#18292,#7820,.T.);
#22589=EDGE_CURVE('',#18294,#18295,#7821,.T.);
#22590=EDGE_CURVE('',#18295,#18296,#7822,.T.);
#22591=EDGE_CURVE('',#18296,#18297,#7823,.T.);
#22592=EDGE_CURVE('',#18293,#18297,#7824,.T.);
#22593=EDGE_CURVE('',#18298,#18299,#7825,.T.);
#22594=EDGE_CURVE('',#18298,#18293,#7826,.T.);
#22595=EDGE_CURVE('',#18299,#18297,#7827,.T.);
#22596=EDGE_CURVE('',#18300,#18298,#7828,.T.);
#22597=EDGE_CURVE('',#18299,#18301,#7829,.T.);
#22598=EDGE_CURVE('',#18302,#18301,#7830,.T.);
#22599=EDGE_CURVE('',#18303,#18302,#7831,.T.);
#22600=EDGE_CURVE('',#18300,#18303,#7832,.T.);
#22601=EDGE_CURVE('',#18292,#18300,#7833,.T.);
#22602=EDGE_CURVE('',#18294,#18303,#7834,.T.);
#22603=EDGE_CURVE('',#18304,#18305,#7835,.T.);
#22604=EDGE_CURVE('',#18304,#18306,#7836,.T.);
#22605=EDGE_CURVE('',#18306,#18307,#7837,.T.);
#22606=EDGE_CURVE('',#18305,#18307,#7838,.T.);
#22607=EDGE_CURVE('',#18308,#18309,#7839,.T.);
#22608=EDGE_CURVE('',#18309,#18305,#7840,.T.);
#22609=EDGE_CURVE('',#18310,#18307,#7841,.T.);
#22610=EDGE_CURVE('',#18311,#18310,#7842,.T.);
#22611=EDGE_CURVE('',#18308,#18311,#7843,.T.);
#22612=EDGE_CURVE('',#18304,#18312,#7844,.T.);
#22613=EDGE_CURVE('',#18312,#18313,#7845,.T.);
#22614=EDGE_CURVE('',#18314,#18313,#7846,.T.);
#22615=EDGE_CURVE('',#18314,#18315,#7847,.T.);
#22616=EDGE_CURVE('',#18306,#18315,#7848,.T.);
#22617=EDGE_CURVE('',#18309,#18312,#7849,.T.);
#22618=EDGE_CURVE('',#18308,#18313,#7850,.T.);
#22619=EDGE_CURVE('',#18316,#18317,#17050,.T.);
#22620=EDGE_CURVE('',#18318,#18316,#7851,.T.);
#22621=EDGE_CURVE('',#18318,#18319,#17051,.T.);
#22622=EDGE_CURVE('',#18320,#18319,#7852,.T.);
#22623=EDGE_CURVE('',#18321,#18320,#17052,.T.);
#22624=EDGE_CURVE('',#18321,#18322,#7853,.T.);
#22625=EDGE_CURVE('',#18322,#18323,#17053,.T.);
#22626=EDGE_CURVE('',#18324,#18323,#7854,.T.);
#22627=EDGE_CURVE('',#18325,#18324,#17054,.T.);
#22628=EDGE_CURVE('',#18325,#18326,#7855,.T.);
#22629=EDGE_CURVE('',#18326,#18327,#17055,.T.);
#22630=EDGE_CURVE('',#18327,#18317,#7856,.T.);
#22631=EDGE_CURVE('',#18310,#18315,#7857,.T.);
#22632=EDGE_CURVE('',#18296,#18301,#7858,.T.);
#22633=EDGE_CURVE('',#18287,#18290,#7859,.T.);
#22634=EDGE_CURVE('',#18328,#18329,#7860,.T.);
#22635=EDGE_CURVE('',#18329,#18330,#17056,.T.);
#22636=EDGE_CURVE('',#18330,#18331,#7861,.T.);
#22637=EDGE_CURVE('',#18331,#18332,#17057,.T.);
#22638=EDGE_CURVE('',#18332,#18333,#7862,.T.);
#22639=EDGE_CURVE('',#18333,#18334,#17058,.T.);
#22640=EDGE_CURVE('',#18334,#18335,#7863,.T.);
#22641=EDGE_CURVE('',#18335,#18328,#17059,.T.);
#22642=EDGE_CURVE('',#18336,#18337,#17060,.T.);
#22643=EDGE_CURVE('',#18338,#18337,#7864,.T.);
#22644=EDGE_CURVE('',#18339,#18338,#17061,.T.);
#22645=EDGE_CURVE('',#18340,#18339,#7865,.T.);
#22646=EDGE_CURVE('',#18340,#18341,#17062,.T.);
#22647=EDGE_CURVE('',#18341,#18342,#7866,.T.);
#22648=EDGE_CURVE('',#18343,#18342,#17063,.T.);
#22649=EDGE_CURVE('',#18344,#18343,#7867,.T.);
#22650=EDGE_CURVE('',#18344,#18345,#17064,.T.);
#22651=EDGE_CURVE('',#18345,#18346,#7868,.T.);
#22652=EDGE_CURVE('',#18347,#18346,#17065,.T.);
#22653=EDGE_CURVE('',#18347,#18336,#7869,.T.);
#22654=EDGE_CURVE('',#18348,#18253,#7870,.T.);
#22655=EDGE_CURVE('',#18348,#18349,#17066,.T.);
#22656=EDGE_CURVE('',#18349,#18350,#7871,.T.);
#22657=EDGE_CURVE('',#18351,#18350,#17067,.T.);
#22658=EDGE_CURVE('',#18351,#18352,#7872,.T.);
#22659=EDGE_CURVE('',#18352,#18353,#17068,.T.);
#22660=EDGE_CURVE('',#18353,#18354,#7873,.T.);
#22661=EDGE_CURVE('',#18354,#18355,#17069,.T.);
#22662=EDGE_CURVE('',#18355,#18356,#7874,.T.);
#22663=EDGE_CURVE('',#18356,#18357,#17070,.T.);
#22664=EDGE_CURVE('',#18254,#18357,#7875,.T.);
#22665=EDGE_CURVE('',#18358,#18359,#7876,.T.);
#22666=EDGE_CURVE('',#18360,#18358,#17071,.T.);
#22667=EDGE_CURVE('',#18360,#18361,#7877,.T.);
#22668=EDGE_CURVE('',#18361,#18362,#17072,.T.);
#22669=EDGE_CURVE('',#18362,#18363,#7878,.T.);
#22670=EDGE_CURVE('',#18364,#18363,#17073,.T.);
#22671=EDGE_CURVE('',#18365,#18364,#7879,.T.);
#22672=EDGE_CURVE('',#18365,#18366,#17074,.T.);
#22673=EDGE_CURVE('',#18367,#18366,#7880,.T.);
#22674=EDGE_CURVE('',#18368,#18367,#17075,.T.);
#22675=EDGE_CURVE('',#18368,#18369,#7881,.T.);
#22676=EDGE_CURVE('',#18369,#18359,#17076,.T.);
#22677=EDGE_CURVE('',#18370,#18371,#7882,.T.);
#22678=EDGE_CURVE('',#18370,#18372,#17077,.T.);
#22679=EDGE_CURVE('',#18372,#18349,#7883,.T.);
#22680=EDGE_CURVE('',#18373,#18348,#7884,.T.);
#22681=EDGE_CURVE('',#18371,#18373,#17078,.T.);
#22682=EDGE_CURVE('',#18374,#18375,#7885,.T.);
#22683=EDGE_CURVE('',#18374,#18370,#7886,.T.);
#22684=EDGE_CURVE('',#18371,#18375,#7887,.T.);
#22685=EDGE_CURVE('',#18376,#18377,#7888,.T.);
#22686=EDGE_CURVE('',#18376,#18378,#17079,.T.);
#22687=EDGE_CURVE('',#18378,#18355,#7889,.T.);
#22688=EDGE_CURVE('',#18379,#18354,#7890,.T.);
#22689=EDGE_CURVE('',#18377,#18379,#17080,.T.);
#22690=EDGE_CURVE('',#18380,#18381,#7891,.T.);
#22691=EDGE_CURVE('',#18380,#18376,#7892,.T.);
#22692=EDGE_CURVE('',#18377,#18381,#7893,.T.);
#22693=EDGE_CURVE('',#18382,#18350,#7894,.T.);
#22694=EDGE_CURVE('',#18382,#18380,#17081,.T.);
#22695=EDGE_CURVE('',#18383,#18381,#17082,.T.);
#22696=EDGE_CURVE('',#18383,#18351,#7895,.T.);
#22697=EDGE_CURVE('',#18372,#18382,#7896,.T.);
#22698=EDGE_CURVE('',#18384,#18356,#7897,.T.);
#22699=EDGE_CURVE('',#18384,#18374,#17083,.T.);
#22700=EDGE_CURVE('',#18385,#18375,#17084,.T.);
#22701=EDGE_CURVE('',#18385,#18357,#7898,.T.);
#22702=EDGE_CURVE('',#18378,#18384,#7899,.T.);
#22703=EDGE_CURVE('',#18386,#18353,#7900,.T.);
#22704=EDGE_CURVE('',#18386,#18379,#7901,.T.);
#22705=EDGE_CURVE('',#18387,#18352,#7902,.T.);
#22706=EDGE_CURVE('',#18387,#18386,#17085,.T.);
#22707=EDGE_CURVE('',#18383,#18387,#7903,.T.);
#22708=EDGE_CURVE('',#18373,#18251,#7904,.T.);
#22709=EDGE_CURVE('',#18252,#18385,#7905,.T.);
#22710=EDGE_CURVE('',#18334,#18382,#17086,.T.);
#22711=EDGE_CURVE('',#18380,#18333,#17087,.T.);
#22712=EDGE_CURVE('',#18376,#18332,#17088,.T.);
#22713=EDGE_CURVE('',#18335,#18372,#17089,.T.);
#22714=EDGE_CURVE('',#18378,#18331,#17090,.T.);
#22715=EDGE_CURVE('',#18328,#18370,#17091,.T.);
#22716=EDGE_CURVE('',#18384,#18330,#17092,.T.);
#22717=EDGE_CURVE('',#18329,#18374,#17093,.T.);
#22718=EDGE_CURVE('',#18257,#18358,#7906,.T.);
#22719=EDGE_CURVE('',#18256,#18360,#7907,.T.);
#22720=EDGE_CURVE('',#18258,#18359,#7908,.T.);
#22721=EDGE_CURVE('',#18259,#18369,#7909,.T.);
#22722=EDGE_CURVE('',#18260,#18368,#7910,.T.);
#22723=EDGE_CURVE('',#18261,#18367,#7911,.T.);
#22724=EDGE_CURVE('',#18262,#18366,#7912,.T.);
#22725=EDGE_CURVE('',#18263,#18365,#7913,.T.);
#22726=EDGE_CURVE('',#18264,#18364,#7914,.T.);
#22727=EDGE_CURVE('',#18265,#18363,#7915,.T.);
#22728=EDGE_CURVE('',#18266,#18362,#7916,.T.);
#22729=EDGE_CURVE('',#18267,#18361,#7917,.T.);
#22730=EDGE_CURVE('',#18316,#18336,#7918,.T.);
#22731=EDGE_CURVE('',#18317,#18337,#7919,.T.);
#22732=EDGE_CURVE('',#18327,#18338,#7920,.T.);
#22733=EDGE_CURVE('',#18326,#18339,#7921,.T.);
#22734=EDGE_CURVE('',#18325,#18340,#7922,.T.);
#22735=EDGE_CURVE('',#18324,#18341,#7923,.T.);
#22736=EDGE_CURVE('',#18323,#18342,#7924,.T.);
#22737=EDGE_CURVE('',#18322,#18343,#7925,.T.);
#22738=EDGE_CURVE('',#18321,#18344,#7926,.T.);
#22739=EDGE_CURVE('',#18320,#18345,#7927,.T.);
#22740=EDGE_CURVE('',#18319,#18346,#7928,.T.);
#22741=EDGE_CURVE('',#18318,#18347,#7929,.T.);
#22742=EDGE_CURVE('',#18289,#18285,#7930,.T.);
#22743=EDGE_CURVE('',#18314,#18311,#7931,.T.);
#22744=EDGE_CURVE('',#18302,#18295,#7932,.T.);
#22745=EDGE_CURVE('',#18388,#18389,#7933,.T.);
#22746=EDGE_CURVE('',#18390,#18389,#7934,.T.);
#22747=EDGE_CURVE('',#18390,#18391,#7935,.T.);
#22748=EDGE_CURVE('',#18388,#18391,#7936,.T.);
#22749=EDGE_CURVE('',#18392,#18393,#7937,.T.);
#22750=EDGE_CURVE('',#18393,#18394,#7938,.T.);
#22751=EDGE_CURVE('',#18394,#18395,#7939,.T.);
#22752=EDGE_CURVE('',#18392,#18395,#7940,.T.);
#22753=EDGE_CURVE('',#18389,#18269,#7941,.T.);
#22754=EDGE_CURVE('',#18388,#18270,#7942,.T.);
#22755=EDGE_CURVE('',#18390,#18268,#7943,.T.);
#22756=EDGE_CURVE('',#18391,#18271,#7944,.T.);
#22757=EDGE_CURVE('',#18396,#18397,#7945,.T.);
#22758=EDGE_CURVE('',#18397,#18398,#7946,.T.);
#22759=EDGE_CURVE('',#18399,#18398,#7947,.T.);
#22760=EDGE_CURVE('',#18399,#18396,#7948,.T.);
#22761=EDGE_CURVE('',#18400,#18399,#7949,.T.);
#22762=EDGE_CURVE('',#18400,#18401,#7950,.T.);
#22763=EDGE_CURVE('',#18401,#18396,#7951,.T.);
#22764=EDGE_CURVE('',#18401,#18402,#7952,.T.);
#22765=EDGE_CURVE('',#18400,#18403,#7953,.T.);
#22766=EDGE_CURVE('',#18402,#18403,#7954,.T.);
#22767=EDGE_CURVE('',#18402,#18394,#7955,.T.);
#22768=EDGE_CURVE('',#18403,#18395,#7956,.T.);
#22769=EDGE_CURVE('',#18398,#18392,#7957,.T.);
#22770=EDGE_CURVE('',#18397,#18393,#7958,.T.);
#22771=EDGE_CURVE('',#18404,#18276,#7959,.T.);
#22772=EDGE_CURVE('',#18404,#18405,#7960,.T.);
#22773=EDGE_CURVE('',#18405,#18277,#7961,.T.);
#22774=EDGE_CURVE('',#18406,#18279,#7962,.T.);
#22775=EDGE_CURVE('',#18404,#18406,#7963,.T.);
#22776=EDGE_CURVE('',#18407,#18278,#7964,.T.);
#22777=EDGE_CURVE('',#18407,#18406,#7965,.T.);
#22778=EDGE_CURVE('',#18407,#18405,#7966,.T.);
#22779=EDGE_CURVE('',#18408,#18409,#7967,.T.);
#22780=EDGE_CURVE('',#18408,#18410,#7968,.T.);
#22781=EDGE_CURVE('',#18410,#18411,#7969,.T.);
#22782=EDGE_CURVE('',#18411,#18409,#7970,.T.);
#22783=EDGE_CURVE('',#18412,#18413,#7971,.T.);
#22784=EDGE_CURVE('',#18413,#18414,#7972,.T.);
#22785=EDGE_CURVE('',#18415,#18414,#7973,.T.);
#22786=EDGE_CURVE('',#18412,#18415,#7974,.T.);
#22787=EDGE_CURVE('',#18412,#18416,#7975,.T.);
#22788=EDGE_CURVE('',#18417,#18415,#7976,.T.);
#22789=EDGE_CURVE('',#18416,#18417,#7977,.T.);
#22790=EDGE_CURVE('',#18418,#18419,#7978,.T.);
#22791=EDGE_CURVE('',#18419,#18414,#7979,.T.);
#22792=EDGE_CURVE('',#18413,#18418,#7980,.T.);
#22793=EDGE_CURVE('',#18419,#18411,#7981,.T.);
#22794=EDGE_CURVE('',#18418,#18409,#7982,.T.);
#22795=EDGE_CURVE('',#18416,#18408,#7983,.T.);
#22796=EDGE_CURVE('',#18417,#18410,#7984,.T.);
#22797=EDGE_CURVE('',#18420,#18421,#7985,.T.);
#22798=EDGE_CURVE('',#18420,#18422,#7986,.T.);
#22799=EDGE_CURVE('',#18423,#18422,#7987,.T.);
#22800=EDGE_CURVE('',#18423,#18421,#7988,.T.);
#22801=EDGE_CURVE('',#18424,#18425,#7989,.T.);
#22802=EDGE_CURVE('',#18424,#18426,#7990,.T.);
#22803=EDGE_CURVE('',#18426,#18427,#7991,.T.);
#22804=EDGE_CURVE('',#18427,#18425,#7992,.T.);
#22805=EDGE_CURVE('',#18420,#18272,#7993,.T.);
#22806=EDGE_CURVE('',#18421,#18273,#7994,.T.);
#22807=EDGE_CURVE('',#18422,#18275,#7995,.T.);
#22808=EDGE_CURVE('',#18423,#18274,#7996,.T.);
#22809=EDGE_CURVE('',#18428,#18429,#7997,.T.);
#22810=EDGE_CURVE('',#18428,#18430,#7998,.T.);
#22811=EDGE_CURVE('',#18430,#18431,#7999,.T.);
#22812=EDGE_CURVE('',#18429,#18431,#8000,.T.);
#22813=EDGE_CURVE('',#18432,#18433,#8001,.T.);
#22814=EDGE_CURVE('',#18431,#18433,#8002,.T.);
#22815=EDGE_CURVE('',#18430,#18432,#8003,.T.);
#22816=EDGE_CURVE('',#18429,#18434,#8004,.T.);
#22817=EDGE_CURVE('',#18435,#18434,#8005,.T.);
#22818=EDGE_CURVE('',#18428,#18435,#8006,.T.);
#22819=EDGE_CURVE('',#18435,#18427,#8007,.T.);
#22820=EDGE_CURVE('',#18434,#18425,#8008,.T.);
#22821=EDGE_CURVE('',#18433,#18424,#8009,.T.);
#22822=EDGE_CURVE('',#18432,#18426,#8010,.T.);
#22823=EDGE_CURVE('',#18436,#18437,#8011,.T.);
#22824=EDGE_CURVE('',#18438,#18436,#8012,.T.);
#22825=EDGE_CURVE('',#18439,#18438,#8013,.T.);
#22826=EDGE_CURVE('',#18437,#18439,#8014,.T.);
#22827=EDGE_CURVE('',#18440,#18441,#8015,.T.);
#22828=EDGE_CURVE('',#18441,#18442,#8016,.T.);
#22829=EDGE_CURVE('',#18442,#18443,#8017,.T.);
#22830=EDGE_CURVE('',#18443,#18440,#8018,.T.);
#22831=EDGE_CURVE('',#18441,#18439,#8019,.T.);
#22832=EDGE_CURVE('',#18440,#18437,#8020,.T.);
#22833=EDGE_CURVE('',#18443,#18436,#8021,.T.);
#22834=EDGE_CURVE('',#18442,#18438,#8022,.T.);
#22835=EDGE_CURVE('',#18444,#18444,#17094,.T.);
#22836=EDGE_CURVE('',#18444,#18445,#8023,.T.);
#22837=EDGE_CURVE('',#18445,#18445,#17095,.T.);
#22838=EDGE_CURVE('',#18446,#18446,#17096,.T.);
#22839=EDGE_CURVE('',#18446,#18447,#8024,.T.);
#22840=EDGE_CURVE('',#18447,#18447,#17097,.T.);
#22841=EDGE_CURVE('',#18448,#18449,#17098,.T.);
#22842=EDGE_CURVE('',#18448,#18450,#8025,.T.);
#22843=EDGE_CURVE('',#18450,#18451,#17099,.T.);
#22844=EDGE_CURVE('',#18451,#18449,#8026,.T.);
#22845=EDGE_CURVE('',#18452,#18453,#8027,.T.);
#22846=EDGE_CURVE('',#18454,#18452,#8028,.T.);
#22847=EDGE_CURVE('',#18454,#18455,#8029,.T.);
#22848=EDGE_CURVE('',#18455,#18453,#8030,.T.);
#22849=EDGE_CURVE('',#18456,#18457,#8031,.T.);
#22850=EDGE_CURVE('',#18457,#18458,#8032,.T.);
#22851=EDGE_CURVE('',#18459,#18458,#8033,.T.);
#22852=EDGE_CURVE('',#18456,#18459,#8034,.T.);
#22853=EDGE_CURVE('',#18460,#18452,#8035,.T.);
#22854=EDGE_CURVE('',#18453,#18461,#8036,.T.);
#22855=EDGE_CURVE('',#18462,#18461,#8037,.T.);
#22856=EDGE_CURVE('',#18463,#18462,#8038,.T.);
#22857=EDGE_CURVE('',#18460,#18463,#8039,.T.);
#22858=EDGE_CURVE('',#18464,#18457,#8040,.T.);
#22859=EDGE_CURVE('',#18464,#18465,#8041,.T.);
#22860=EDGE_CURVE('',#18465,#18466,#8042,.T.);
#22861=EDGE_CURVE('',#18466,#18467,#8043,.T.);
#22862=EDGE_CURVE('',#18458,#18467,#8044,.T.);
#22863=EDGE_CURVE('',#18468,#18469,#8045,.T.);
#22864=EDGE_CURVE('',#18469,#18470,#8046,.T.);
#22865=EDGE_CURVE('',#18471,#18470,#8047,.T.);
#22866=EDGE_CURVE('',#18468,#18471,#8048,.T.);
#22867=EDGE_CURVE('',#18472,#18473,#8049,.T.);
#22868=EDGE_CURVE('',#18474,#18472,#8050,.T.);
#22869=EDGE_CURVE('',#18474,#18475,#8051,.T.);
#22870=EDGE_CURVE('',#18475,#18473,#8052,.T.);
#22871=EDGE_CURVE('',#18476,#18469,#8053,.T.);
#22872=EDGE_CURVE('',#18476,#18477,#8054,.T.);
#22873=EDGE_CURVE('',#18477,#18478,#8055,.T.);
#22874=EDGE_CURVE('',#18478,#18479,#8056,.T.);
#22875=EDGE_CURVE('',#18470,#18479,#8057,.T.);
#22876=EDGE_CURVE('',#18480,#18472,#8058,.T.);
#22877=EDGE_CURVE('',#18473,#18481,#8059,.T.);
#22878=EDGE_CURVE('',#18482,#18481,#8060,.T.);
#22879=EDGE_CURVE('',#18483,#18482,#8061,.T.);
#22880=EDGE_CURVE('',#18480,#18483,#8062,.T.);
#22881=EDGE_CURVE('',#18484,#18485,#8063,.T.);
#22882=EDGE_CURVE('',#18485,#18486,#8064,.T.);
#22883=EDGE_CURVE('',#18486,#18487,#8065,.T.);
#22884=EDGE_CURVE('',#18487,#18484,#8066,.T.);
#22885=EDGE_CURVE('',#18488,#18489,#8067,.T.);
#22886=EDGE_CURVE('',#18461,#18488,#8068,.T.);
#22887=EDGE_CURVE('',#18455,#18459,#8069,.T.);
#22888=EDGE_CURVE('',#18467,#18489,#8070,.T.);
#22889=EDGE_CURVE('',#18490,#18491,#8071,.T.);
#22890=EDGE_CURVE('',#18481,#18490,#8072,.T.);
#22891=EDGE_CURVE('',#18475,#18471,#8073,.T.);
#22892=EDGE_CURVE('',#18479,#18491,#8074,.T.);
#22893=EDGE_CURVE('',#18492,#18493,#8075,.T.);
#22894=EDGE_CURVE('',#18494,#18493,#8076,.T.);
#22895=EDGE_CURVE('',#18495,#18494,#8077,.T.);
#22896=EDGE_CURVE('',#18495,#18492,#8078,.T.);
#22897=EDGE_CURVE('',#18496,#18497,#8079,.T.);
#22898=EDGE_CURVE('',#18498,#18496,#8080,.T.);
#22899=EDGE_CURVE('',#18499,#18498,#8081,.T.);
#22900=EDGE_CURVE('',#18500,#18499,#8082,.T.);
#22901=EDGE_CURVE('',#18500,#18501,#8083,.T.);
#22902=EDGE_CURVE('',#18501,#18502,#8084,.T.);
#22903=EDGE_CURVE('',#18503,#18502,#8085,.T.);
#22904=EDGE_CURVE('',#18504,#18503,#8086,.T.);
#22905=EDGE_CURVE('',#18505,#18504,#8087,.T.);
#22906=EDGE_CURVE('',#18505,#18497,#8088,.T.);
#22907=EDGE_CURVE('',#18506,#18494,#8089,.T.);
#22908=EDGE_CURVE('',#18507,#18506,#8090,.T.);
#22909=EDGE_CURVE('',#18507,#18495,#8091,.T.);
#22910=EDGE_CURVE('',#18508,#18493,#8092,.T.);
#22911=EDGE_CURVE('',#18506,#18508,#8093,.T.);
#22912=EDGE_CURVE('',#18509,#18492,#8094,.T.);
#22913=EDGE_CURVE('',#18509,#18508,#8095,.T.);
#22914=EDGE_CURVE('',#18507,#18509,#8096,.T.);
#22915=EDGE_CURVE('',#18510,#18511,#8097,.T.);
#22916=EDGE_CURVE('',#18512,#18510,#8098,.T.);
#22917=EDGE_CURVE('',#18513,#18512,#8099,.T.);
#22918=EDGE_CURVE('',#18511,#18513,#8100,.T.);
#22919=EDGE_CURVE('',#18514,#18504,#17100,.T.);
#22920=EDGE_CURVE('',#18504,#18514,#17101,.T.);
#22921=EDGE_CURVE('',#18503,#18515,#8101,.T.);
#22922=EDGE_CURVE('',#18515,#18516,#8102,.T.);
#22923=EDGE_CURVE('',#18516,#18503,#8103,.T.);
#22924=EDGE_CURVE('',#18502,#18517,#8104,.T.);
#22925=EDGE_CURVE('',#18517,#18518,#8105,.T.);
#22926=EDGE_CURVE('',#18485,#18518,#8106,.T.);
#22927=EDGE_CURVE('',#18484,#18519,#8107,.T.);
#22928=EDGE_CURVE('',#18520,#18519,#8108,.T.);
#22929=EDGE_CURVE('',#18497,#18520,#8109,.T.);
#22930=EDGE_CURVE('',#18521,#18505,#8110,.T.);
#22931=EDGE_CURVE('',#18522,#18521,#8111,.T.);
#22932=EDGE_CURVE('',#18522,#18505,#8112,.T.);
#22933=EDGE_CURVE('',#18523,#18518,#8113,.T.);
#22934=EDGE_CURVE('',#18486,#18523,#8114,.T.);
#22935=EDGE_CURVE('',#18524,#18499,#17102,.T.);
#22936=EDGE_CURVE('',#18499,#18524,#17103,.T.);
#22937=EDGE_CURVE('',#18498,#18525,#8115,.T.);
#22938=EDGE_CURVE('',#18525,#18526,#8116,.T.);
#22939=EDGE_CURVE('',#18526,#18498,#8117,.T.);
#22940=EDGE_CURVE('',#18496,#18527,#8118,.T.);
#22941=EDGE_CURVE('',#18527,#18528,#8119,.T.);
#22942=EDGE_CURVE('',#18487,#18528,#8120,.T.);
#22943=EDGE_CURVE('',#18529,#18523,#8121,.T.);
#22944=EDGE_CURVE('',#18501,#18529,#8122,.T.);
#22945=EDGE_CURVE('',#18530,#18500,#8123,.T.);
#22946=EDGE_CURVE('',#18531,#18530,#8124,.T.);
#22947=EDGE_CURVE('',#18531,#18500,#8125,.T.);
#22948=EDGE_CURVE('',#18528,#18519,#8126,.T.);
#22949=EDGE_CURVE('',#18454,#18456,#8127,.T.);
#22950=EDGE_CURVE('',#18462,#18532,#8128,.T.);
#22951=EDGE_CURVE('',#18532,#18488,#8129,.T.);
#22952=EDGE_CURVE('',#18466,#18533,#8130,.T.);
#22953=EDGE_CURVE('',#18533,#18489,#8131,.T.);
#22954=EDGE_CURVE('',#18452,#18534,#8132,.T.);
#22955=EDGE_CURVE('',#18535,#18534,#8133,.T.);
#22956=EDGE_CURVE('',#18462,#18535,#8134,.T.);
#22957=EDGE_CURVE('',#18532,#18533,#8135,.T.);
#22958=EDGE_CURVE('',#18536,#18466,#8136,.T.);
#22959=EDGE_CURVE('',#18536,#18537,#8137,.T.);
#22960=EDGE_CURVE('',#18537,#18457,#8138,.T.);
#22961=EDGE_CURVE('',#18474,#18468,#8139,.T.);
#22962=EDGE_CURVE('',#18482,#18538,#8140,.T.);
#22963=EDGE_CURVE('',#18538,#18490,#8141,.T.);
#22964=EDGE_CURVE('',#18478,#18539,#8142,.T.);
#22965=EDGE_CURVE('',#18539,#18491,#8143,.T.);
#22966=EDGE_CURVE('',#18472,#18540,#8144,.T.);
#22967=EDGE_CURVE('',#18541,#18540,#8145,.T.);
#22968=EDGE_CURVE('',#18482,#18541,#8146,.T.);
#22969=EDGE_CURVE('',#18538,#18539,#8147,.T.);
#22970=EDGE_CURVE('',#18542,#18478,#8148,.T.);
#22971=EDGE_CURVE('',#18542,#18543,#8149,.T.);
#22972=EDGE_CURVE('',#18543,#18469,#8150,.T.);
#22973=EDGE_CURVE('',#18534,#18537,#17104,.T.);
#22974=EDGE_CURVE('',#18544,#18460,#8151,.T.);
#22975=EDGE_CURVE('',#18544,#18545,#8152,.T.);
#22976=EDGE_CURVE('',#18464,#18545,#8153,.T.);
#22977=EDGE_CURVE('',#18535,#18536,#17105,.T.);
#22978=EDGE_CURVE('',#18465,#18546,#8154,.T.);
#22979=EDGE_CURVE('',#18547,#18546,#8155,.T.);
#22980=EDGE_CURVE('',#18547,#18463,#8156,.T.);
#22981=EDGE_CURVE('',#18545,#18546,#8157,.T.);
#22982=EDGE_CURVE('',#18544,#18547,#8158,.T.);
#22983=EDGE_CURVE('',#18540,#18543,#17106,.T.);
#22984=EDGE_CURVE('',#18548,#18480,#8159,.T.);
#22985=EDGE_CURVE('',#18548,#18549,#8160,.T.);
#22986=EDGE_CURVE('',#18476,#18549,#8161,.T.);
#22987=EDGE_CURVE('',#18541,#18542,#17107,.T.);
#22988=EDGE_CURVE('',#18550,#18477,#8162,.T.);
#22989=EDGE_CURVE('',#18551,#18550,#8163,.T.);
#22990=EDGE_CURVE('',#18483,#18551,#8164,.T.);
#22991=EDGE_CURVE('',#18549,#18550,#8165,.T.);
#22992=EDGE_CURVE('',#18551,#18548,#8166,.T.);
#22993=EDGE_CURVE('',#18525,#18522,#8167,.T.);
#22994=EDGE_CURVE('',#18498,#18505,#8168,.T.);
#22995=EDGE_CURVE('',#18500,#18503,#8169,.T.);
#22996=EDGE_CURVE('',#18531,#18515,#8170,.T.);
#22997=EDGE_CURVE('',#18530,#18516,#8171,.T.);
#22998=EDGE_CURVE('',#18529,#18517,#8172,.T.);
#22999=EDGE_CURVE('',#18527,#18520,#8173,.T.);
#23000=EDGE_CURVE('',#18526,#18521,#8174,.T.);
#23001=EDGE_CURVE('',#18450,#18512,#8175,.T.);
#23002=EDGE_CURVE('',#18448,#18513,#8176,.T.);
#23003=EDGE_CURVE('',#18451,#18510,#8177,.T.);
#23004=EDGE_CURVE('',#18449,#18511,#8178,.T.);
#23005=EDGE_CURVE('',#18514,#18552,#17108,.T.);
#23006=EDGE_CURVE('',#18524,#18553,#17109,.T.);
#23007=EDGE_CURVE('',#18554,#18554,#17110,.T.);
#23008=EDGE_CURVE('',#18554,#18555,#17111,.T.);
#23009=EDGE_CURVE('',#18555,#18555,#17112,.T.);
#23010=EDGE_CURVE('',#18556,#18556,#17113,.T.);
#23011=EDGE_CURVE('',#18556,#18557,#17114,.T.);
#23012=EDGE_CURVE('',#18557,#18557,#17115,.T.);
#23013=EDGE_CURVE('',#18558,#18558,#17116,.T.);
#23014=EDGE_CURVE('',#18558,#18556,#17117,.T.);
#23015=EDGE_CURVE('',#18559,#18559,#17118,.T.);
#23016=EDGE_CURVE('',#18559,#18554,#17119,.T.);
#23017=EDGE_CURVE('',#18560,#18561,#8179,.T.);
#23018=EDGE_CURVE('',#18562,#18560,#8180,.T.);
#23019=EDGE_CURVE('',#18562,#18563,#8181,.T.);
#23020=EDGE_CURVE('',#18564,#18563,#8182,.T.);
#23021=EDGE_CURVE('',#18564,#18565,#8183,.T.);
#23022=EDGE_CURVE('',#18565,#18566,#8184,.T.);
#23023=EDGE_CURVE('',#18567,#18566,#8185,.T.);
#23024=EDGE_CURVE('',#18567,#18568,#8186,.T.);
#23025=EDGE_CURVE('',#18568,#18569,#8187,.T.);
#23026=EDGE_CURVE('',#18569,#18570,#8188,.T.);
#23027=EDGE_CURVE('',#18571,#18570,#8189,.T.);
#23028=EDGE_CURVE('',#18561,#18571,#8190,.T.);
#23029=EDGE_CURVE('',#18572,#18573,#8191,.T.);
#23030=EDGE_CURVE('',#18574,#18572,#8192,.T.);
#23031=EDGE_CURVE('',#18574,#18575,#8193,.T.);
#23032=EDGE_CURVE('',#18575,#18576,#8194,.T.);
#23033=EDGE_CURVE('',#18577,#18576,#8195,.T.);
#23034=EDGE_CURVE('',#18577,#18578,#8196,.T.);
#23035=EDGE_CURVE('',#18578,#18579,#8197,.T.);
#23036=EDGE_CURVE('',#18580,#18579,#8198,.T.);
#23037=EDGE_CURVE('',#18581,#18580,#8199,.T.);
#23038=EDGE_CURVE('',#18582,#18581,#8200,.T.);
#23039=EDGE_CURVE('',#18582,#18583,#8201,.T.);
#23040=EDGE_CURVE('',#18583,#18573,#8202,.T.);
#23041=EDGE_CURVE('',#18570,#18576,#8203,.T.);
#23042=EDGE_CURVE('',#18575,#18571,#8204,.T.);
#23043=EDGE_CURVE('',#18564,#18582,#8205,.T.);
#23044=EDGE_CURVE('',#18581,#18565,#8206,.T.);
#23045=EDGE_CURVE('',#18574,#18561,#8207,.T.);
#23046=EDGE_CURVE('',#18560,#18572,#8208,.T.);
#23047=EDGE_CURVE('',#18563,#18583,#8209,.T.);
#23048=EDGE_CURVE('',#18562,#18573,#8210,.T.);
#23049=EDGE_CURVE('',#18569,#18577,#8211,.T.);
#23050=EDGE_CURVE('',#18568,#18578,#8212,.T.);
#23051=EDGE_CURVE('',#18567,#18579,#8213,.T.);
#23052=EDGE_CURVE('',#18580,#18566,#8214,.T.);
#23053=EDGE_CURVE('',#18584,#18585,#8215,.T.);
#23054=EDGE_CURVE('',#18585,#18569,#17120,.T.);
#23055=EDGE_CURVE('',#18584,#18577,#17121,.T.);
#23056=EDGE_CURVE('',#18570,#18586,#17122,.T.);
#23057=EDGE_CURVE('',#18587,#18586,#8216,.T.);
#23058=EDGE_CURVE('',#18576,#18587,#17123,.T.);
#23059=EDGE_CURVE('',#18584,#18587,#8217,.T.);
#23060=EDGE_CURVE('',#18585,#18586,#8218,.T.);
#23061=EDGE_CURVE('',#18566,#18588,#17124,.T.);
#23062=EDGE_CURVE('',#18588,#18589,#8219,.T.);
#23063=EDGE_CURVE('',#18580,#18589,#17125,.T.);
#23064=EDGE_CURVE('',#18590,#18591,#8220,.T.);
#23065=EDGE_CURVE('',#18590,#18565,#17126,.T.);
#23066=EDGE_CURVE('',#18591,#18581,#17127,.T.);
#23067=EDGE_CURVE('',#18591,#18589,#8221,.T.);
#23068=EDGE_CURVE('',#18590,#18588,#8222,.T.);
#23069=EDGE_CURVE('',#18592,#18593,#17128,.T.);
#23070=EDGE_CURVE('',#18594,#18592,#8223,.T.);
#23071=EDGE_CURVE('',#18595,#18594,#17129,.T.);
#23072=EDGE_CURVE('',#18593,#18595,#8224,.T.);
#23073=EDGE_CURVE('',#18596,#18597,#8225,.T.);
#23074=EDGE_CURVE('',#18597,#18598,#8226,.T.);
#23075=EDGE_CURVE('',#18598,#18599,#8227,.T.);
#23076=EDGE_CURVE('',#18596,#18599,#8228,.T.);
#23077=EDGE_CURVE('',#18600,#18601,#17130,.T.);
#23078=EDGE_CURVE('',#18602,#18600,#8229,.T.);
#23079=EDGE_CURVE('',#18603,#18602,#17131,.T.);
#23080=EDGE_CURVE('',#18601,#18603,#8230,.T.);
#23081=EDGE_CURVE('',#18602,#18595,#8231,.T.);
#23082=EDGE_CURVE('',#18600,#18593,#8232,.T.);
#23083=EDGE_CURVE('',#18591,#18601,#8233,.T.);
#23084=EDGE_CURVE('',#18599,#18589,#8234,.T.);
#23085=EDGE_CURVE('',#18598,#18584,#8235,.T.);
#23086=EDGE_CURVE('',#18587,#18592,#8236,.T.);
#23087=EDGE_CURVE('',#18588,#18596,#8237,.T.);
#23088=EDGE_CURVE('',#18590,#18603,#8238,.T.);
#23089=EDGE_CURVE('',#18586,#18594,#8239,.T.);
#23090=EDGE_CURVE('',#18585,#18597,#8240,.T.);
#23091=EDGE_CURVE('',#18604,#18605,#8241,.T.);
#23092=EDGE_CURVE('',#18605,#18563,#17132,.T.);
#23093=EDGE_CURVE('',#18604,#18583,#17133,.T.);
#23094=EDGE_CURVE('',#18564,#18606,#17134,.T.);
#23095=EDGE_CURVE('',#18607,#18606,#8242,.T.);
#23096=EDGE_CURVE('',#18582,#18607,#17135,.T.);
#23097=EDGE_CURVE('',#18607,#18604,#8243,.T.);
#23098=EDGE_CURVE('',#18606,#18605,#8244,.T.);
#23099=EDGE_CURVE('',#18561,#18608,#17136,.T.);
#23100=EDGE_CURVE('',#18608,#18609,#8245,.T.);
#23101=EDGE_CURVE('',#18574,#18609,#17137,.T.);
#23102=EDGE_CURVE('',#18610,#18611,#8246,.T.);
#23103=EDGE_CURVE('',#18610,#18571,#17138,.T.);
#23104=EDGE_CURVE('',#18611,#18575,#17139,.T.);
#23105=EDGE_CURVE('',#18609,#18611,#8247,.T.);
#23106=EDGE_CURVE('',#18608,#18610,#8248,.T.);
#23107=EDGE_CURVE('',#18612,#18613,#17140,.T.);
#23108=EDGE_CURVE('',#18614,#18612,#8249,.T.);
#23109=EDGE_CURVE('',#18615,#18614,#17141,.T.);
#23110=EDGE_CURVE('',#18613,#18615,#8250,.T.);
#23111=EDGE_CURVE('',#18616,#18617,#8251,.T.);
#23112=EDGE_CURVE('',#18618,#18617,#8252,.T.);
#23113=EDGE_CURVE('',#18619,#18618,#8253,.T.);
#23114=EDGE_CURVE('',#18616,#18619,#8254,.T.);
#23115=EDGE_CURVE('',#18620,#18621,#17142,.T.);
#23116=EDGE_CURVE('',#18622,#18620,#8255,.T.);
#23117=EDGE_CURVE('',#18623,#18622,#17143,.T.);
#23118=EDGE_CURVE('',#18621,#18623,#8256,.T.);
#23119=EDGE_CURVE('',#18612,#18621,#8257,.T.);
#23120=EDGE_CURVE('',#18614,#18623,#8258,.T.);
#23121=EDGE_CURVE('',#18622,#18611,#8259,.T.);
#23122=EDGE_CURVE('',#18618,#18609,#8260,.T.);
#23123=EDGE_CURVE('',#18617,#18604,#8261,.T.);
#23124=EDGE_CURVE('',#18615,#18607,#8262,.T.);
#23125=EDGE_CURVE('',#18608,#18619,#8263,.T.);
#23126=EDGE_CURVE('',#18620,#18610,#8264,.T.);
#23127=EDGE_CURVE('',#18613,#18606,#8265,.T.);
#23128=EDGE_CURVE('',#18605,#18616,#8266,.T.);
#23129=EDGE_CURVE('',#18624,#18625,#8267,.T.);
#23130=EDGE_CURVE('',#18626,#18624,#8268,.T.);
#23131=EDGE_CURVE('',#18627,#18626,#8269,.T.);
#23132=EDGE_CURVE('',#18628,#18627,#8270,.T.);
#23133=EDGE_CURVE('',#18629,#18628,#8271,.T.);
#23134=EDGE_CURVE('',#18625,#18629,#8272,.T.);
#23135=EDGE_CURVE('',#18630,#18631,#8273,.T.);
#23136=EDGE_CURVE('',#18632,#18630,#8274,.T.);
#23137=EDGE_CURVE('',#18633,#18632,#8275,.T.);
#23138=EDGE_CURVE('',#18634,#18633,#8276,.T.);
#23139=EDGE_CURVE('',#18635,#18634,#8277,.T.);
#23140=EDGE_CURVE('',#18631,#18635,#8278,.T.);
#23141=EDGE_CURVE('',#18636,#18637,#8279,.T.);
#23142=EDGE_CURVE('',#18638,#18636,#8280,.T.);
#23143=EDGE_CURVE('',#18639,#18638,#8281,.T.);
#23144=EDGE_CURVE('',#18640,#18639,#8282,.T.);
#23145=EDGE_CURVE('',#18641,#18640,#8283,.T.);
#23146=EDGE_CURVE('',#18637,#18641,#8284,.T.);
#23147=EDGE_CURVE('',#18642,#18643,#8285,.T.);
#23148=EDGE_CURVE('',#18644,#18642,#8286,.T.);
#23149=EDGE_CURVE('',#18645,#18644,#8287,.T.);
#23150=EDGE_CURVE('',#18646,#18645,#8288,.T.);
#23151=EDGE_CURVE('',#18647,#18646,#8289,.T.);
#23152=EDGE_CURVE('',#18643,#18647,#8290,.T.);
#23153=EDGE_CURVE('',#18648,#18649,#8291,.T.);
#23154=EDGE_CURVE('',#18650,#18648,#8292,.T.);
#23155=EDGE_CURVE('',#18651,#18650,#8293,.T.);
#23156=EDGE_CURVE('',#18652,#18651,#8294,.T.);
#23157=EDGE_CURVE('',#18653,#18652,#8295,.T.);
#23158=EDGE_CURVE('',#18649,#18653,#8296,.T.);
#23159=EDGE_CURVE('',#18654,#18655,#8297,.T.);
#23160=EDGE_CURVE('',#18656,#18654,#8298,.T.);
#23161=EDGE_CURVE('',#18657,#18656,#8299,.T.);
#23162=EDGE_CURVE('',#18658,#18657,#8300,.T.);
#23163=EDGE_CURVE('',#18659,#18658,#8301,.T.);
#23164=EDGE_CURVE('',#18655,#18659,#8302,.T.);
#23165=EDGE_CURVE('',#18660,#18661,#8303,.T.);
#23166=EDGE_CURVE('',#18662,#18660,#8304,.T.);
#23167=EDGE_CURVE('',#18663,#18662,#8305,.T.);
#23168=EDGE_CURVE('',#18664,#18663,#8306,.T.);
#23169=EDGE_CURVE('',#18665,#18664,#8307,.T.);
#23170=EDGE_CURVE('',#18661,#18665,#8308,.T.);
#23171=EDGE_CURVE('',#18666,#18667,#8309,.T.);
#23172=EDGE_CURVE('',#18668,#18666,#8310,.T.);
#23173=EDGE_CURVE('',#18669,#18668,#8311,.T.);
#23174=EDGE_CURVE('',#18670,#18669,#8312,.T.);
#23175=EDGE_CURVE('',#18671,#18670,#8313,.T.);
#23176=EDGE_CURVE('',#18667,#18671,#8314,.T.);
#23177=EDGE_CURVE('',#18672,#18673,#8315,.T.);
#23178=EDGE_CURVE('',#18674,#18672,#8316,.T.);
#23179=EDGE_CURVE('',#18675,#18674,#8317,.T.);
#23180=EDGE_CURVE('',#18676,#18675,#8318,.T.);
#23181=EDGE_CURVE('',#18677,#18676,#8319,.T.);
#23182=EDGE_CURVE('',#18673,#18677,#8320,.T.);
#23183=EDGE_CURVE('',#18678,#18679,#8321,.T.);
#23184=EDGE_CURVE('',#18680,#18678,#8322,.T.);
#23185=EDGE_CURVE('',#18681,#18680,#8323,.T.);
#23186=EDGE_CURVE('',#18682,#18681,#8324,.T.);
#23187=EDGE_CURVE('',#18683,#18682,#8325,.T.);
#23188=EDGE_CURVE('',#18679,#18683,#8326,.T.);
#23189=EDGE_CURVE('',#18684,#18685,#8327,.T.);
#23190=EDGE_CURVE('',#18686,#18684,#8328,.T.);
#23191=EDGE_CURVE('',#18687,#18686,#8329,.T.);
#23192=EDGE_CURVE('',#18688,#18687,#8330,.T.);
#23193=EDGE_CURVE('',#18689,#18688,#8331,.T.);
#23194=EDGE_CURVE('',#18685,#18689,#8332,.T.);
#23195=EDGE_CURVE('',#18690,#18691,#8333,.T.);
#23196=EDGE_CURVE('',#18692,#18690,#8334,.T.);
#23197=EDGE_CURVE('',#18693,#18692,#8335,.T.);
#23198=EDGE_CURVE('',#18694,#18693,#8336,.T.);
#23199=EDGE_CURVE('',#18695,#18694,#8337,.T.);
#23200=EDGE_CURVE('',#18691,#18695,#8338,.T.);
#23201=EDGE_CURVE('',#18696,#18697,#8339,.T.);
#23202=EDGE_CURVE('',#18698,#18696,#8340,.T.);
#23203=EDGE_CURVE('',#18699,#18698,#8341,.T.);
#23204=EDGE_CURVE('',#18700,#18699,#8342,.T.);
#23205=EDGE_CURVE('',#18701,#18700,#8343,.T.);
#23206=EDGE_CURVE('',#18697,#18701,#8344,.T.);
#23207=EDGE_CURVE('',#18702,#18703,#8345,.T.);
#23208=EDGE_CURVE('',#18704,#18702,#8346,.T.);
#23209=EDGE_CURVE('',#18705,#18704,#8347,.T.);
#23210=EDGE_CURVE('',#18706,#18705,#8348,.T.);
#23211=EDGE_CURVE('',#18707,#18706,#8349,.T.);
#23212=EDGE_CURVE('',#18703,#18707,#8350,.T.);
#23213=EDGE_CURVE('',#18708,#18709,#8351,.T.);
#23214=EDGE_CURVE('',#18710,#18708,#8352,.T.);
#23215=EDGE_CURVE('',#18711,#18710,#8353,.T.);
#23216=EDGE_CURVE('',#18712,#18711,#8354,.T.);
#23217=EDGE_CURVE('',#18713,#18712,#8355,.T.);
#23218=EDGE_CURVE('',#18709,#18713,#8356,.T.);
#23219=EDGE_CURVE('',#18714,#18715,#8357,.T.);
#23220=EDGE_CURVE('',#18716,#18714,#8358,.T.);
#23221=EDGE_CURVE('',#18717,#18716,#8359,.T.);
#23222=EDGE_CURVE('',#18718,#18717,#8360,.T.);
#23223=EDGE_CURVE('',#18719,#18718,#8361,.T.);
#23224=EDGE_CURVE('',#18715,#18719,#8362,.T.);
#23225=EDGE_CURVE('',#18720,#18721,#8363,.T.);
#23226=EDGE_CURVE('',#18722,#18720,#8364,.T.);
#23227=EDGE_CURVE('',#18723,#18722,#8365,.T.);
#23228=EDGE_CURVE('',#18724,#18723,#8366,.T.);
#23229=EDGE_CURVE('',#18725,#18724,#8367,.T.);
#23230=EDGE_CURVE('',#18721,#18725,#8368,.T.);
#23231=EDGE_CURVE('',#18726,#18727,#8369,.T.);
#23232=EDGE_CURVE('',#18728,#18726,#8370,.T.);
#23233=EDGE_CURVE('',#18729,#18728,#8371,.T.);
#23234=EDGE_CURVE('',#18730,#18729,#8372,.T.);
#23235=EDGE_CURVE('',#18731,#18730,#8373,.T.);
#23236=EDGE_CURVE('',#18727,#18731,#8374,.T.);
#23237=EDGE_CURVE('',#18732,#18733,#8375,.T.);
#23238=EDGE_CURVE('',#18734,#18732,#8376,.T.);
#23239=EDGE_CURVE('',#18735,#18734,#8377,.T.);
#23240=EDGE_CURVE('',#18736,#18735,#8378,.T.);
#23241=EDGE_CURVE('',#18737,#18736,#8379,.T.);
#23242=EDGE_CURVE('',#18733,#18737,#8380,.T.);
#23243=EDGE_CURVE('',#18738,#18739,#8381,.T.);
#23244=EDGE_CURVE('',#18740,#18738,#8382,.T.);
#23245=EDGE_CURVE('',#18741,#18740,#8383,.T.);
#23246=EDGE_CURVE('',#18742,#18741,#8384,.T.);
#23247=EDGE_CURVE('',#18743,#18742,#8385,.T.);
#23248=EDGE_CURVE('',#18739,#18743,#8386,.T.);
#23249=EDGE_CURVE('',#18744,#18745,#8387,.T.);
#23250=EDGE_CURVE('',#18746,#18744,#8388,.T.);
#23251=EDGE_CURVE('',#18747,#18746,#8389,.T.);
#23252=EDGE_CURVE('',#18748,#18747,#8390,.T.);
#23253=EDGE_CURVE('',#18749,#18748,#8391,.T.);
#23254=EDGE_CURVE('',#18745,#18749,#8392,.T.);
#23255=EDGE_CURVE('',#18750,#18751,#8393,.T.);
#23256=EDGE_CURVE('',#18752,#18750,#8394,.T.);
#23257=EDGE_CURVE('',#18753,#18752,#8395,.T.);
#23258=EDGE_CURVE('',#18754,#18753,#8396,.T.);
#23259=EDGE_CURVE('',#18755,#18754,#8397,.T.);
#23260=EDGE_CURVE('',#18751,#18755,#8398,.T.);
#23261=EDGE_CURVE('',#18756,#18757,#8399,.T.);
#23262=EDGE_CURVE('',#18758,#18756,#8400,.T.);
#23263=EDGE_CURVE('',#18759,#18758,#8401,.T.);
#23264=EDGE_CURVE('',#18760,#18759,#8402,.T.);
#23265=EDGE_CURVE('',#18761,#18760,#8403,.T.);
#23266=EDGE_CURVE('',#18757,#18761,#8404,.T.);
#23267=EDGE_CURVE('',#18762,#18763,#8405,.T.);
#23268=EDGE_CURVE('',#18764,#18762,#8406,.T.);
#23269=EDGE_CURVE('',#18765,#18764,#8407,.T.);
#23270=EDGE_CURVE('',#18766,#18765,#8408,.T.);
#23271=EDGE_CURVE('',#18767,#18766,#8409,.T.);
#23272=EDGE_CURVE('',#18763,#18767,#8410,.T.);
#23273=EDGE_CURVE('',#18768,#18769,#8411,.T.);
#23274=EDGE_CURVE('',#18770,#18768,#8412,.T.);
#23275=EDGE_CURVE('',#18771,#18770,#8413,.T.);
#23276=EDGE_CURVE('',#18772,#18771,#8414,.T.);
#23277=EDGE_CURVE('',#18773,#18772,#8415,.T.);
#23278=EDGE_CURVE('',#18769,#18773,#8416,.T.);
#23279=EDGE_CURVE('',#18774,#18775,#8417,.T.);
#23280=EDGE_CURVE('',#18776,#18774,#8418,.T.);
#23281=EDGE_CURVE('',#18777,#18776,#8419,.T.);
#23282=EDGE_CURVE('',#18778,#18777,#8420,.T.);
#23283=EDGE_CURVE('',#18779,#18778,#8421,.T.);
#23284=EDGE_CURVE('',#18775,#18779,#8422,.T.);
#23285=EDGE_CURVE('',#18780,#18781,#8423,.T.);
#23286=EDGE_CURVE('',#18782,#18780,#8424,.T.);
#23287=EDGE_CURVE('',#18783,#18782,#8425,.T.);
#23288=EDGE_CURVE('',#18784,#18783,#8426,.T.);
#23289=EDGE_CURVE('',#18785,#18784,#8427,.T.);
#23290=EDGE_CURVE('',#18781,#18785,#8428,.T.);
#23291=EDGE_CURVE('',#18786,#18787,#8429,.T.);
#23292=EDGE_CURVE('',#18788,#18786,#8430,.T.);
#23293=EDGE_CURVE('',#18789,#18788,#8431,.T.);
#23294=EDGE_CURVE('',#18790,#18789,#8432,.T.);
#23295=EDGE_CURVE('',#18791,#18790,#8433,.T.);
#23296=EDGE_CURVE('',#18787,#18791,#8434,.T.);
#23297=EDGE_CURVE('',#18792,#18793,#8435,.T.);
#23298=EDGE_CURVE('',#18794,#18792,#8436,.T.);
#23299=EDGE_CURVE('',#18795,#18794,#8437,.T.);
#23300=EDGE_CURVE('',#18796,#18795,#8438,.T.);
#23301=EDGE_CURVE('',#18797,#18796,#8439,.T.);
#23302=EDGE_CURVE('',#18793,#18797,#8440,.T.);
#23303=EDGE_CURVE('',#18798,#18799,#8441,.T.);
#23304=EDGE_CURVE('',#18800,#18798,#8442,.T.);
#23305=EDGE_CURVE('',#18801,#18800,#8443,.T.);
#23306=EDGE_CURVE('',#18802,#18801,#8444,.T.);
#23307=EDGE_CURVE('',#18803,#18802,#8445,.T.);
#23308=EDGE_CURVE('',#18799,#18803,#8446,.T.);
#23309=EDGE_CURVE('',#18804,#18805,#8447,.T.);
#23310=EDGE_CURVE('',#18806,#18804,#8448,.T.);
#23311=EDGE_CURVE('',#18807,#18806,#8449,.T.);
#23312=EDGE_CURVE('',#18808,#18807,#8450,.T.);
#23313=EDGE_CURVE('',#18809,#18808,#8451,.T.);
#23314=EDGE_CURVE('',#18805,#18809,#8452,.T.);
#23315=EDGE_CURVE('',#18810,#18811,#8453,.T.);
#23316=EDGE_CURVE('',#18812,#18810,#8454,.T.);
#23317=EDGE_CURVE('',#18813,#18812,#8455,.T.);
#23318=EDGE_CURVE('',#18814,#18813,#8456,.T.);
#23319=EDGE_CURVE('',#18815,#18814,#8457,.T.);
#23320=EDGE_CURVE('',#18811,#18815,#8458,.T.);
#23321=EDGE_CURVE('',#18816,#18817,#8459,.T.);
#23322=EDGE_CURVE('',#18818,#18816,#8460,.T.);
#23323=EDGE_CURVE('',#18819,#18818,#8461,.T.);
#23324=EDGE_CURVE('',#18820,#18819,#8462,.T.);
#23325=EDGE_CURVE('',#18821,#18820,#8463,.T.);
#23326=EDGE_CURVE('',#18817,#18821,#8464,.T.);
#23327=EDGE_CURVE('',#18822,#18823,#8465,.T.);
#23328=EDGE_CURVE('',#18824,#18822,#8466,.T.);
#23329=EDGE_CURVE('',#18825,#18824,#8467,.T.);
#23330=EDGE_CURVE('',#18826,#18825,#8468,.T.);
#23331=EDGE_CURVE('',#18827,#18826,#8469,.T.);
#23332=EDGE_CURVE('',#18823,#18827,#8470,.T.);
#23333=EDGE_CURVE('',#18828,#18829,#8471,.T.);
#23334=EDGE_CURVE('',#18830,#18828,#8472,.T.);
#23335=EDGE_CURVE('',#18831,#18830,#8473,.T.);
#23336=EDGE_CURVE('',#18832,#18831,#8474,.T.);
#23337=EDGE_CURVE('',#18833,#18832,#8475,.T.);
#23338=EDGE_CURVE('',#18829,#18833,#8476,.T.);
#23339=EDGE_CURVE('',#18834,#18835,#8477,.T.);
#23340=EDGE_CURVE('',#18836,#18834,#8478,.T.);
#23341=EDGE_CURVE('',#18837,#18836,#8479,.T.);
#23342=EDGE_CURVE('',#18838,#18837,#8480,.T.);
#23343=EDGE_CURVE('',#18839,#18838,#8481,.T.);
#23344=EDGE_CURVE('',#18835,#18839,#8482,.T.);
#23345=EDGE_CURVE('',#18840,#18841,#8483,.T.);
#23346=EDGE_CURVE('',#18842,#18840,#8484,.T.);
#23347=EDGE_CURVE('',#18843,#18842,#8485,.T.);
#23348=EDGE_CURVE('',#18844,#18843,#8486,.T.);
#23349=EDGE_CURVE('',#18845,#18844,#8487,.T.);
#23350=EDGE_CURVE('',#18841,#18845,#8488,.T.);
#23351=EDGE_CURVE('',#18846,#18847,#8489,.T.);
#23352=EDGE_CURVE('',#18848,#18846,#8490,.T.);
#23353=EDGE_CURVE('',#18849,#18848,#8491,.T.);
#23354=EDGE_CURVE('',#18850,#18849,#8492,.T.);
#23355=EDGE_CURVE('',#18851,#18850,#8493,.T.);
#23356=EDGE_CURVE('',#18847,#18851,#8494,.T.);
#23357=EDGE_CURVE('',#18852,#18853,#8495,.T.);
#23358=EDGE_CURVE('',#18854,#18852,#8496,.T.);
#23359=EDGE_CURVE('',#18855,#18854,#8497,.T.);
#23360=EDGE_CURVE('',#18856,#18855,#8498,.T.);
#23361=EDGE_CURVE('',#18857,#18856,#8499,.T.);
#23362=EDGE_CURVE('',#18853,#18857,#8500,.T.);
#23363=EDGE_CURVE('',#18858,#18859,#8501,.T.);
#23364=EDGE_CURVE('',#18860,#18858,#8502,.T.);
#23365=EDGE_CURVE('',#18861,#18860,#8503,.T.);
#23366=EDGE_CURVE('',#18862,#18861,#8504,.T.);
#23367=EDGE_CURVE('',#18863,#18862,#8505,.T.);
#23368=EDGE_CURVE('',#18859,#18863,#8506,.T.);
#23369=EDGE_CURVE('',#18864,#18865,#8507,.T.);
#23370=EDGE_CURVE('',#18866,#18864,#8508,.T.);
#23371=EDGE_CURVE('',#18867,#18866,#8509,.T.);
#23372=EDGE_CURVE('',#18868,#18867,#8510,.T.);
#23373=EDGE_CURVE('',#18869,#18868,#8511,.T.);
#23374=EDGE_CURVE('',#18865,#18869,#8512,.T.);
#23375=EDGE_CURVE('',#18870,#18871,#8513,.T.);
#23376=EDGE_CURVE('',#18872,#18870,#8514,.T.);
#23377=EDGE_CURVE('',#18873,#18872,#8515,.T.);
#23378=EDGE_CURVE('',#18874,#18873,#8516,.T.);
#23379=EDGE_CURVE('',#18875,#18874,#8517,.T.);
#23380=EDGE_CURVE('',#18871,#18875,#8518,.T.);
#23381=EDGE_CURVE('',#18876,#18877,#8519,.T.);
#23382=EDGE_CURVE('',#18878,#18876,#8520,.T.);
#23383=EDGE_CURVE('',#18879,#18878,#8521,.T.);
#23384=EDGE_CURVE('',#18880,#18879,#8522,.T.);
#23385=EDGE_CURVE('',#18881,#18880,#8523,.T.);
#23386=EDGE_CURVE('',#18877,#18881,#8524,.T.);
#23387=EDGE_CURVE('',#18882,#18883,#8525,.T.);
#23388=EDGE_CURVE('',#18884,#18882,#8526,.T.);
#23389=EDGE_CURVE('',#18885,#18884,#8527,.T.);
#23390=EDGE_CURVE('',#18886,#18885,#8528,.T.);
#23391=EDGE_CURVE('',#18887,#18886,#8529,.T.);
#23392=EDGE_CURVE('',#18883,#18887,#8530,.T.);
#23393=EDGE_CURVE('',#18888,#18889,#8531,.T.);
#23394=EDGE_CURVE('',#18890,#18888,#8532,.T.);
#23395=EDGE_CURVE('',#18891,#18890,#8533,.T.);
#23396=EDGE_CURVE('',#18892,#18891,#8534,.T.);
#23397=EDGE_CURVE('',#18893,#18892,#8535,.T.);
#23398=EDGE_CURVE('',#18889,#18893,#8536,.T.);
#23399=EDGE_CURVE('',#18894,#18895,#8537,.T.);
#23400=EDGE_CURVE('',#18896,#18894,#8538,.T.);
#23401=EDGE_CURVE('',#18897,#18896,#8539,.T.);
#23402=EDGE_CURVE('',#18898,#18897,#8540,.T.);
#23403=EDGE_CURVE('',#18899,#18898,#8541,.T.);
#23404=EDGE_CURVE('',#18895,#18899,#8542,.T.);
#23405=EDGE_CURVE('',#18900,#18901,#8543,.T.);
#23406=EDGE_CURVE('',#18902,#18900,#8544,.T.);
#23407=EDGE_CURVE('',#18903,#18902,#8545,.T.);
#23408=EDGE_CURVE('',#18904,#18903,#8546,.T.);
#23409=EDGE_CURVE('',#18905,#18904,#8547,.T.);
#23410=EDGE_CURVE('',#18901,#18905,#8548,.T.);
#23411=EDGE_CURVE('',#18906,#18907,#8549,.T.);
#23412=EDGE_CURVE('',#18908,#18906,#8550,.T.);
#23413=EDGE_CURVE('',#18909,#18908,#8551,.T.);
#23414=EDGE_CURVE('',#18910,#18909,#8552,.T.);
#23415=EDGE_CURVE('',#18911,#18910,#8553,.T.);
#23416=EDGE_CURVE('',#18907,#18911,#8554,.T.);
#23417=EDGE_CURVE('',#18912,#18913,#8555,.T.);
#23418=EDGE_CURVE('',#18914,#18912,#8556,.T.);
#23419=EDGE_CURVE('',#18915,#18914,#8557,.T.);
#23420=EDGE_CURVE('',#18916,#18915,#8558,.T.);
#23421=EDGE_CURVE('',#18917,#18916,#8559,.T.);
#23422=EDGE_CURVE('',#18913,#18917,#8560,.T.);
#23423=EDGE_CURVE('',#18918,#18919,#8561,.T.);
#23424=EDGE_CURVE('',#18920,#18918,#8562,.T.);
#23425=EDGE_CURVE('',#18921,#18920,#8563,.T.);
#23426=EDGE_CURVE('',#18922,#18921,#8564,.T.);
#23427=EDGE_CURVE('',#18923,#18922,#8565,.T.);
#23428=EDGE_CURVE('',#18919,#18923,#8566,.T.);
#23429=EDGE_CURVE('',#18924,#18925,#8567,.T.);
#23430=EDGE_CURVE('',#18926,#18924,#8568,.T.);
#23431=EDGE_CURVE('',#18927,#18926,#8569,.T.);
#23432=EDGE_CURVE('',#18928,#18927,#8570,.T.);
#23433=EDGE_CURVE('',#18929,#18928,#8571,.T.);
#23434=EDGE_CURVE('',#18925,#18929,#8572,.T.);
#23435=EDGE_CURVE('',#18930,#18931,#8573,.T.);
#23436=EDGE_CURVE('',#18932,#18930,#8574,.T.);
#23437=EDGE_CURVE('',#18933,#18932,#8575,.T.);
#23438=EDGE_CURVE('',#18934,#18933,#8576,.T.);
#23439=EDGE_CURVE('',#18935,#18934,#8577,.T.);
#23440=EDGE_CURVE('',#18931,#18935,#8578,.T.);
#23441=EDGE_CURVE('',#18936,#18937,#8579,.T.);
#23442=EDGE_CURVE('',#18938,#18936,#8580,.T.);
#23443=EDGE_CURVE('',#18939,#18938,#8581,.T.);
#23444=EDGE_CURVE('',#18940,#18939,#8582,.T.);
#23445=EDGE_CURVE('',#18941,#18940,#8583,.T.);
#23446=EDGE_CURVE('',#18937,#18941,#8584,.T.);
#23447=EDGE_CURVE('',#18942,#18943,#8585,.T.);
#23448=EDGE_CURVE('',#18944,#18942,#8586,.T.);
#23449=EDGE_CURVE('',#18945,#18944,#8587,.T.);
#23450=EDGE_CURVE('',#18946,#18945,#8588,.T.);
#23451=EDGE_CURVE('',#18947,#18946,#8589,.T.);
#23452=EDGE_CURVE('',#18943,#18947,#8590,.T.);
#23453=EDGE_CURVE('',#18948,#18949,#8591,.T.);
#23454=EDGE_CURVE('',#18950,#18948,#8592,.T.);
#23455=EDGE_CURVE('',#18951,#18950,#8593,.T.);
#23456=EDGE_CURVE('',#18952,#18951,#8594,.T.);
#23457=EDGE_CURVE('',#18953,#18952,#8595,.T.);
#23458=EDGE_CURVE('',#18949,#18953,#8596,.T.);
#23459=EDGE_CURVE('',#18954,#18955,#8597,.T.);
#23460=EDGE_CURVE('',#18956,#18954,#8598,.T.);
#23461=EDGE_CURVE('',#18957,#18956,#8599,.T.);
#23462=EDGE_CURVE('',#18958,#18957,#8600,.T.);
#23463=EDGE_CURVE('',#18959,#18958,#8601,.T.);
#23464=EDGE_CURVE('',#18955,#18959,#8602,.T.);
#23465=EDGE_CURVE('',#18960,#18961,#8603,.T.);
#23466=EDGE_CURVE('',#18962,#18960,#8604,.T.);
#23467=EDGE_CURVE('',#18963,#18962,#8605,.T.);
#23468=EDGE_CURVE('',#18964,#18963,#8606,.T.);
#23469=EDGE_CURVE('',#18965,#18964,#8607,.T.);
#23470=EDGE_CURVE('',#18961,#18965,#8608,.T.);
#23471=EDGE_CURVE('',#18966,#18967,#8609,.T.);
#23472=EDGE_CURVE('',#18968,#18966,#8610,.T.);
#23473=EDGE_CURVE('',#18969,#18968,#8611,.T.);
#23474=EDGE_CURVE('',#18970,#18969,#8612,.T.);
#23475=EDGE_CURVE('',#18971,#18970,#8613,.T.);
#23476=EDGE_CURVE('',#18967,#18971,#8614,.T.);
#23477=EDGE_CURVE('',#18972,#18973,#8615,.T.);
#23478=EDGE_CURVE('',#18974,#18972,#8616,.T.);
#23479=EDGE_CURVE('',#18975,#18974,#8617,.T.);
#23480=EDGE_CURVE('',#18976,#18975,#8618,.T.);
#23481=EDGE_CURVE('',#18977,#18976,#8619,.T.);
#23482=EDGE_CURVE('',#18973,#18977,#8620,.T.);
#23483=EDGE_CURVE('',#18978,#18979,#8621,.T.);
#23484=EDGE_CURVE('',#18980,#18978,#8622,.T.);
#23485=EDGE_CURVE('',#18981,#18980,#8623,.T.);
#23486=EDGE_CURVE('',#18982,#18981,#8624,.T.);
#23487=EDGE_CURVE('',#18983,#18982,#8625,.T.);
#23488=EDGE_CURVE('',#18979,#18983,#8626,.T.);
#23489=EDGE_CURVE('',#18984,#18985,#8627,.T.);
#23490=EDGE_CURVE('',#18986,#18984,#8628,.T.);
#23491=EDGE_CURVE('',#18987,#18986,#8629,.T.);
#23492=EDGE_CURVE('',#18988,#18987,#8630,.T.);
#23493=EDGE_CURVE('',#18989,#18988,#8631,.T.);
#23494=EDGE_CURVE('',#18985,#18989,#8632,.T.);
#23495=EDGE_CURVE('',#18990,#18991,#8633,.T.);
#23496=EDGE_CURVE('',#18992,#18990,#8634,.T.);
#23497=EDGE_CURVE('',#18993,#18992,#8635,.T.);
#23498=EDGE_CURVE('',#18994,#18993,#8636,.T.);
#23499=EDGE_CURVE('',#18995,#18994,#8637,.T.);
#23500=EDGE_CURVE('',#18991,#18995,#8638,.T.);
#23501=EDGE_CURVE('',#18996,#18997,#8639,.T.);
#23502=EDGE_CURVE('',#18998,#18996,#8640,.T.);
#23503=EDGE_CURVE('',#18999,#18998,#8641,.T.);
#23504=EDGE_CURVE('',#19000,#18999,#8642,.T.);
#23505=EDGE_CURVE('',#19001,#19000,#8643,.T.);
#23506=EDGE_CURVE('',#18997,#19001,#8644,.T.);
#23507=EDGE_CURVE('',#19002,#19003,#8645,.T.);
#23508=EDGE_CURVE('',#19004,#19002,#8646,.T.);
#23509=EDGE_CURVE('',#19005,#19004,#8647,.T.);
#23510=EDGE_CURVE('',#19006,#19005,#8648,.T.);
#23511=EDGE_CURVE('',#19007,#19006,#8649,.T.);
#23512=EDGE_CURVE('',#19003,#19007,#8650,.T.);
#23513=EDGE_CURVE('',#19008,#19009,#8651,.T.);
#23514=EDGE_CURVE('',#19010,#19008,#8652,.T.);
#23515=EDGE_CURVE('',#19011,#19010,#8653,.T.);
#23516=EDGE_CURVE('',#19012,#19011,#8654,.T.);
#23517=EDGE_CURVE('',#19013,#19012,#8655,.T.);
#23518=EDGE_CURVE('',#19009,#19013,#8656,.T.);
#23519=EDGE_CURVE('',#19014,#19015,#8657,.T.);
#23520=EDGE_CURVE('',#19016,#19014,#8658,.T.);
#23521=EDGE_CURVE('',#19017,#19016,#8659,.T.);
#23522=EDGE_CURVE('',#19018,#19017,#8660,.T.);
#23523=EDGE_CURVE('',#19019,#19018,#8661,.T.);
#23524=EDGE_CURVE('',#19015,#19019,#8662,.T.);
#23525=EDGE_CURVE('',#19020,#19021,#8663,.T.);
#23526=EDGE_CURVE('',#19022,#19020,#8664,.T.);
#23527=EDGE_CURVE('',#19023,#19022,#8665,.T.);
#23528=EDGE_CURVE('',#19024,#19023,#8666,.T.);
#23529=EDGE_CURVE('',#19025,#19024,#8667,.T.);
#23530=EDGE_CURVE('',#19021,#19025,#8668,.T.);
#23531=EDGE_CURVE('',#19026,#19027,#8669,.T.);
#23532=EDGE_CURVE('',#19028,#19026,#8670,.T.);
#23533=EDGE_CURVE('',#19029,#19028,#8671,.T.);
#23534=EDGE_CURVE('',#19030,#19029,#8672,.T.);
#23535=EDGE_CURVE('',#19031,#19030,#8673,.T.);
#23536=EDGE_CURVE('',#19027,#19031,#8674,.T.);
#23537=EDGE_CURVE('',#19032,#19033,#8675,.T.);
#23538=EDGE_CURVE('',#19034,#19032,#8676,.T.);
#23539=EDGE_CURVE('',#19035,#19034,#8677,.T.);
#23540=EDGE_CURVE('',#19036,#19035,#8678,.T.);
#23541=EDGE_CURVE('',#19037,#19036,#8679,.T.);
#23542=EDGE_CURVE('',#19033,#19037,#8680,.T.);
#23543=EDGE_CURVE('',#19038,#19039,#8681,.T.);
#23544=EDGE_CURVE('',#19040,#19038,#8682,.T.);
#23545=EDGE_CURVE('',#19041,#19040,#8683,.T.);
#23546=EDGE_CURVE('',#19042,#19041,#8684,.T.);
#23547=EDGE_CURVE('',#19043,#19042,#8685,.T.);
#23548=EDGE_CURVE('',#19039,#19043,#8686,.T.);
#23549=EDGE_CURVE('',#19044,#19045,#8687,.T.);
#23550=EDGE_CURVE('',#19046,#19044,#8688,.T.);
#23551=EDGE_CURVE('',#19047,#19046,#8689,.T.);
#23552=EDGE_CURVE('',#19048,#19047,#8690,.T.);
#23553=EDGE_CURVE('',#19049,#19048,#8691,.T.);
#23554=EDGE_CURVE('',#19045,#19049,#8692,.T.);
#23555=EDGE_CURVE('',#19050,#19051,#8693,.T.);
#23556=EDGE_CURVE('',#19052,#19050,#8694,.T.);
#23557=EDGE_CURVE('',#19053,#19052,#8695,.T.);
#23558=EDGE_CURVE('',#19054,#19053,#8696,.T.);
#23559=EDGE_CURVE('',#19055,#19054,#8697,.T.);
#23560=EDGE_CURVE('',#19051,#19055,#8698,.T.);
#23561=EDGE_CURVE('',#19056,#19057,#8699,.T.);
#23562=EDGE_CURVE('',#19058,#19056,#8700,.T.);
#23563=EDGE_CURVE('',#19059,#19058,#8701,.T.);
#23564=EDGE_CURVE('',#19060,#19059,#8702,.T.);
#23565=EDGE_CURVE('',#19061,#19060,#8703,.T.);
#23566=EDGE_CURVE('',#19057,#19061,#8704,.T.);
#23567=EDGE_CURVE('',#19062,#19063,#8705,.T.);
#23568=EDGE_CURVE('',#19064,#19062,#8706,.T.);
#23569=EDGE_CURVE('',#19065,#19064,#8707,.T.);
#23570=EDGE_CURVE('',#19066,#19065,#8708,.T.);
#23571=EDGE_CURVE('',#19067,#19066,#8709,.T.);
#23572=EDGE_CURVE('',#19063,#19067,#8710,.T.);
#23573=EDGE_CURVE('',#19068,#19069,#8711,.T.);
#23574=EDGE_CURVE('',#19070,#19068,#8712,.T.);
#23575=EDGE_CURVE('',#19071,#19070,#8713,.T.);
#23576=EDGE_CURVE('',#19072,#19071,#8714,.T.);
#23577=EDGE_CURVE('',#19073,#19072,#8715,.T.);
#23578=EDGE_CURVE('',#19069,#19073,#8716,.T.);
#23579=EDGE_CURVE('',#19074,#19075,#8717,.T.);
#23580=EDGE_CURVE('',#19076,#19074,#8718,.T.);
#23581=EDGE_CURVE('',#19077,#19076,#8719,.T.);
#23582=EDGE_CURVE('',#19078,#19077,#8720,.T.);
#23583=EDGE_CURVE('',#19079,#19078,#8721,.T.);
#23584=EDGE_CURVE('',#19075,#19079,#8722,.T.);
#23585=EDGE_CURVE('',#19080,#19081,#8723,.T.);
#23586=EDGE_CURVE('',#19082,#19080,#8724,.T.);
#23587=EDGE_CURVE('',#19083,#19082,#8725,.T.);
#23588=EDGE_CURVE('',#19084,#19083,#8726,.T.);
#23589=EDGE_CURVE('',#19085,#19084,#8727,.T.);
#23590=EDGE_CURVE('',#19081,#19085,#8728,.T.);
#23591=EDGE_CURVE('',#19086,#19087,#8729,.T.);
#23592=EDGE_CURVE('',#19088,#19086,#8730,.T.);
#23593=EDGE_CURVE('',#19089,#19088,#8731,.T.);
#23594=EDGE_CURVE('',#19090,#19089,#8732,.T.);
#23595=EDGE_CURVE('',#19091,#19090,#8733,.T.);
#23596=EDGE_CURVE('',#19087,#19091,#8734,.T.);
#23597=EDGE_CURVE('',#19092,#19093,#8735,.T.);
#23598=EDGE_CURVE('',#19094,#19092,#8736,.T.);
#23599=EDGE_CURVE('',#19095,#19094,#8737,.T.);
#23600=EDGE_CURVE('',#19096,#19095,#8738,.T.);
#23601=EDGE_CURVE('',#19097,#19096,#8739,.T.);
#23602=EDGE_CURVE('',#19093,#19097,#8740,.T.);
#23603=EDGE_CURVE('',#19098,#19099,#8741,.T.);
#23604=EDGE_CURVE('',#19100,#19098,#8742,.T.);
#23605=EDGE_CURVE('',#19101,#19100,#8743,.T.);
#23606=EDGE_CURVE('',#19102,#19101,#8744,.T.);
#23607=EDGE_CURVE('',#19103,#19102,#8745,.T.);
#23608=EDGE_CURVE('',#19099,#19103,#8746,.T.);
#23609=EDGE_CURVE('',#19104,#19105,#8747,.T.);
#23610=EDGE_CURVE('',#19106,#19104,#8748,.T.);
#23611=EDGE_CURVE('',#19107,#19106,#8749,.T.);
#23612=EDGE_CURVE('',#19108,#19107,#8750,.T.);
#23613=EDGE_CURVE('',#19109,#19108,#8751,.T.);
#23614=EDGE_CURVE('',#19105,#19109,#8752,.T.);
#23615=EDGE_CURVE('',#19110,#19111,#8753,.T.);
#23616=EDGE_CURVE('',#19112,#19110,#8754,.T.);
#23617=EDGE_CURVE('',#19113,#19112,#8755,.T.);
#23618=EDGE_CURVE('',#19114,#19113,#8756,.T.);
#23619=EDGE_CURVE('',#19115,#19114,#8757,.T.);
#23620=EDGE_CURVE('',#19111,#19115,#8758,.T.);
#23621=EDGE_CURVE('',#19116,#19117,#8759,.T.);
#23622=EDGE_CURVE('',#19118,#19116,#8760,.T.);
#23623=EDGE_CURVE('',#19119,#19118,#8761,.T.);
#23624=EDGE_CURVE('',#19120,#19119,#8762,.T.);
#23625=EDGE_CURVE('',#19121,#19120,#8763,.T.);
#23626=EDGE_CURVE('',#19117,#19121,#8764,.T.);
#23627=EDGE_CURVE('',#19122,#19123,#8765,.T.);
#23628=EDGE_CURVE('',#19124,#19122,#8766,.T.);
#23629=EDGE_CURVE('',#19125,#19124,#8767,.T.);
#23630=EDGE_CURVE('',#19126,#19125,#8768,.T.);
#23631=EDGE_CURVE('',#19127,#19126,#8769,.T.);
#23632=EDGE_CURVE('',#19123,#19127,#8770,.T.);
#23633=EDGE_CURVE('',#19128,#19129,#8771,.T.);
#23634=EDGE_CURVE('',#19130,#19128,#8772,.T.);
#23635=EDGE_CURVE('',#19131,#19130,#8773,.T.);
#23636=EDGE_CURVE('',#19132,#19131,#8774,.T.);
#23637=EDGE_CURVE('',#19133,#19132,#8775,.T.);
#23638=EDGE_CURVE('',#19129,#19133,#8776,.T.);
#23639=EDGE_CURVE('',#19134,#19135,#8777,.T.);
#23640=EDGE_CURVE('',#19136,#19134,#8778,.T.);
#23641=EDGE_CURVE('',#19137,#19136,#8779,.T.);
#23642=EDGE_CURVE('',#19138,#19137,#8780,.T.);
#23643=EDGE_CURVE('',#19139,#19138,#8781,.T.);
#23644=EDGE_CURVE('',#19135,#19139,#8782,.T.);
#23645=EDGE_CURVE('',#19140,#19141,#8783,.T.);
#23646=EDGE_CURVE('',#19142,#19140,#8784,.T.);
#23647=EDGE_CURVE('',#19143,#19142,#8785,.T.);
#23648=EDGE_CURVE('',#19144,#19143,#8786,.T.);
#23649=EDGE_CURVE('',#19145,#19144,#8787,.T.);
#23650=EDGE_CURVE('',#19141,#19145,#8788,.T.);
#23651=EDGE_CURVE('',#19146,#19147,#8789,.T.);
#23652=EDGE_CURVE('',#19148,#19146,#8790,.T.);
#23653=EDGE_CURVE('',#19149,#19148,#8791,.T.);
#23654=EDGE_CURVE('',#19150,#19149,#8792,.T.);
#23655=EDGE_CURVE('',#19151,#19150,#8793,.T.);
#23656=EDGE_CURVE('',#19147,#19151,#8794,.T.);
#23657=EDGE_CURVE('',#19152,#19153,#8795,.T.);
#23658=EDGE_CURVE('',#19154,#19152,#8796,.T.);
#23659=EDGE_CURVE('',#19155,#19154,#8797,.T.);
#23660=EDGE_CURVE('',#19156,#19155,#8798,.T.);
#23661=EDGE_CURVE('',#19157,#19156,#8799,.T.);
#23662=EDGE_CURVE('',#19153,#19157,#8800,.T.);
#23663=EDGE_CURVE('',#19158,#19159,#8801,.T.);
#23664=EDGE_CURVE('',#19160,#19158,#8802,.T.);
#23665=EDGE_CURVE('',#19161,#19160,#8803,.T.);
#23666=EDGE_CURVE('',#19162,#19161,#8804,.T.);
#23667=EDGE_CURVE('',#19163,#19162,#8805,.T.);
#23668=EDGE_CURVE('',#19159,#19163,#8806,.T.);
#23669=EDGE_CURVE('',#19164,#19165,#8807,.T.);
#23670=EDGE_CURVE('',#19166,#19164,#8808,.T.);
#23671=EDGE_CURVE('',#19167,#19166,#8809,.T.);
#23672=EDGE_CURVE('',#19168,#19167,#8810,.T.);
#23673=EDGE_CURVE('',#19169,#19168,#8811,.T.);
#23674=EDGE_CURVE('',#19165,#19169,#8812,.T.);
#23675=EDGE_CURVE('',#19170,#19171,#8813,.T.);
#23676=EDGE_CURVE('',#19172,#19170,#8814,.T.);
#23677=EDGE_CURVE('',#19173,#19172,#8815,.T.);
#23678=EDGE_CURVE('',#19174,#19173,#8816,.T.);
#23679=EDGE_CURVE('',#19175,#19174,#8817,.T.);
#23680=EDGE_CURVE('',#19171,#19175,#8818,.T.);
#23681=EDGE_CURVE('',#19176,#19177,#8819,.T.);
#23682=EDGE_CURVE('',#19178,#19176,#8820,.T.);
#23683=EDGE_CURVE('',#19179,#19178,#8821,.T.);
#23684=EDGE_CURVE('',#19180,#19179,#8822,.T.);
#23685=EDGE_CURVE('',#19181,#19180,#8823,.T.);
#23686=EDGE_CURVE('',#19177,#19181,#8824,.T.);
#23687=EDGE_CURVE('',#19182,#19183,#8825,.T.);
#23688=EDGE_CURVE('',#19184,#19182,#8826,.T.);
#23689=EDGE_CURVE('',#19185,#19184,#8827,.T.);
#23690=EDGE_CURVE('',#19186,#19185,#8828,.T.);
#23691=EDGE_CURVE('',#19187,#19186,#8829,.T.);
#23692=EDGE_CURVE('',#19183,#19187,#8830,.T.);
#23693=EDGE_CURVE('',#19188,#19189,#8831,.T.);
#23694=EDGE_CURVE('',#19190,#19188,#8832,.T.);
#23695=EDGE_CURVE('',#19191,#19190,#8833,.T.);
#23696=EDGE_CURVE('',#19192,#19191,#8834,.T.);
#23697=EDGE_CURVE('',#19193,#19192,#8835,.T.);
#23698=EDGE_CURVE('',#19189,#19193,#8836,.T.);
#23699=EDGE_CURVE('',#19194,#19195,#8837,.T.);
#23700=EDGE_CURVE('',#19196,#19194,#8838,.T.);
#23701=EDGE_CURVE('',#19197,#19196,#8839,.T.);
#23702=EDGE_CURVE('',#19198,#19197,#8840,.T.);
#23703=EDGE_CURVE('',#19199,#19198,#8841,.T.);
#23704=EDGE_CURVE('',#19195,#19199,#8842,.T.);
#23705=EDGE_CURVE('',#19200,#19201,#8843,.T.);
#23706=EDGE_CURVE('',#19202,#19200,#8844,.T.);
#23707=EDGE_CURVE('',#19203,#19202,#8845,.T.);
#23708=EDGE_CURVE('',#19204,#19203,#8846,.T.);
#23709=EDGE_CURVE('',#19205,#19204,#8847,.T.);
#23710=EDGE_CURVE('',#19201,#19205,#8848,.T.);
#23711=EDGE_CURVE('',#19206,#19207,#8849,.T.);
#23712=EDGE_CURVE('',#19208,#19206,#8850,.T.);
#23713=EDGE_CURVE('',#19209,#19208,#8851,.T.);
#23714=EDGE_CURVE('',#19210,#19209,#8852,.T.);
#23715=EDGE_CURVE('',#19211,#19210,#8853,.T.);
#23716=EDGE_CURVE('',#19207,#19211,#8854,.T.);
#23717=EDGE_CURVE('',#19212,#19213,#8855,.T.);
#23718=EDGE_CURVE('',#19214,#19212,#8856,.T.);
#23719=EDGE_CURVE('',#19215,#19214,#8857,.T.);
#23720=EDGE_CURVE('',#19216,#19215,#8858,.T.);
#23721=EDGE_CURVE('',#19217,#19216,#8859,.T.);
#23722=EDGE_CURVE('',#19213,#19217,#8860,.T.);
#23723=EDGE_CURVE('',#19218,#19219,#8861,.T.);
#23724=EDGE_CURVE('',#19220,#19218,#8862,.T.);
#23725=EDGE_CURVE('',#19221,#19220,#8863,.T.);
#23726=EDGE_CURVE('',#19222,#19221,#8864,.T.);
#23727=EDGE_CURVE('',#19223,#19222,#8865,.T.);
#23728=EDGE_CURVE('',#19219,#19223,#8866,.T.);
#23729=EDGE_CURVE('',#19224,#19225,#8867,.T.);
#23730=EDGE_CURVE('',#19226,#19224,#8868,.T.);
#23731=EDGE_CURVE('',#19227,#19226,#8869,.T.);
#23732=EDGE_CURVE('',#19228,#19227,#8870,.T.);
#23733=EDGE_CURVE('',#19229,#19228,#8871,.T.);
#23734=EDGE_CURVE('',#19225,#19229,#8872,.T.);
#23735=EDGE_CURVE('',#19230,#19231,#8873,.T.);
#23736=EDGE_CURVE('',#19232,#19230,#8874,.T.);
#23737=EDGE_CURVE('',#19233,#19232,#8875,.T.);
#23738=EDGE_CURVE('',#19234,#19233,#8876,.T.);
#23739=EDGE_CURVE('',#19235,#19234,#8877,.T.);
#23740=EDGE_CURVE('',#19231,#19235,#8878,.T.);
#23741=EDGE_CURVE('',#19236,#19237,#8879,.T.);
#23742=EDGE_CURVE('',#19238,#19236,#8880,.T.);
#23743=EDGE_CURVE('',#19239,#19238,#8881,.T.);
#23744=EDGE_CURVE('',#19240,#19239,#8882,.T.);
#23745=EDGE_CURVE('',#19241,#19240,#8883,.T.);
#23746=EDGE_CURVE('',#19237,#19241,#8884,.T.);
#23747=EDGE_CURVE('',#19242,#19243,#8885,.T.);
#23748=EDGE_CURVE('',#19244,#19242,#8886,.T.);
#23749=EDGE_CURVE('',#19245,#19244,#8887,.T.);
#23750=EDGE_CURVE('',#19246,#19245,#8888,.T.);
#23751=EDGE_CURVE('',#19247,#19246,#8889,.T.);
#23752=EDGE_CURVE('',#19243,#19247,#8890,.T.);
#23753=EDGE_CURVE('',#19248,#19249,#8891,.T.);
#23754=EDGE_CURVE('',#19250,#19248,#8892,.T.);
#23755=EDGE_CURVE('',#19251,#19250,#8893,.T.);
#23756=EDGE_CURVE('',#19252,#19251,#8894,.T.);
#23757=EDGE_CURVE('',#19253,#19252,#8895,.T.);
#23758=EDGE_CURVE('',#19249,#19253,#8896,.T.);
#23759=EDGE_CURVE('',#19254,#19255,#8897,.T.);
#23760=EDGE_CURVE('',#19256,#19254,#8898,.T.);
#23761=EDGE_CURVE('',#19257,#19256,#8899,.T.);
#23762=EDGE_CURVE('',#19258,#19257,#8900,.T.);
#23763=EDGE_CURVE('',#19259,#19258,#8901,.T.);
#23764=EDGE_CURVE('',#19255,#19259,#8902,.T.);
#23765=EDGE_CURVE('',#19260,#19261,#8903,.T.);
#23766=EDGE_CURVE('',#19262,#19260,#8904,.T.);
#23767=EDGE_CURVE('',#19263,#19262,#8905,.T.);
#23768=EDGE_CURVE('',#19264,#19263,#8906,.T.);
#23769=EDGE_CURVE('',#19265,#19264,#8907,.T.);
#23770=EDGE_CURVE('',#19261,#19265,#8908,.T.);
#23771=EDGE_CURVE('',#19266,#19267,#8909,.T.);
#23772=EDGE_CURVE('',#19268,#19266,#8910,.T.);
#23773=EDGE_CURVE('',#19269,#19268,#8911,.T.);
#23774=EDGE_CURVE('',#19270,#19269,#8912,.T.);
#23775=EDGE_CURVE('',#19271,#19270,#8913,.T.);
#23776=EDGE_CURVE('',#19267,#19271,#8914,.T.);
#23777=EDGE_CURVE('',#19272,#19273,#8915,.T.);
#23778=EDGE_CURVE('',#19274,#19272,#8916,.T.);
#23779=EDGE_CURVE('',#19275,#19274,#8917,.T.);
#23780=EDGE_CURVE('',#19276,#19275,#8918,.T.);
#23781=EDGE_CURVE('',#19277,#19276,#8919,.T.);
#23782=EDGE_CURVE('',#19273,#19277,#8920,.T.);
#23783=EDGE_CURVE('',#19278,#19279,#8921,.T.);
#23784=EDGE_CURVE('',#19280,#19278,#8922,.T.);
#23785=EDGE_CURVE('',#19281,#19280,#8923,.T.);
#23786=EDGE_CURVE('',#19282,#19281,#8924,.T.);
#23787=EDGE_CURVE('',#19283,#19282,#8925,.T.);
#23788=EDGE_CURVE('',#19279,#19283,#8926,.T.);
#23789=EDGE_CURVE('',#19284,#19285,#8927,.T.);
#23790=EDGE_CURVE('',#19286,#19284,#8928,.T.);
#23791=EDGE_CURVE('',#19287,#19286,#8929,.T.);
#23792=EDGE_CURVE('',#19288,#19287,#8930,.T.);
#23793=EDGE_CURVE('',#19289,#19288,#8931,.T.);
#23794=EDGE_CURVE('',#19285,#19289,#8932,.T.);
#23795=EDGE_CURVE('',#19290,#19291,#8933,.T.);
#23796=EDGE_CURVE('',#19292,#19290,#8934,.T.);
#23797=EDGE_CURVE('',#19293,#19292,#8935,.T.);
#23798=EDGE_CURVE('',#19294,#19293,#8936,.T.);
#23799=EDGE_CURVE('',#19295,#19294,#8937,.T.);
#23800=EDGE_CURVE('',#19291,#19295,#8938,.T.);
#23801=EDGE_CURVE('',#19296,#19297,#8939,.T.);
#23802=EDGE_CURVE('',#19298,#19296,#8940,.T.);
#23803=EDGE_CURVE('',#19299,#19298,#8941,.T.);
#23804=EDGE_CURVE('',#19300,#19299,#8942,.T.);
#23805=EDGE_CURVE('',#19301,#19300,#8943,.T.);
#23806=EDGE_CURVE('',#19297,#19301,#8944,.T.);
#23807=EDGE_CURVE('',#19302,#19303,#8945,.T.);
#23808=EDGE_CURVE('',#19304,#19302,#8946,.T.);
#23809=EDGE_CURVE('',#19305,#19304,#8947,.T.);
#23810=EDGE_CURVE('',#19306,#19305,#8948,.T.);
#23811=EDGE_CURVE('',#19307,#19306,#8949,.T.);
#23812=EDGE_CURVE('',#19303,#19307,#8950,.T.);
#23813=EDGE_CURVE('',#19308,#19309,#8951,.T.);
#23814=EDGE_CURVE('',#19310,#19308,#8952,.T.);
#23815=EDGE_CURVE('',#19311,#19310,#8953,.T.);
#23816=EDGE_CURVE('',#19312,#19311,#8954,.T.);
#23817=EDGE_CURVE('',#19313,#19312,#8955,.T.);
#23818=EDGE_CURVE('',#19309,#19313,#8956,.T.);
#23819=EDGE_CURVE('',#19314,#19315,#8957,.T.);
#23820=EDGE_CURVE('',#19316,#19314,#8958,.T.);
#23821=EDGE_CURVE('',#19317,#19316,#8959,.T.);
#23822=EDGE_CURVE('',#19318,#19317,#8960,.T.);
#23823=EDGE_CURVE('',#19319,#19318,#8961,.T.);
#23824=EDGE_CURVE('',#19315,#19319,#8962,.T.);
#23825=EDGE_CURVE('',#19320,#19321,#8963,.T.);
#23826=EDGE_CURVE('',#19322,#19320,#8964,.T.);
#23827=EDGE_CURVE('',#19323,#19322,#8965,.T.);
#23828=EDGE_CURVE('',#19324,#19323,#8966,.T.);
#23829=EDGE_CURVE('',#19325,#19324,#8967,.T.);
#23830=EDGE_CURVE('',#19321,#19325,#8968,.T.);
#23831=EDGE_CURVE('',#19326,#19327,#8969,.T.);
#23832=EDGE_CURVE('',#19328,#19326,#8970,.T.);
#23833=EDGE_CURVE('',#19329,#19328,#8971,.T.);
#23834=EDGE_CURVE('',#19330,#19329,#8972,.T.);
#23835=EDGE_CURVE('',#19331,#19330,#8973,.T.);
#23836=EDGE_CURVE('',#19327,#19331,#8974,.T.);
#23837=EDGE_CURVE('',#19332,#19333,#8975,.T.);
#23838=EDGE_CURVE('',#19334,#19332,#8976,.T.);
#23839=EDGE_CURVE('',#19335,#19334,#8977,.T.);
#23840=EDGE_CURVE('',#19336,#19335,#8978,.T.);
#23841=EDGE_CURVE('',#19337,#19336,#8979,.T.);
#23842=EDGE_CURVE('',#19333,#19337,#8980,.T.);
#23843=EDGE_CURVE('',#19338,#19339,#8981,.T.);
#23844=EDGE_CURVE('',#19340,#19338,#8982,.T.);
#23845=EDGE_CURVE('',#19341,#19340,#8983,.T.);
#23846=EDGE_CURVE('',#19342,#19341,#8984,.T.);
#23847=EDGE_CURVE('',#19343,#19342,#8985,.T.);
#23848=EDGE_CURVE('',#19339,#19343,#8986,.T.);
#23849=EDGE_CURVE('',#19344,#19345,#8987,.T.);
#23850=EDGE_CURVE('',#19346,#19344,#8988,.T.);
#23851=EDGE_CURVE('',#19347,#19346,#8989,.T.);
#23852=EDGE_CURVE('',#19348,#19347,#8990,.T.);
#23853=EDGE_CURVE('',#19349,#19348,#8991,.T.);
#23854=EDGE_CURVE('',#19345,#19349,#8992,.T.);
#23855=EDGE_CURVE('',#19350,#19351,#8993,.T.);
#23856=EDGE_CURVE('',#19352,#19350,#8994,.T.);
#23857=EDGE_CURVE('',#19353,#19352,#8995,.T.);
#23858=EDGE_CURVE('',#19354,#19353,#8996,.T.);
#23859=EDGE_CURVE('',#19355,#19354,#8997,.T.);
#23860=EDGE_CURVE('',#19351,#19355,#8998,.T.);
#23861=EDGE_CURVE('',#19356,#19357,#8999,.T.);
#23862=EDGE_CURVE('',#19358,#19356,#9000,.T.);
#23863=EDGE_CURVE('',#19359,#19358,#9001,.T.);
#23864=EDGE_CURVE('',#19360,#19359,#9002,.T.);
#23865=EDGE_CURVE('',#19361,#19360,#9003,.T.);
#23866=EDGE_CURVE('',#19357,#19361,#9004,.T.);
#23867=EDGE_CURVE('',#19362,#19363,#9005,.T.);
#23868=EDGE_CURVE('',#19364,#19362,#9006,.T.);
#23869=EDGE_CURVE('',#19365,#19364,#9007,.T.);
#23870=EDGE_CURVE('',#19366,#19365,#9008,.T.);
#23871=EDGE_CURVE('',#19367,#19366,#9009,.T.);
#23872=EDGE_CURVE('',#19363,#19367,#9010,.T.);
#23873=EDGE_CURVE('',#19368,#19369,#9011,.T.);
#23874=EDGE_CURVE('',#19370,#19368,#9012,.T.);
#23875=EDGE_CURVE('',#19371,#19370,#9013,.T.);
#23876=EDGE_CURVE('',#19372,#19371,#9014,.T.);
#23877=EDGE_CURVE('',#19373,#19372,#9015,.T.);
#23878=EDGE_CURVE('',#19369,#19373,#9016,.T.);
#23879=EDGE_CURVE('',#19374,#19375,#9017,.T.);
#23880=EDGE_CURVE('',#19376,#19374,#9018,.T.);
#23881=EDGE_CURVE('',#19377,#19376,#9019,.T.);
#23882=EDGE_CURVE('',#19378,#19377,#9020,.T.);
#23883=EDGE_CURVE('',#19379,#19378,#9021,.T.);
#23884=EDGE_CURVE('',#19375,#19379,#9022,.T.);
#23885=EDGE_CURVE('',#19380,#19381,#9023,.T.);
#23886=EDGE_CURVE('',#19382,#19380,#9024,.T.);
#23887=EDGE_CURVE('',#19383,#19382,#9025,.T.);
#23888=EDGE_CURVE('',#19384,#19383,#9026,.T.);
#23889=EDGE_CURVE('',#19385,#19384,#9027,.T.);
#23890=EDGE_CURVE('',#19381,#19385,#9028,.T.);
#23891=EDGE_CURVE('',#19386,#19387,#9029,.T.);
#23892=EDGE_CURVE('',#19388,#19386,#9030,.T.);
#23893=EDGE_CURVE('',#19389,#19388,#9031,.T.);
#23894=EDGE_CURVE('',#19390,#19389,#9032,.T.);
#23895=EDGE_CURVE('',#19391,#19390,#9033,.T.);
#23896=EDGE_CURVE('',#19387,#19391,#9034,.T.);
#23897=EDGE_CURVE('',#19392,#19393,#9035,.T.);
#23898=EDGE_CURVE('',#19394,#19392,#9036,.T.);
#23899=EDGE_CURVE('',#19395,#19394,#9037,.T.);
#23900=EDGE_CURVE('',#19396,#19395,#9038,.T.);
#23901=EDGE_CURVE('',#19397,#19396,#9039,.T.);
#23902=EDGE_CURVE('',#19393,#19397,#9040,.T.);
#23903=EDGE_CURVE('',#19398,#19399,#9041,.T.);
#23904=EDGE_CURVE('',#19400,#19398,#9042,.T.);
#23905=EDGE_CURVE('',#19401,#19400,#9043,.T.);
#23906=EDGE_CURVE('',#19402,#19401,#9044,.T.);
#23907=EDGE_CURVE('',#19403,#19402,#9045,.T.);
#23908=EDGE_CURVE('',#19399,#19403,#9046,.T.);
#23909=EDGE_CURVE('',#19404,#19405,#9047,.T.);
#23910=EDGE_CURVE('',#19406,#19404,#9048,.T.);
#23911=EDGE_CURVE('',#19407,#19406,#9049,.T.);
#23912=EDGE_CURVE('',#19408,#19407,#9050,.T.);
#23913=EDGE_CURVE('',#19409,#19408,#9051,.T.);
#23914=EDGE_CURVE('',#19405,#19409,#9052,.T.);
#23915=EDGE_CURVE('',#19410,#19411,#9053,.T.);
#23916=EDGE_CURVE('',#19412,#19410,#9054,.T.);
#23917=EDGE_CURVE('',#19413,#19412,#9055,.T.);
#23918=EDGE_CURVE('',#19414,#19413,#9056,.T.);
#23919=EDGE_CURVE('',#19415,#19414,#9057,.T.);
#23920=EDGE_CURVE('',#19411,#19415,#9058,.T.);
#23921=EDGE_CURVE('',#19416,#19417,#9059,.T.);
#23922=EDGE_CURVE('',#19418,#19416,#9060,.T.);
#23923=EDGE_CURVE('',#19419,#19418,#9061,.T.);
#23924=EDGE_CURVE('',#19420,#19419,#9062,.T.);
#23925=EDGE_CURVE('',#19421,#19420,#9063,.T.);
#23926=EDGE_CURVE('',#19417,#19421,#9064,.T.);
#23927=EDGE_CURVE('',#19422,#19423,#9065,.T.);
#23928=EDGE_CURVE('',#19424,#19422,#9066,.T.);
#23929=EDGE_CURVE('',#19425,#19424,#9067,.T.);
#23930=EDGE_CURVE('',#19426,#19425,#9068,.T.);
#23931=EDGE_CURVE('',#19427,#19426,#9069,.T.);
#23932=EDGE_CURVE('',#19423,#19427,#9070,.T.);
#23933=EDGE_CURVE('',#19428,#19429,#9071,.T.);
#23934=EDGE_CURVE('',#19430,#19428,#9072,.T.);
#23935=EDGE_CURVE('',#19431,#19430,#9073,.T.);
#23936=EDGE_CURVE('',#19432,#19431,#9074,.T.);
#23937=EDGE_CURVE('',#19433,#19432,#9075,.T.);
#23938=EDGE_CURVE('',#19429,#19433,#9076,.T.);
#23939=EDGE_CURVE('',#19434,#19435,#9077,.T.);
#23940=EDGE_CURVE('',#19436,#19434,#9078,.T.);
#23941=EDGE_CURVE('',#19437,#19436,#9079,.T.);
#23942=EDGE_CURVE('',#19438,#19437,#9080,.T.);
#23943=EDGE_CURVE('',#19439,#19438,#9081,.T.);
#23944=EDGE_CURVE('',#19435,#19439,#9082,.T.);
#23945=EDGE_CURVE('',#19440,#19441,#9083,.T.);
#23946=EDGE_CURVE('',#19442,#19440,#9084,.T.);
#23947=EDGE_CURVE('',#19443,#19442,#9085,.T.);
#23948=EDGE_CURVE('',#19444,#19443,#9086,.T.);
#23949=EDGE_CURVE('',#19445,#19444,#9087,.T.);
#23950=EDGE_CURVE('',#19441,#19445,#9088,.T.);
#23951=EDGE_CURVE('',#19446,#19447,#9089,.T.);
#23952=EDGE_CURVE('',#19448,#19446,#9090,.T.);
#23953=EDGE_CURVE('',#19449,#19448,#9091,.T.);
#23954=EDGE_CURVE('',#19450,#19449,#9092,.T.);
#23955=EDGE_CURVE('',#19451,#19450,#9093,.T.);
#23956=EDGE_CURVE('',#19447,#19451,#9094,.T.);
#23957=EDGE_CURVE('',#19452,#19453,#9095,.T.);
#23958=EDGE_CURVE('',#19454,#19452,#9096,.T.);
#23959=EDGE_CURVE('',#19455,#19454,#9097,.T.);
#23960=EDGE_CURVE('',#19456,#19455,#9098,.T.);
#23961=EDGE_CURVE('',#19457,#19456,#9099,.T.);
#23962=EDGE_CURVE('',#19453,#19457,#9100,.T.);
#23963=EDGE_CURVE('',#19458,#19459,#9101,.T.);
#23964=EDGE_CURVE('',#19460,#19458,#9102,.T.);
#23965=EDGE_CURVE('',#19461,#19460,#9103,.T.);
#23966=EDGE_CURVE('',#19462,#19461,#9104,.T.);
#23967=EDGE_CURVE('',#19463,#19462,#9105,.T.);
#23968=EDGE_CURVE('',#19459,#19463,#9106,.T.);
#23969=EDGE_CURVE('',#19464,#19465,#9107,.T.);
#23970=EDGE_CURVE('',#19466,#19464,#9108,.T.);
#23971=EDGE_CURVE('',#19467,#19466,#9109,.T.);
#23972=EDGE_CURVE('',#19468,#19467,#9110,.T.);
#23973=EDGE_CURVE('',#19469,#19468,#9111,.T.);
#23974=EDGE_CURVE('',#19465,#19469,#9112,.T.);
#23975=EDGE_CURVE('',#19470,#19471,#9113,.T.);
#23976=EDGE_CURVE('',#19472,#19470,#9114,.T.);
#23977=EDGE_CURVE('',#19473,#19472,#9115,.T.);
#23978=EDGE_CURVE('',#19474,#19473,#9116,.T.);
#23979=EDGE_CURVE('',#19475,#19474,#9117,.T.);
#23980=EDGE_CURVE('',#19471,#19475,#9118,.T.);
#23981=EDGE_CURVE('',#19476,#19477,#9119,.T.);
#23982=EDGE_CURVE('',#19478,#19476,#9120,.T.);
#23983=EDGE_CURVE('',#19479,#19478,#9121,.T.);
#23984=EDGE_CURVE('',#19480,#19479,#9122,.T.);
#23985=EDGE_CURVE('',#19481,#19480,#9123,.T.);
#23986=EDGE_CURVE('',#19477,#19481,#9124,.T.);
#23987=EDGE_CURVE('',#19482,#19483,#9125,.T.);
#23988=EDGE_CURVE('',#19484,#19482,#9126,.T.);
#23989=EDGE_CURVE('',#19485,#19484,#9127,.T.);
#23990=EDGE_CURVE('',#19486,#19485,#9128,.T.);
#23991=EDGE_CURVE('',#19487,#19486,#9129,.T.);
#23992=EDGE_CURVE('',#19483,#19487,#9130,.T.);
#23993=EDGE_CURVE('',#19488,#19489,#9131,.T.);
#23994=EDGE_CURVE('',#19490,#19488,#9132,.T.);
#23995=EDGE_CURVE('',#19491,#19490,#9133,.T.);
#23996=EDGE_CURVE('',#19492,#19491,#9134,.T.);
#23997=EDGE_CURVE('',#19493,#19492,#9135,.T.);
#23998=EDGE_CURVE('',#19489,#19493,#9136,.T.);
#23999=EDGE_CURVE('',#19494,#19495,#9137,.T.);
#24000=EDGE_CURVE('',#19496,#19494,#9138,.T.);
#24001=EDGE_CURVE('',#19497,#19496,#9139,.T.);
#24002=EDGE_CURVE('',#19498,#19497,#9140,.T.);
#24003=EDGE_CURVE('',#19499,#19498,#9141,.T.);
#24004=EDGE_CURVE('',#19495,#19499,#9142,.T.);
#24005=EDGE_CURVE('',#19500,#19501,#9143,.T.);
#24006=EDGE_CURVE('',#19502,#19500,#9144,.T.);
#24007=EDGE_CURVE('',#19503,#19502,#9145,.T.);
#24008=EDGE_CURVE('',#19504,#19503,#9146,.T.);
#24009=EDGE_CURVE('',#19505,#19504,#9147,.T.);
#24010=EDGE_CURVE('',#19501,#19505,#9148,.T.);
#24011=EDGE_CURVE('',#19506,#19507,#9149,.T.);
#24012=EDGE_CURVE('',#19508,#19506,#9150,.T.);
#24013=EDGE_CURVE('',#19509,#19508,#9151,.T.);
#24014=EDGE_CURVE('',#19510,#19509,#9152,.T.);
#24015=EDGE_CURVE('',#19511,#19510,#9153,.T.);
#24016=EDGE_CURVE('',#19507,#19511,#9154,.T.);
#24017=EDGE_CURVE('',#19512,#19513,#9155,.T.);
#24018=EDGE_CURVE('',#19514,#19512,#9156,.T.);
#24019=EDGE_CURVE('',#19515,#19514,#9157,.T.);
#24020=EDGE_CURVE('',#19516,#19515,#9158,.T.);
#24021=EDGE_CURVE('',#19517,#19516,#9159,.T.);
#24022=EDGE_CURVE('',#19513,#19517,#9160,.T.);
#24023=EDGE_CURVE('',#19518,#19519,#9161,.T.);
#24024=EDGE_CURVE('',#19520,#19518,#9162,.T.);
#24025=EDGE_CURVE('',#19521,#19520,#9163,.T.);
#24026=EDGE_CURVE('',#19522,#19521,#9164,.T.);
#24027=EDGE_CURVE('',#19523,#19522,#9165,.T.);
#24028=EDGE_CURVE('',#19519,#19523,#9166,.T.);
#24029=EDGE_CURVE('',#19524,#19525,#9167,.T.);
#24030=EDGE_CURVE('',#19526,#19524,#9168,.T.);
#24031=EDGE_CURVE('',#19527,#19526,#9169,.T.);
#24032=EDGE_CURVE('',#19528,#19527,#9170,.T.);
#24033=EDGE_CURVE('',#19529,#19528,#9171,.T.);
#24034=EDGE_CURVE('',#19525,#19529,#9172,.T.);
#24035=EDGE_CURVE('',#19530,#19531,#9173,.T.);
#24036=EDGE_CURVE('',#19532,#19530,#9174,.T.);
#24037=EDGE_CURVE('',#19533,#19532,#9175,.T.);
#24038=EDGE_CURVE('',#19534,#19533,#9176,.T.);
#24039=EDGE_CURVE('',#19535,#19534,#9177,.T.);
#24040=EDGE_CURVE('',#19531,#19535,#9178,.T.);
#24041=EDGE_CURVE('',#19536,#19537,#9179,.T.);
#24042=EDGE_CURVE('',#19538,#19536,#9180,.T.);
#24043=EDGE_CURVE('',#19539,#19538,#9181,.T.);
#24044=EDGE_CURVE('',#19540,#19539,#9182,.T.);
#24045=EDGE_CURVE('',#19541,#19540,#9183,.T.);
#24046=EDGE_CURVE('',#19537,#19541,#9184,.T.);
#24047=EDGE_CURVE('',#19542,#19543,#9185,.T.);
#24048=EDGE_CURVE('',#19544,#19542,#9186,.T.);
#24049=EDGE_CURVE('',#19545,#19544,#9187,.T.);
#24050=EDGE_CURVE('',#19546,#19545,#9188,.T.);
#24051=EDGE_CURVE('',#19547,#19546,#9189,.T.);
#24052=EDGE_CURVE('',#19543,#19547,#9190,.T.);
#24053=EDGE_CURVE('',#19548,#19549,#9191,.T.);
#24054=EDGE_CURVE('',#19550,#19548,#9192,.T.);
#24055=EDGE_CURVE('',#19551,#19550,#9193,.T.);
#24056=EDGE_CURVE('',#19552,#19551,#9194,.T.);
#24057=EDGE_CURVE('',#19553,#19552,#9195,.T.);
#24058=EDGE_CURVE('',#19549,#19553,#9196,.T.);
#24059=EDGE_CURVE('',#19554,#19555,#9197,.T.);
#24060=EDGE_CURVE('',#19556,#19554,#9198,.T.);
#24061=EDGE_CURVE('',#19557,#19556,#9199,.T.);
#24062=EDGE_CURVE('',#19558,#19557,#9200,.T.);
#24063=EDGE_CURVE('',#19559,#19558,#9201,.T.);
#24064=EDGE_CURVE('',#19555,#19559,#9202,.T.);
#24065=EDGE_CURVE('',#19560,#19561,#9203,.T.);
#24066=EDGE_CURVE('',#19562,#19560,#9204,.T.);
#24067=EDGE_CURVE('',#19563,#19562,#9205,.T.);
#24068=EDGE_CURVE('',#19564,#19563,#9206,.T.);
#24069=EDGE_CURVE('',#19565,#19564,#9207,.T.);
#24070=EDGE_CURVE('',#19561,#19565,#9208,.T.);
#24071=EDGE_CURVE('',#19566,#19567,#9209,.T.);
#24072=EDGE_CURVE('',#19568,#19566,#9210,.T.);
#24073=EDGE_CURVE('',#19569,#19568,#9211,.T.);
#24074=EDGE_CURVE('',#19570,#19569,#9212,.T.);
#24075=EDGE_CURVE('',#19571,#19570,#9213,.T.);
#24076=EDGE_CURVE('',#19567,#19571,#9214,.T.);
#24077=EDGE_CURVE('',#19572,#19573,#9215,.T.);
#24078=EDGE_CURVE('',#19574,#19572,#9216,.T.);
#24079=EDGE_CURVE('',#19575,#19574,#9217,.T.);
#24080=EDGE_CURVE('',#19576,#19575,#9218,.T.);
#24081=EDGE_CURVE('',#19577,#19576,#9219,.T.);
#24082=EDGE_CURVE('',#19573,#19577,#9220,.T.);
#24083=EDGE_CURVE('',#19578,#19579,#9221,.T.);
#24084=EDGE_CURVE('',#19580,#19578,#9222,.T.);
#24085=EDGE_CURVE('',#19581,#19580,#9223,.T.);
#24086=EDGE_CURVE('',#19582,#19581,#9224,.T.);
#24087=EDGE_CURVE('',#19583,#19582,#9225,.T.);
#24088=EDGE_CURVE('',#19579,#19583,#9226,.T.);
#24089=EDGE_CURVE('',#19584,#19585,#9227,.T.);
#24090=EDGE_CURVE('',#19586,#19584,#9228,.T.);
#24091=EDGE_CURVE('',#19587,#19586,#9229,.T.);
#24092=EDGE_CURVE('',#19588,#19587,#9230,.T.);
#24093=EDGE_CURVE('',#19589,#19588,#9231,.T.);
#24094=EDGE_CURVE('',#19585,#19589,#9232,.T.);
#24095=EDGE_CURVE('',#19590,#19591,#9233,.T.);
#24096=EDGE_CURVE('',#19592,#19590,#9234,.T.);
#24097=EDGE_CURVE('',#19593,#19592,#9235,.T.);
#24098=EDGE_CURVE('',#19594,#19593,#9236,.T.);
#24099=EDGE_CURVE('',#19595,#19594,#9237,.T.);
#24100=EDGE_CURVE('',#19591,#19595,#9238,.T.);
#24101=EDGE_CURVE('',#19596,#19597,#9239,.T.);
#24102=EDGE_CURVE('',#19598,#19596,#9240,.T.);
#24103=EDGE_CURVE('',#19599,#19598,#9241,.T.);
#24104=EDGE_CURVE('',#19600,#19599,#9242,.T.);
#24105=EDGE_CURVE('',#19601,#19600,#9243,.T.);
#24106=EDGE_CURVE('',#19597,#19601,#9244,.T.);
#24107=EDGE_CURVE('',#19602,#19603,#9245,.T.);
#24108=EDGE_CURVE('',#19604,#19602,#9246,.T.);
#24109=EDGE_CURVE('',#19605,#19604,#9247,.T.);
#24110=EDGE_CURVE('',#19606,#19605,#9248,.T.);
#24111=EDGE_CURVE('',#19607,#19606,#9249,.T.);
#24112=EDGE_CURVE('',#19603,#19607,#9250,.T.);
#24113=EDGE_CURVE('',#19608,#19609,#9251,.T.);
#24114=EDGE_CURVE('',#19610,#19608,#9252,.T.);
#24115=EDGE_CURVE('',#19611,#19610,#9253,.T.);
#24116=EDGE_CURVE('',#19612,#19611,#9254,.T.);
#24117=EDGE_CURVE('',#19613,#19612,#9255,.T.);
#24118=EDGE_CURVE('',#19609,#19613,#9256,.T.);
#24119=EDGE_CURVE('',#19614,#19615,#9257,.T.);
#24120=EDGE_CURVE('',#19616,#19614,#9258,.T.);
#24121=EDGE_CURVE('',#19617,#19616,#9259,.T.);
#24122=EDGE_CURVE('',#19618,#19617,#9260,.T.);
#24123=EDGE_CURVE('',#19619,#19618,#9261,.T.);
#24124=EDGE_CURVE('',#19615,#19619,#9262,.T.);
#24125=EDGE_CURVE('',#19620,#19621,#9263,.T.);
#24126=EDGE_CURVE('',#19622,#19620,#9264,.T.);
#24127=EDGE_CURVE('',#19623,#19622,#9265,.T.);
#24128=EDGE_CURVE('',#19624,#19623,#9266,.T.);
#24129=EDGE_CURVE('',#19625,#19624,#9267,.T.);
#24130=EDGE_CURVE('',#19621,#19625,#9268,.T.);
#24131=EDGE_CURVE('',#19626,#19627,#9269,.T.);
#24132=EDGE_CURVE('',#19628,#19626,#9270,.T.);
#24133=EDGE_CURVE('',#19629,#19628,#9271,.T.);
#24134=EDGE_CURVE('',#19630,#19629,#9272,.T.);
#24135=EDGE_CURVE('',#19631,#19630,#9273,.T.);
#24136=EDGE_CURVE('',#19627,#19631,#9274,.T.);
#24137=EDGE_CURVE('',#19632,#19633,#9275,.T.);
#24138=EDGE_CURVE('',#19634,#19632,#9276,.T.);
#24139=EDGE_CURVE('',#19635,#19634,#9277,.T.);
#24140=EDGE_CURVE('',#19636,#19635,#9278,.T.);
#24141=EDGE_CURVE('',#19637,#19636,#9279,.T.);
#24142=EDGE_CURVE('',#19633,#19637,#9280,.T.);
#24143=EDGE_CURVE('',#19638,#19639,#9281,.T.);
#24144=EDGE_CURVE('',#19640,#19638,#9282,.T.);
#24145=EDGE_CURVE('',#19641,#19640,#9283,.T.);
#24146=EDGE_CURVE('',#19642,#19641,#9284,.T.);
#24147=EDGE_CURVE('',#19643,#19642,#9285,.T.);
#24148=EDGE_CURVE('',#19639,#19643,#9286,.T.);
#24149=EDGE_CURVE('',#19644,#19645,#9287,.T.);
#24150=EDGE_CURVE('',#19646,#19644,#9288,.T.);
#24151=EDGE_CURVE('',#19647,#19646,#9289,.T.);
#24152=EDGE_CURVE('',#19648,#19647,#9290,.T.);
#24153=EDGE_CURVE('',#19649,#19648,#9291,.T.);
#24154=EDGE_CURVE('',#19645,#19649,#9292,.T.);
#24155=EDGE_CURVE('',#19650,#19651,#9293,.T.);
#24156=EDGE_CURVE('',#19652,#19650,#9294,.T.);
#24157=EDGE_CURVE('',#19653,#19652,#9295,.T.);
#24158=EDGE_CURVE('',#19654,#19653,#9296,.T.);
#24159=EDGE_CURVE('',#19655,#19654,#9297,.T.);
#24160=EDGE_CURVE('',#19651,#19655,#9298,.T.);
#24161=EDGE_CURVE('',#19656,#19657,#9299,.T.);
#24162=EDGE_CURVE('',#19658,#19656,#9300,.T.);
#24163=EDGE_CURVE('',#19659,#19658,#9301,.T.);
#24164=EDGE_CURVE('',#19660,#19659,#9302,.T.);
#24165=EDGE_CURVE('',#19661,#19660,#9303,.T.);
#24166=EDGE_CURVE('',#19657,#19661,#9304,.T.);
#24167=EDGE_CURVE('',#19662,#19663,#9305,.T.);
#24168=EDGE_CURVE('',#19664,#19662,#9306,.T.);
#24169=EDGE_CURVE('',#19665,#19664,#9307,.T.);
#24170=EDGE_CURVE('',#19666,#19665,#9308,.T.);
#24171=EDGE_CURVE('',#19667,#19666,#9309,.T.);
#24172=EDGE_CURVE('',#19663,#19667,#9310,.T.);
#24173=EDGE_CURVE('',#19668,#19669,#9311,.T.);
#24174=EDGE_CURVE('',#19670,#19668,#9312,.T.);
#24175=EDGE_CURVE('',#19671,#19670,#9313,.T.);
#24176=EDGE_CURVE('',#19672,#19671,#9314,.T.);
#24177=EDGE_CURVE('',#19673,#19672,#9315,.T.);
#24178=EDGE_CURVE('',#19669,#19673,#9316,.T.);
#24179=EDGE_CURVE('',#19674,#19675,#9317,.T.);
#24180=EDGE_CURVE('',#19676,#19674,#9318,.T.);
#24181=EDGE_CURVE('',#19677,#19676,#9319,.T.);
#24182=EDGE_CURVE('',#19678,#19677,#9320,.T.);
#24183=EDGE_CURVE('',#19679,#19678,#9321,.T.);
#24184=EDGE_CURVE('',#19675,#19679,#9322,.T.);
#24185=EDGE_CURVE('',#19680,#19681,#9323,.T.);
#24186=EDGE_CURVE('',#19682,#19680,#9324,.T.);
#24187=EDGE_CURVE('',#19683,#19682,#9325,.T.);
#24188=EDGE_CURVE('',#19684,#19683,#9326,.T.);
#24189=EDGE_CURVE('',#19685,#19684,#9327,.T.);
#24190=EDGE_CURVE('',#19681,#19685,#9328,.T.);
#24191=EDGE_CURVE('',#19686,#19687,#9329,.T.);
#24192=EDGE_CURVE('',#19688,#19686,#9330,.T.);
#24193=EDGE_CURVE('',#19689,#19688,#9331,.T.);
#24194=EDGE_CURVE('',#19690,#19689,#9332,.T.);
#24195=EDGE_CURVE('',#19691,#19690,#9333,.T.);
#24196=EDGE_CURVE('',#19687,#19691,#9334,.T.);
#24197=EDGE_CURVE('',#19692,#19693,#9335,.T.);
#24198=EDGE_CURVE('',#19694,#19692,#9336,.T.);
#24199=EDGE_CURVE('',#19695,#19694,#9337,.T.);
#24200=EDGE_CURVE('',#19696,#19695,#9338,.T.);
#24201=EDGE_CURVE('',#19697,#19696,#9339,.T.);
#24202=EDGE_CURVE('',#19693,#19697,#9340,.T.);
#24203=EDGE_CURVE('',#19698,#19699,#9341,.T.);
#24204=EDGE_CURVE('',#19700,#19698,#9342,.T.);
#24205=EDGE_CURVE('',#19701,#19700,#9343,.T.);
#24206=EDGE_CURVE('',#19702,#19701,#9344,.T.);
#24207=EDGE_CURVE('',#19703,#19702,#9345,.T.);
#24208=EDGE_CURVE('',#19699,#19703,#9346,.T.);
#24209=EDGE_CURVE('',#19704,#19705,#9347,.T.);
#24210=EDGE_CURVE('',#19706,#19704,#9348,.T.);
#24211=EDGE_CURVE('',#19707,#19706,#9349,.T.);
#24212=EDGE_CURVE('',#19708,#19707,#9350,.T.);
#24213=EDGE_CURVE('',#19709,#19708,#9351,.T.);
#24214=EDGE_CURVE('',#19705,#19709,#9352,.T.);
#24215=EDGE_CURVE('',#19710,#19711,#9353,.T.);
#24216=EDGE_CURVE('',#19712,#19710,#9354,.T.);
#24217=EDGE_CURVE('',#19713,#19712,#9355,.T.);
#24218=EDGE_CURVE('',#19714,#19713,#9356,.T.);
#24219=EDGE_CURVE('',#19715,#19714,#9357,.T.);
#24220=EDGE_CURVE('',#19711,#19715,#9358,.T.);
#24221=EDGE_CURVE('',#19716,#19717,#9359,.T.);
#24222=EDGE_CURVE('',#19718,#19716,#9360,.T.);
#24223=EDGE_CURVE('',#19719,#19718,#9361,.T.);
#24224=EDGE_CURVE('',#19720,#19719,#9362,.T.);
#24225=EDGE_CURVE('',#19721,#19720,#9363,.T.);
#24226=EDGE_CURVE('',#19717,#19721,#9364,.T.);
#24227=EDGE_CURVE('',#19722,#19723,#9365,.T.);
#24228=EDGE_CURVE('',#19724,#19722,#9366,.T.);
#24229=EDGE_CURVE('',#19725,#19724,#9367,.T.);
#24230=EDGE_CURVE('',#19726,#19725,#9368,.T.);
#24231=EDGE_CURVE('',#19727,#19726,#9369,.T.);
#24232=EDGE_CURVE('',#19723,#19727,#9370,.T.);
#24233=EDGE_CURVE('',#19728,#19729,#9371,.T.);
#24234=EDGE_CURVE('',#19730,#19728,#9372,.T.);
#24235=EDGE_CURVE('',#19731,#19730,#9373,.T.);
#24236=EDGE_CURVE('',#19732,#19731,#9374,.T.);
#24237=EDGE_CURVE('',#19733,#19732,#9375,.T.);
#24238=EDGE_CURVE('',#19729,#19733,#9376,.T.);
#24239=EDGE_CURVE('',#19734,#19735,#9377,.T.);
#24240=EDGE_CURVE('',#19736,#19734,#9378,.T.);
#24241=EDGE_CURVE('',#19737,#19736,#9379,.T.);
#24242=EDGE_CURVE('',#19738,#19737,#9380,.T.);
#24243=EDGE_CURVE('',#19739,#19738,#9381,.T.);
#24244=EDGE_CURVE('',#19735,#19739,#9382,.T.);
#24245=EDGE_CURVE('',#19740,#19741,#9383,.T.);
#24246=EDGE_CURVE('',#19741,#19742,#9384,.T.);
#24247=EDGE_CURVE('',#19742,#19743,#9385,.T.);
#24248=EDGE_CURVE('',#19743,#19744,#9386,.T.);
#24249=EDGE_CURVE('',#19744,#19745,#9387,.T.);
#24250=EDGE_CURVE('',#19745,#19740,#9388,.T.);
#24251=EDGE_CURVE('',#19746,#19747,#9389,.T.);
#24252=EDGE_CURVE('',#19747,#19748,#9390,.T.);
#24253=EDGE_CURVE('',#19748,#19749,#9391,.T.);
#24254=EDGE_CURVE('',#19749,#19750,#9392,.T.);
#24255=EDGE_CURVE('',#19750,#19751,#9393,.T.);
#24256=EDGE_CURVE('',#19751,#19746,#9394,.T.);
#24257=EDGE_CURVE('',#19752,#19753,#9395,.T.);
#24258=EDGE_CURVE('',#19753,#19754,#9396,.T.);
#24259=EDGE_CURVE('',#19754,#19755,#9397,.T.);
#24260=EDGE_CURVE('',#19755,#19756,#9398,.T.);
#24261=EDGE_CURVE('',#19756,#19757,#9399,.T.);
#24262=EDGE_CURVE('',#19757,#19752,#9400,.T.);
#24263=EDGE_CURVE('',#19758,#19759,#9401,.T.);
#24264=EDGE_CURVE('',#19759,#19760,#9402,.T.);
#24265=EDGE_CURVE('',#19760,#19761,#9403,.T.);
#24266=EDGE_CURVE('',#19761,#19762,#9404,.T.);
#24267=EDGE_CURVE('',#19762,#19763,#9405,.T.);
#24268=EDGE_CURVE('',#19763,#19758,#9406,.T.);
#24269=EDGE_CURVE('',#19764,#19765,#9407,.T.);
#24270=EDGE_CURVE('',#19765,#19766,#9408,.T.);
#24271=EDGE_CURVE('',#19766,#19767,#9409,.T.);
#24272=EDGE_CURVE('',#19767,#19768,#9410,.T.);
#24273=EDGE_CURVE('',#19768,#19769,#9411,.T.);
#24274=EDGE_CURVE('',#19769,#19764,#9412,.T.);
#24275=EDGE_CURVE('',#19770,#19771,#9413,.T.);
#24276=EDGE_CURVE('',#19771,#19772,#9414,.T.);
#24277=EDGE_CURVE('',#19772,#19773,#9415,.T.);
#24278=EDGE_CURVE('',#19773,#19774,#9416,.T.);
#24279=EDGE_CURVE('',#19774,#19775,#9417,.T.);
#24280=EDGE_CURVE('',#19775,#19770,#9418,.T.);
#24281=EDGE_CURVE('',#19776,#19777,#9419,.T.);
#24282=EDGE_CURVE('',#19777,#19778,#9420,.T.);
#24283=EDGE_CURVE('',#19778,#19779,#9421,.T.);
#24284=EDGE_CURVE('',#19779,#19780,#9422,.T.);
#24285=EDGE_CURVE('',#19780,#19781,#9423,.T.);
#24286=EDGE_CURVE('',#19781,#19776,#9424,.T.);
#24287=EDGE_CURVE('',#19782,#19783,#9425,.T.);
#24288=EDGE_CURVE('',#19783,#19784,#9426,.T.);
#24289=EDGE_CURVE('',#19784,#19785,#9427,.T.);
#24290=EDGE_CURVE('',#19785,#19786,#9428,.T.);
#24291=EDGE_CURVE('',#19786,#19787,#9429,.T.);
#24292=EDGE_CURVE('',#19787,#19782,#9430,.T.);
#24293=EDGE_CURVE('',#19788,#19789,#9431,.T.);
#24294=EDGE_CURVE('',#19789,#19790,#9432,.T.);
#24295=EDGE_CURVE('',#19790,#19791,#9433,.T.);
#24296=EDGE_CURVE('',#19791,#19792,#9434,.T.);
#24297=EDGE_CURVE('',#19792,#19793,#9435,.T.);
#24298=EDGE_CURVE('',#19793,#19788,#9436,.T.);
#24299=EDGE_CURVE('',#19794,#19795,#9437,.T.);
#24300=EDGE_CURVE('',#19795,#19796,#9438,.T.);
#24301=EDGE_CURVE('',#19796,#19797,#9439,.T.);
#24302=EDGE_CURVE('',#19797,#19798,#9440,.T.);
#24303=EDGE_CURVE('',#19798,#19799,#9441,.T.);
#24304=EDGE_CURVE('',#19799,#19794,#9442,.T.);
#24305=EDGE_CURVE('',#19800,#19801,#9443,.T.);
#24306=EDGE_CURVE('',#19801,#19802,#9444,.T.);
#24307=EDGE_CURVE('',#19802,#19803,#9445,.T.);
#24308=EDGE_CURVE('',#19803,#19804,#9446,.T.);
#24309=EDGE_CURVE('',#19804,#19805,#9447,.T.);
#24310=EDGE_CURVE('',#19805,#19800,#9448,.T.);
#24311=EDGE_CURVE('',#19806,#19807,#9449,.T.);
#24312=EDGE_CURVE('',#19807,#19808,#9450,.T.);
#24313=EDGE_CURVE('',#19808,#19809,#9451,.T.);
#24314=EDGE_CURVE('',#19809,#19810,#9452,.T.);
#24315=EDGE_CURVE('',#19810,#19811,#9453,.T.);
#24316=EDGE_CURVE('',#19811,#19806,#9454,.T.);
#24317=EDGE_CURVE('',#19812,#19813,#9455,.T.);
#24318=EDGE_CURVE('',#19813,#19814,#9456,.T.);
#24319=EDGE_CURVE('',#19814,#19815,#9457,.T.);
#24320=EDGE_CURVE('',#19815,#19816,#9458,.T.);
#24321=EDGE_CURVE('',#19816,#19817,#9459,.T.);
#24322=EDGE_CURVE('',#19817,#19812,#9460,.T.);
#24323=EDGE_CURVE('',#19818,#19819,#9461,.T.);
#24324=EDGE_CURVE('',#19819,#19820,#9462,.T.);
#24325=EDGE_CURVE('',#19820,#19821,#9463,.T.);
#24326=EDGE_CURVE('',#19821,#19822,#9464,.T.);
#24327=EDGE_CURVE('',#19822,#19823,#9465,.T.);
#24328=EDGE_CURVE('',#19823,#19818,#9466,.T.);
#24329=EDGE_CURVE('',#19824,#19825,#9467,.T.);
#24330=EDGE_CURVE('',#19825,#19826,#9468,.T.);
#24331=EDGE_CURVE('',#19826,#19827,#9469,.T.);
#24332=EDGE_CURVE('',#19827,#19828,#9470,.T.);
#24333=EDGE_CURVE('',#19828,#19829,#9471,.T.);
#24334=EDGE_CURVE('',#19829,#19824,#9472,.T.);
#24335=EDGE_CURVE('',#19830,#19831,#9473,.T.);
#24336=EDGE_CURVE('',#19831,#19832,#9474,.T.);
#24337=EDGE_CURVE('',#19832,#19833,#9475,.T.);
#24338=EDGE_CURVE('',#19833,#19834,#9476,.T.);
#24339=EDGE_CURVE('',#19834,#19835,#9477,.T.);
#24340=EDGE_CURVE('',#19835,#19830,#9478,.T.);
#24341=EDGE_CURVE('',#19836,#19837,#9479,.T.);
#24342=EDGE_CURVE('',#19837,#19838,#9480,.T.);
#24343=EDGE_CURVE('',#19838,#19839,#9481,.T.);
#24344=EDGE_CURVE('',#19839,#19840,#9482,.T.);
#24345=EDGE_CURVE('',#19840,#19841,#9483,.T.);
#24346=EDGE_CURVE('',#19841,#19836,#9484,.T.);
#24347=EDGE_CURVE('',#19842,#19843,#9485,.T.);
#24348=EDGE_CURVE('',#19843,#19844,#9486,.T.);
#24349=EDGE_CURVE('',#19844,#19845,#9487,.T.);
#24350=EDGE_CURVE('',#19845,#19846,#9488,.T.);
#24351=EDGE_CURVE('',#19846,#19847,#9489,.T.);
#24352=EDGE_CURVE('',#19847,#19842,#9490,.T.);
#24353=EDGE_CURVE('',#19848,#19849,#9491,.T.);
#24354=EDGE_CURVE('',#19849,#19850,#9492,.T.);
#24355=EDGE_CURVE('',#19850,#19851,#9493,.T.);
#24356=EDGE_CURVE('',#19851,#19852,#9494,.T.);
#24357=EDGE_CURVE('',#19852,#19853,#9495,.T.);
#24358=EDGE_CURVE('',#19853,#19848,#9496,.T.);
#24359=EDGE_CURVE('',#19854,#19855,#9497,.T.);
#24360=EDGE_CURVE('',#19855,#19856,#9498,.T.);
#24361=EDGE_CURVE('',#19856,#19857,#9499,.T.);
#24362=EDGE_CURVE('',#19857,#19858,#9500,.T.);
#24363=EDGE_CURVE('',#19858,#19859,#9501,.T.);
#24364=EDGE_CURVE('',#19859,#19854,#9502,.T.);
#24365=EDGE_CURVE('',#19860,#19861,#9503,.T.);
#24366=EDGE_CURVE('',#19861,#19862,#9504,.T.);
#24367=EDGE_CURVE('',#19862,#19863,#9505,.T.);
#24368=EDGE_CURVE('',#19863,#19864,#9506,.T.);
#24369=EDGE_CURVE('',#19864,#19865,#9507,.T.);
#24370=EDGE_CURVE('',#19865,#19860,#9508,.T.);
#24371=EDGE_CURVE('',#19866,#19867,#9509,.T.);
#24372=EDGE_CURVE('',#19867,#19868,#9510,.T.);
#24373=EDGE_CURVE('',#19868,#19869,#9511,.T.);
#24374=EDGE_CURVE('',#19869,#19870,#9512,.T.);
#24375=EDGE_CURVE('',#19870,#19871,#9513,.T.);
#24376=EDGE_CURVE('',#19871,#19866,#9514,.T.);
#24377=EDGE_CURVE('',#19872,#19873,#9515,.T.);
#24378=EDGE_CURVE('',#19873,#19874,#9516,.T.);
#24379=EDGE_CURVE('',#19874,#19875,#9517,.T.);
#24380=EDGE_CURVE('',#19875,#19876,#9518,.T.);
#24381=EDGE_CURVE('',#19876,#19877,#9519,.T.);
#24382=EDGE_CURVE('',#19877,#19872,#9520,.T.);
#24383=EDGE_CURVE('',#19878,#19879,#9521,.T.);
#24384=EDGE_CURVE('',#19879,#19880,#9522,.T.);
#24385=EDGE_CURVE('',#19880,#19881,#9523,.T.);
#24386=EDGE_CURVE('',#19881,#19882,#9524,.T.);
#24387=EDGE_CURVE('',#19882,#19883,#9525,.T.);
#24388=EDGE_CURVE('',#19883,#19878,#9526,.T.);
#24389=EDGE_CURVE('',#19884,#19885,#9527,.T.);
#24390=EDGE_CURVE('',#19885,#19886,#9528,.T.);
#24391=EDGE_CURVE('',#19886,#19887,#9529,.T.);
#24392=EDGE_CURVE('',#19887,#19888,#9530,.T.);
#24393=EDGE_CURVE('',#19888,#19889,#9531,.T.);
#24394=EDGE_CURVE('',#19889,#19884,#9532,.T.);
#24395=EDGE_CURVE('',#19890,#19891,#9533,.T.);
#24396=EDGE_CURVE('',#19891,#19892,#9534,.T.);
#24397=EDGE_CURVE('',#19892,#19893,#9535,.T.);
#24398=EDGE_CURVE('',#19893,#19894,#9536,.T.);
#24399=EDGE_CURVE('',#19894,#19895,#9537,.T.);
#24400=EDGE_CURVE('',#19895,#19890,#9538,.T.);
#24401=EDGE_CURVE('',#19896,#19897,#9539,.T.);
#24402=EDGE_CURVE('',#19897,#19898,#9540,.T.);
#24403=EDGE_CURVE('',#19898,#19899,#9541,.T.);
#24404=EDGE_CURVE('',#19899,#19900,#9542,.T.);
#24405=EDGE_CURVE('',#19900,#19901,#9543,.T.);
#24406=EDGE_CURVE('',#19901,#19896,#9544,.T.);
#24407=EDGE_CURVE('',#19902,#19903,#9545,.T.);
#24408=EDGE_CURVE('',#19903,#19904,#9546,.T.);
#24409=EDGE_CURVE('',#19904,#19905,#9547,.T.);
#24410=EDGE_CURVE('',#19905,#19906,#9548,.T.);
#24411=EDGE_CURVE('',#19906,#19907,#9549,.T.);
#24412=EDGE_CURVE('',#19907,#19902,#9550,.T.);
#24413=EDGE_CURVE('',#19908,#19909,#9551,.T.);
#24414=EDGE_CURVE('',#19909,#19910,#9552,.T.);
#24415=EDGE_CURVE('',#19910,#19911,#9553,.T.);
#24416=EDGE_CURVE('',#19911,#19912,#9554,.T.);
#24417=EDGE_CURVE('',#19912,#19913,#9555,.T.);
#24418=EDGE_CURVE('',#19913,#19908,#9556,.T.);
#24419=EDGE_CURVE('',#19914,#19915,#9557,.T.);
#24420=EDGE_CURVE('',#19915,#19916,#9558,.T.);
#24421=EDGE_CURVE('',#19916,#19917,#9559,.T.);
#24422=EDGE_CURVE('',#19917,#19918,#9560,.T.);
#24423=EDGE_CURVE('',#19918,#19919,#9561,.T.);
#24424=EDGE_CURVE('',#19919,#19914,#9562,.T.);
#24425=EDGE_CURVE('',#19920,#19921,#9563,.T.);
#24426=EDGE_CURVE('',#19921,#19922,#9564,.T.);
#24427=EDGE_CURVE('',#19922,#19923,#9565,.T.);
#24428=EDGE_CURVE('',#19923,#19924,#9566,.T.);
#24429=EDGE_CURVE('',#19924,#19925,#9567,.T.);
#24430=EDGE_CURVE('',#19925,#19920,#9568,.T.);
#24431=EDGE_CURVE('',#19926,#19927,#9569,.T.);
#24432=EDGE_CURVE('',#19927,#19928,#9570,.T.);
#24433=EDGE_CURVE('',#19928,#19929,#9571,.T.);
#24434=EDGE_CURVE('',#19929,#19930,#9572,.T.);
#24435=EDGE_CURVE('',#19930,#19931,#9573,.T.);
#24436=EDGE_CURVE('',#19931,#19926,#9574,.T.);
#24437=EDGE_CURVE('',#19932,#19933,#9575,.T.);
#24438=EDGE_CURVE('',#19933,#19934,#9576,.T.);
#24439=EDGE_CURVE('',#19934,#19935,#9577,.T.);
#24440=EDGE_CURVE('',#19935,#19936,#9578,.T.);
#24441=EDGE_CURVE('',#19936,#19937,#9579,.T.);
#24442=EDGE_CURVE('',#19937,#19932,#9580,.T.);
#24443=EDGE_CURVE('',#19938,#19939,#9581,.T.);
#24444=EDGE_CURVE('',#19939,#19940,#9582,.T.);
#24445=EDGE_CURVE('',#19940,#19941,#9583,.T.);
#24446=EDGE_CURVE('',#19941,#19942,#9584,.T.);
#24447=EDGE_CURVE('',#19942,#19943,#9585,.T.);
#24448=EDGE_CURVE('',#19943,#19938,#9586,.T.);
#24449=EDGE_CURVE('',#19944,#19945,#9587,.T.);
#24450=EDGE_CURVE('',#19945,#19946,#9588,.T.);
#24451=EDGE_CURVE('',#19946,#19947,#9589,.T.);
#24452=EDGE_CURVE('',#19947,#19948,#9590,.T.);
#24453=EDGE_CURVE('',#19948,#19949,#9591,.T.);
#24454=EDGE_CURVE('',#19949,#19944,#9592,.T.);
#24455=EDGE_CURVE('',#19950,#19951,#9593,.T.);
#24456=EDGE_CURVE('',#19951,#19952,#9594,.T.);
#24457=EDGE_CURVE('',#19952,#19953,#9595,.T.);
#24458=EDGE_CURVE('',#19953,#19954,#9596,.T.);
#24459=EDGE_CURVE('',#19954,#19955,#9597,.T.);
#24460=EDGE_CURVE('',#19955,#19950,#9598,.T.);
#24461=EDGE_CURVE('',#19956,#19957,#9599,.T.);
#24462=EDGE_CURVE('',#19957,#19958,#9600,.T.);
#24463=EDGE_CURVE('',#19958,#19959,#9601,.T.);
#24464=EDGE_CURVE('',#19959,#19960,#9602,.T.);
#24465=EDGE_CURVE('',#19960,#19961,#9603,.T.);
#24466=EDGE_CURVE('',#19961,#19956,#9604,.T.);
#24467=EDGE_CURVE('',#19962,#19963,#9605,.T.);
#24468=EDGE_CURVE('',#19963,#19964,#9606,.T.);
#24469=EDGE_CURVE('',#19964,#19965,#9607,.T.);
#24470=EDGE_CURVE('',#19965,#19966,#9608,.T.);
#24471=EDGE_CURVE('',#19966,#19967,#9609,.T.);
#24472=EDGE_CURVE('',#19967,#19962,#9610,.T.);
#24473=EDGE_CURVE('',#19968,#19969,#9611,.T.);
#24474=EDGE_CURVE('',#19969,#19970,#9612,.T.);
#24475=EDGE_CURVE('',#19970,#19971,#9613,.T.);
#24476=EDGE_CURVE('',#19971,#19972,#9614,.T.);
#24477=EDGE_CURVE('',#19972,#19973,#9615,.T.);
#24478=EDGE_CURVE('',#19973,#19968,#9616,.T.);
#24479=EDGE_CURVE('',#19974,#19975,#9617,.T.);
#24480=EDGE_CURVE('',#19975,#19976,#9618,.T.);
#24481=EDGE_CURVE('',#19976,#19977,#9619,.T.);
#24482=EDGE_CURVE('',#19977,#19978,#9620,.T.);
#24483=EDGE_CURVE('',#19978,#19979,#9621,.T.);
#24484=EDGE_CURVE('',#19979,#19974,#9622,.T.);
#24485=EDGE_CURVE('',#19980,#19981,#9623,.T.);
#24486=EDGE_CURVE('',#19981,#19982,#9624,.T.);
#24487=EDGE_CURVE('',#19982,#19983,#9625,.T.);
#24488=EDGE_CURVE('',#19983,#19984,#9626,.T.);
#24489=EDGE_CURVE('',#19984,#19985,#9627,.T.);
#24490=EDGE_CURVE('',#19985,#19980,#9628,.T.);
#24491=EDGE_CURVE('',#19986,#19987,#9629,.T.);
#24492=EDGE_CURVE('',#19987,#19988,#9630,.T.);
#24493=EDGE_CURVE('',#19988,#19989,#9631,.T.);
#24494=EDGE_CURVE('',#19989,#19990,#9632,.T.);
#24495=EDGE_CURVE('',#19990,#19991,#9633,.T.);
#24496=EDGE_CURVE('',#19991,#19986,#9634,.T.);
#24497=EDGE_CURVE('',#19992,#19993,#9635,.T.);
#24498=EDGE_CURVE('',#19993,#19994,#9636,.T.);
#24499=EDGE_CURVE('',#19994,#19995,#9637,.T.);
#24500=EDGE_CURVE('',#19995,#19996,#9638,.T.);
#24501=EDGE_CURVE('',#19996,#19997,#9639,.T.);
#24502=EDGE_CURVE('',#19997,#19992,#9640,.T.);
#24503=EDGE_CURVE('',#19998,#19999,#9641,.T.);
#24504=EDGE_CURVE('',#19999,#20000,#9642,.T.);
#24505=EDGE_CURVE('',#20000,#20001,#9643,.T.);
#24506=EDGE_CURVE('',#20001,#20002,#9644,.T.);
#24507=EDGE_CURVE('',#20002,#20003,#9645,.T.);
#24508=EDGE_CURVE('',#20003,#19998,#9646,.T.);
#24509=EDGE_CURVE('',#20004,#20005,#9647,.T.);
#24510=EDGE_CURVE('',#20005,#20006,#9648,.T.);
#24511=EDGE_CURVE('',#20006,#20007,#9649,.T.);
#24512=EDGE_CURVE('',#20007,#20008,#9650,.T.);
#24513=EDGE_CURVE('',#20008,#20009,#9651,.T.);
#24514=EDGE_CURVE('',#20009,#20004,#9652,.T.);
#24515=EDGE_CURVE('',#20010,#20011,#9653,.T.);
#24516=EDGE_CURVE('',#20011,#20012,#9654,.T.);
#24517=EDGE_CURVE('',#20012,#20013,#9655,.T.);
#24518=EDGE_CURVE('',#20013,#20014,#9656,.T.);
#24519=EDGE_CURVE('',#20014,#20015,#9657,.T.);
#24520=EDGE_CURVE('',#20015,#20010,#9658,.T.);
#24521=EDGE_CURVE('',#20016,#20017,#9659,.T.);
#24522=EDGE_CURVE('',#20017,#20018,#9660,.T.);
#24523=EDGE_CURVE('',#20018,#20019,#9661,.T.);
#24524=EDGE_CURVE('',#20019,#20020,#9662,.T.);
#24525=EDGE_CURVE('',#20020,#20021,#9663,.T.);
#24526=EDGE_CURVE('',#20021,#20016,#9664,.T.);
#24527=EDGE_CURVE('',#20022,#20023,#9665,.T.);
#24528=EDGE_CURVE('',#20023,#20024,#9666,.T.);
#24529=EDGE_CURVE('',#20024,#20025,#9667,.T.);
#24530=EDGE_CURVE('',#20025,#20026,#9668,.T.);
#24531=EDGE_CURVE('',#20026,#20027,#9669,.T.);
#24532=EDGE_CURVE('',#20027,#20022,#9670,.T.);
#24533=EDGE_CURVE('',#20028,#20029,#9671,.T.);
#24534=EDGE_CURVE('',#20029,#20030,#9672,.T.);
#24535=EDGE_CURVE('',#20030,#20031,#9673,.T.);
#24536=EDGE_CURVE('',#20031,#20032,#9674,.T.);
#24537=EDGE_CURVE('',#20032,#20033,#9675,.T.);
#24538=EDGE_CURVE('',#20033,#20028,#9676,.T.);
#24539=EDGE_CURVE('',#20034,#20035,#9677,.T.);
#24540=EDGE_CURVE('',#20035,#20036,#9678,.T.);
#24541=EDGE_CURVE('',#20036,#20037,#9679,.T.);
#24542=EDGE_CURVE('',#20037,#20038,#9680,.T.);
#24543=EDGE_CURVE('',#20038,#20039,#9681,.T.);
#24544=EDGE_CURVE('',#20039,#20034,#9682,.T.);
#24545=EDGE_CURVE('',#20040,#20041,#9683,.T.);
#24546=EDGE_CURVE('',#20041,#20042,#9684,.T.);
#24547=EDGE_CURVE('',#20042,#20043,#9685,.T.);
#24548=EDGE_CURVE('',#20043,#20044,#9686,.T.);
#24549=EDGE_CURVE('',#20044,#20045,#9687,.T.);
#24550=EDGE_CURVE('',#20045,#20040,#9688,.T.);
#24551=EDGE_CURVE('',#20046,#20047,#9689,.T.);
#24552=EDGE_CURVE('',#20047,#20048,#9690,.T.);
#24553=EDGE_CURVE('',#20048,#20049,#9691,.T.);
#24554=EDGE_CURVE('',#20049,#20050,#9692,.T.);
#24555=EDGE_CURVE('',#20050,#20051,#9693,.T.);
#24556=EDGE_CURVE('',#20051,#20046,#9694,.T.);
#24557=EDGE_CURVE('',#20052,#20053,#9695,.T.);
#24558=EDGE_CURVE('',#20053,#20054,#9696,.T.);
#24559=EDGE_CURVE('',#20054,#20055,#9697,.T.);
#24560=EDGE_CURVE('',#20055,#20056,#9698,.T.);
#24561=EDGE_CURVE('',#20056,#20057,#9699,.T.);
#24562=EDGE_CURVE('',#20057,#20052,#9700,.T.);
#24563=EDGE_CURVE('',#20058,#20059,#9701,.T.);
#24564=EDGE_CURVE('',#20059,#20060,#9702,.T.);
#24565=EDGE_CURVE('',#20060,#20061,#9703,.T.);
#24566=EDGE_CURVE('',#20061,#20062,#9704,.T.);
#24567=EDGE_CURVE('',#20062,#20063,#9705,.T.);
#24568=EDGE_CURVE('',#20063,#20058,#9706,.T.);
#24569=EDGE_CURVE('',#20064,#20065,#9707,.T.);
#24570=EDGE_CURVE('',#20065,#20066,#9708,.T.);
#24571=EDGE_CURVE('',#20066,#20067,#9709,.T.);
#24572=EDGE_CURVE('',#20067,#20068,#9710,.T.);
#24573=EDGE_CURVE('',#20068,#20069,#9711,.T.);
#24574=EDGE_CURVE('',#20069,#20064,#9712,.T.);
#24575=EDGE_CURVE('',#20070,#20071,#9713,.T.);
#24576=EDGE_CURVE('',#20071,#20072,#9714,.T.);
#24577=EDGE_CURVE('',#20072,#20073,#9715,.T.);
#24578=EDGE_CURVE('',#20073,#20074,#9716,.T.);
#24579=EDGE_CURVE('',#20074,#20075,#9717,.T.);
#24580=EDGE_CURVE('',#20075,#20070,#9718,.T.);
#24581=EDGE_CURVE('',#20076,#20077,#9719,.T.);
#24582=EDGE_CURVE('',#20077,#20078,#9720,.T.);
#24583=EDGE_CURVE('',#20078,#20079,#9721,.T.);
#24584=EDGE_CURVE('',#20079,#20080,#9722,.T.);
#24585=EDGE_CURVE('',#20080,#20081,#9723,.T.);
#24586=EDGE_CURVE('',#20081,#20076,#9724,.T.);
#24587=EDGE_CURVE('',#20082,#20083,#9725,.T.);
#24588=EDGE_CURVE('',#20083,#20084,#9726,.T.);
#24589=EDGE_CURVE('',#20084,#20085,#9727,.T.);
#24590=EDGE_CURVE('',#20085,#20086,#9728,.T.);
#24591=EDGE_CURVE('',#20086,#20087,#9729,.T.);
#24592=EDGE_CURVE('',#20087,#20082,#9730,.T.);
#24593=EDGE_CURVE('',#20088,#20089,#9731,.T.);
#24594=EDGE_CURVE('',#20089,#20090,#9732,.T.);
#24595=EDGE_CURVE('',#20090,#20091,#9733,.T.);
#24596=EDGE_CURVE('',#20091,#20092,#9734,.T.);
#24597=EDGE_CURVE('',#20092,#20093,#9735,.T.);
#24598=EDGE_CURVE('',#20093,#20088,#9736,.T.);
#24599=EDGE_CURVE('',#20094,#20095,#9737,.T.);
#24600=EDGE_CURVE('',#20095,#20096,#9738,.T.);
#24601=EDGE_CURVE('',#20096,#20097,#9739,.T.);
#24602=EDGE_CURVE('',#20097,#20098,#9740,.T.);
#24603=EDGE_CURVE('',#20098,#20099,#9741,.T.);
#24604=EDGE_CURVE('',#20099,#20094,#9742,.T.);
#24605=EDGE_CURVE('',#20100,#20101,#9743,.T.);
#24606=EDGE_CURVE('',#20101,#20102,#9744,.T.);
#24607=EDGE_CURVE('',#20102,#20103,#9745,.T.);
#24608=EDGE_CURVE('',#20103,#20104,#9746,.T.);
#24609=EDGE_CURVE('',#20104,#20105,#9747,.T.);
#24610=EDGE_CURVE('',#20105,#20100,#9748,.T.);
#24611=EDGE_CURVE('',#20106,#20107,#9749,.T.);
#24612=EDGE_CURVE('',#20107,#20108,#9750,.T.);
#24613=EDGE_CURVE('',#20108,#20109,#9751,.T.);
#24614=EDGE_CURVE('',#20109,#20110,#9752,.T.);
#24615=EDGE_CURVE('',#20110,#20111,#9753,.T.);
#24616=EDGE_CURVE('',#20111,#20106,#9754,.T.);
#24617=EDGE_CURVE('',#20112,#20113,#9755,.T.);
#24618=EDGE_CURVE('',#20113,#20114,#9756,.T.);
#24619=EDGE_CURVE('',#20114,#20115,#9757,.T.);
#24620=EDGE_CURVE('',#20115,#20116,#9758,.T.);
#24621=EDGE_CURVE('',#20116,#20117,#9759,.T.);
#24622=EDGE_CURVE('',#20117,#20112,#9760,.T.);
#24623=EDGE_CURVE('',#20118,#20119,#9761,.T.);
#24624=EDGE_CURVE('',#20119,#20120,#9762,.T.);
#24625=EDGE_CURVE('',#20120,#20121,#9763,.T.);
#24626=EDGE_CURVE('',#20121,#20122,#9764,.T.);
#24627=EDGE_CURVE('',#20122,#20123,#9765,.T.);
#24628=EDGE_CURVE('',#20123,#20118,#9766,.T.);
#24629=EDGE_CURVE('',#20124,#20125,#9767,.T.);
#24630=EDGE_CURVE('',#20125,#20126,#9768,.T.);
#24631=EDGE_CURVE('',#20126,#20127,#9769,.T.);
#24632=EDGE_CURVE('',#20127,#20128,#9770,.T.);
#24633=EDGE_CURVE('',#20128,#20129,#9771,.T.);
#24634=EDGE_CURVE('',#20129,#20124,#9772,.T.);
#24635=EDGE_CURVE('',#20130,#20131,#9773,.T.);
#24636=EDGE_CURVE('',#20131,#20132,#9774,.T.);
#24637=EDGE_CURVE('',#20132,#20133,#9775,.T.);
#24638=EDGE_CURVE('',#20133,#20134,#9776,.T.);
#24639=EDGE_CURVE('',#20134,#20135,#9777,.T.);
#24640=EDGE_CURVE('',#20135,#20130,#9778,.T.);
#24641=EDGE_CURVE('',#20136,#20137,#9779,.T.);
#24642=EDGE_CURVE('',#20137,#20138,#9780,.T.);
#24643=EDGE_CURVE('',#20138,#20139,#9781,.T.);
#24644=EDGE_CURVE('',#20139,#20140,#9782,.T.);
#24645=EDGE_CURVE('',#20140,#20141,#9783,.T.);
#24646=EDGE_CURVE('',#20141,#20136,#9784,.T.);
#24647=EDGE_CURVE('',#20142,#20143,#9785,.T.);
#24648=EDGE_CURVE('',#20143,#20144,#9786,.T.);
#24649=EDGE_CURVE('',#20144,#20145,#9787,.T.);
#24650=EDGE_CURVE('',#20145,#20146,#9788,.T.);
#24651=EDGE_CURVE('',#20146,#20147,#9789,.T.);
#24652=EDGE_CURVE('',#20147,#20142,#9790,.T.);
#24653=EDGE_CURVE('',#20148,#20149,#9791,.T.);
#24654=EDGE_CURVE('',#20149,#20150,#9792,.T.);
#24655=EDGE_CURVE('',#20150,#20151,#9793,.T.);
#24656=EDGE_CURVE('',#20151,#20152,#9794,.T.);
#24657=EDGE_CURVE('',#20152,#20153,#9795,.T.);
#24658=EDGE_CURVE('',#20153,#20148,#9796,.T.);
#24659=EDGE_CURVE('',#20154,#20155,#9797,.T.);
#24660=EDGE_CURVE('',#20155,#20156,#9798,.T.);
#24661=EDGE_CURVE('',#20156,#20157,#9799,.T.);
#24662=EDGE_CURVE('',#20157,#20158,#9800,.T.);
#24663=EDGE_CURVE('',#20158,#20159,#9801,.T.);
#24664=EDGE_CURVE('',#20159,#20154,#9802,.T.);
#24665=EDGE_CURVE('',#20160,#20161,#9803,.T.);
#24666=EDGE_CURVE('',#20161,#20162,#9804,.T.);
#24667=EDGE_CURVE('',#20162,#20163,#9805,.T.);
#24668=EDGE_CURVE('',#20163,#20164,#9806,.T.);
#24669=EDGE_CURVE('',#20164,#20165,#9807,.T.);
#24670=EDGE_CURVE('',#20165,#20160,#9808,.T.);
#24671=EDGE_CURVE('',#20166,#20167,#9809,.T.);
#24672=EDGE_CURVE('',#20167,#20168,#9810,.T.);
#24673=EDGE_CURVE('',#20168,#20169,#9811,.T.);
#24674=EDGE_CURVE('',#20169,#20170,#9812,.T.);
#24675=EDGE_CURVE('',#20170,#20171,#9813,.T.);
#24676=EDGE_CURVE('',#20171,#20166,#9814,.T.);
#24677=EDGE_CURVE('',#20172,#20173,#9815,.T.);
#24678=EDGE_CURVE('',#20173,#20174,#9816,.T.);
#24679=EDGE_CURVE('',#20174,#20175,#9817,.T.);
#24680=EDGE_CURVE('',#20175,#20176,#9818,.T.);
#24681=EDGE_CURVE('',#20176,#20177,#9819,.T.);
#24682=EDGE_CURVE('',#20177,#20172,#9820,.T.);
#24683=EDGE_CURVE('',#20178,#20179,#9821,.T.);
#24684=EDGE_CURVE('',#20179,#20180,#9822,.T.);
#24685=EDGE_CURVE('',#20180,#20181,#9823,.T.);
#24686=EDGE_CURVE('',#20181,#20182,#9824,.T.);
#24687=EDGE_CURVE('',#20182,#20183,#9825,.T.);
#24688=EDGE_CURVE('',#20183,#20178,#9826,.T.);
#24689=EDGE_CURVE('',#20184,#20185,#9827,.T.);
#24690=EDGE_CURVE('',#20185,#20186,#9828,.T.);
#24691=EDGE_CURVE('',#20186,#20187,#9829,.T.);
#24692=EDGE_CURVE('',#20187,#20188,#9830,.T.);
#24693=EDGE_CURVE('',#20188,#20189,#9831,.T.);
#24694=EDGE_CURVE('',#20189,#20184,#9832,.T.);
#24695=EDGE_CURVE('',#20190,#20191,#9833,.T.);
#24696=EDGE_CURVE('',#20191,#20192,#9834,.T.);
#24697=EDGE_CURVE('',#20192,#20193,#9835,.T.);
#24698=EDGE_CURVE('',#20193,#20194,#9836,.T.);
#24699=EDGE_CURVE('',#20194,#20195,#9837,.T.);
#24700=EDGE_CURVE('',#20195,#20190,#9838,.T.);
#24701=EDGE_CURVE('',#20196,#20197,#9839,.T.);
#24702=EDGE_CURVE('',#20197,#20198,#9840,.T.);
#24703=EDGE_CURVE('',#20198,#20199,#9841,.T.);
#24704=EDGE_CURVE('',#20199,#20200,#9842,.T.);
#24705=EDGE_CURVE('',#20200,#20201,#9843,.T.);
#24706=EDGE_CURVE('',#20201,#20196,#9844,.T.);
#24707=EDGE_CURVE('',#20202,#20203,#9845,.T.);
#24708=EDGE_CURVE('',#20203,#20204,#9846,.T.);
#24709=EDGE_CURVE('',#20204,#20205,#9847,.T.);
#24710=EDGE_CURVE('',#20205,#20206,#9848,.T.);
#24711=EDGE_CURVE('',#20206,#20207,#9849,.T.);
#24712=EDGE_CURVE('',#20207,#20202,#9850,.T.);
#24713=EDGE_CURVE('',#20208,#20209,#9851,.T.);
#24714=EDGE_CURVE('',#20209,#20210,#9852,.T.);
#24715=EDGE_CURVE('',#20210,#20211,#9853,.T.);
#24716=EDGE_CURVE('',#20211,#20212,#9854,.T.);
#24717=EDGE_CURVE('',#20212,#20213,#9855,.T.);
#24718=EDGE_CURVE('',#20213,#20208,#9856,.T.);
#24719=EDGE_CURVE('',#20214,#20215,#9857,.T.);
#24720=EDGE_CURVE('',#20215,#20216,#9858,.T.);
#24721=EDGE_CURVE('',#20216,#20217,#9859,.T.);
#24722=EDGE_CURVE('',#20217,#20218,#9860,.T.);
#24723=EDGE_CURVE('',#20218,#20219,#9861,.T.);
#24724=EDGE_CURVE('',#20219,#20214,#9862,.T.);
#24725=EDGE_CURVE('',#20220,#20221,#9863,.T.);
#24726=EDGE_CURVE('',#20221,#20222,#9864,.T.);
#24727=EDGE_CURVE('',#20222,#20223,#9865,.T.);
#24728=EDGE_CURVE('',#20223,#20224,#9866,.T.);
#24729=EDGE_CURVE('',#20224,#20225,#9867,.T.);
#24730=EDGE_CURVE('',#20225,#20220,#9868,.T.);
#24731=EDGE_CURVE('',#20226,#20227,#9869,.T.);
#24732=EDGE_CURVE('',#20227,#20228,#9870,.T.);
#24733=EDGE_CURVE('',#20228,#20229,#9871,.T.);
#24734=EDGE_CURVE('',#20229,#20230,#9872,.T.);
#24735=EDGE_CURVE('',#20230,#20231,#9873,.T.);
#24736=EDGE_CURVE('',#20231,#20226,#9874,.T.);
#24737=EDGE_CURVE('',#20232,#20233,#9875,.T.);
#24738=EDGE_CURVE('',#20233,#20234,#9876,.T.);
#24739=EDGE_CURVE('',#20234,#20235,#9877,.T.);
#24740=EDGE_CURVE('',#20235,#20236,#9878,.T.);
#24741=EDGE_CURVE('',#20236,#20237,#9879,.T.);
#24742=EDGE_CURVE('',#20237,#20232,#9880,.T.);
#24743=EDGE_CURVE('',#20238,#20239,#9881,.T.);
#24744=EDGE_CURVE('',#20239,#20240,#9882,.T.);
#24745=EDGE_CURVE('',#20240,#20241,#9883,.T.);
#24746=EDGE_CURVE('',#20241,#20242,#9884,.T.);
#24747=EDGE_CURVE('',#20242,#20243,#9885,.T.);
#24748=EDGE_CURVE('',#20243,#20238,#9886,.T.);
#24749=EDGE_CURVE('',#20244,#20245,#9887,.T.);
#24750=EDGE_CURVE('',#20245,#20246,#9888,.T.);
#24751=EDGE_CURVE('',#20246,#20247,#9889,.T.);
#24752=EDGE_CURVE('',#20247,#20248,#9890,.T.);
#24753=EDGE_CURVE('',#20248,#20249,#9891,.T.);
#24754=EDGE_CURVE('',#20249,#20244,#9892,.T.);
#24755=EDGE_CURVE('',#20250,#20251,#9893,.T.);
#24756=EDGE_CURVE('',#20251,#20252,#9894,.T.);
#24757=EDGE_CURVE('',#20252,#20253,#9895,.T.);
#24758=EDGE_CURVE('',#20253,#20254,#9896,.T.);
#24759=EDGE_CURVE('',#20254,#20255,#9897,.T.);
#24760=EDGE_CURVE('',#20255,#20250,#9898,.T.);
#24761=EDGE_CURVE('',#20256,#20257,#9899,.T.);
#24762=EDGE_CURVE('',#20257,#20258,#9900,.T.);
#24763=EDGE_CURVE('',#20258,#20259,#9901,.T.);
#24764=EDGE_CURVE('',#20259,#20260,#9902,.T.);
#24765=EDGE_CURVE('',#20260,#20261,#9903,.T.);
#24766=EDGE_CURVE('',#20261,#20256,#9904,.T.);
#24767=EDGE_CURVE('',#20262,#20263,#9905,.T.);
#24768=EDGE_CURVE('',#20263,#20264,#9906,.T.);
#24769=EDGE_CURVE('',#20264,#20265,#9907,.T.);
#24770=EDGE_CURVE('',#20265,#20266,#9908,.T.);
#24771=EDGE_CURVE('',#20266,#20267,#9909,.T.);
#24772=EDGE_CURVE('',#20267,#20262,#9910,.T.);
#24773=EDGE_CURVE('',#20268,#20269,#9911,.T.);
#24774=EDGE_CURVE('',#20269,#20270,#9912,.T.);
#24775=EDGE_CURVE('',#20270,#20271,#9913,.T.);
#24776=EDGE_CURVE('',#20271,#20272,#9914,.T.);
#24777=EDGE_CURVE('',#20272,#20273,#9915,.T.);
#24778=EDGE_CURVE('',#20273,#20268,#9916,.T.);
#24779=EDGE_CURVE('',#20274,#20275,#9917,.T.);
#24780=EDGE_CURVE('',#20275,#20276,#9918,.T.);
#24781=EDGE_CURVE('',#20276,#20277,#9919,.T.);
#24782=EDGE_CURVE('',#20277,#20278,#9920,.T.);
#24783=EDGE_CURVE('',#20278,#20279,#9921,.T.);
#24784=EDGE_CURVE('',#20279,#20274,#9922,.T.);
#24785=EDGE_CURVE('',#20280,#20281,#9923,.T.);
#24786=EDGE_CURVE('',#20281,#20282,#9924,.T.);
#24787=EDGE_CURVE('',#20282,#20283,#9925,.T.);
#24788=EDGE_CURVE('',#20283,#20284,#9926,.T.);
#24789=EDGE_CURVE('',#20284,#20285,#9927,.T.);
#24790=EDGE_CURVE('',#20285,#20280,#9928,.T.);
#24791=EDGE_CURVE('',#20286,#20287,#9929,.T.);
#24792=EDGE_CURVE('',#20287,#20288,#9930,.T.);
#24793=EDGE_CURVE('',#20288,#20289,#9931,.T.);
#24794=EDGE_CURVE('',#20289,#20290,#9932,.T.);
#24795=EDGE_CURVE('',#20290,#20291,#9933,.T.);
#24796=EDGE_CURVE('',#20291,#20286,#9934,.T.);
#24797=EDGE_CURVE('',#20292,#20293,#9935,.T.);
#24798=EDGE_CURVE('',#20293,#20294,#9936,.T.);
#24799=EDGE_CURVE('',#20294,#20295,#9937,.T.);
#24800=EDGE_CURVE('',#20295,#20296,#9938,.T.);
#24801=EDGE_CURVE('',#20296,#20297,#9939,.T.);
#24802=EDGE_CURVE('',#20297,#20292,#9940,.T.);
#24803=EDGE_CURVE('',#20298,#20299,#9941,.T.);
#24804=EDGE_CURVE('',#20299,#20300,#9942,.T.);
#24805=EDGE_CURVE('',#20300,#20301,#9943,.T.);
#24806=EDGE_CURVE('',#20301,#20302,#9944,.T.);
#24807=EDGE_CURVE('',#20302,#20303,#9945,.T.);
#24808=EDGE_CURVE('',#20303,#20298,#9946,.T.);
#24809=EDGE_CURVE('',#20304,#20305,#9947,.T.);
#24810=EDGE_CURVE('',#20305,#20306,#9948,.T.);
#24811=EDGE_CURVE('',#20306,#20307,#9949,.T.);
#24812=EDGE_CURVE('',#20307,#20308,#9950,.T.);
#24813=EDGE_CURVE('',#20308,#20309,#9951,.T.);
#24814=EDGE_CURVE('',#20309,#20304,#9952,.T.);
#24815=EDGE_CURVE('',#20310,#20311,#9953,.T.);
#24816=EDGE_CURVE('',#20311,#20312,#9954,.T.);
#24817=EDGE_CURVE('',#20312,#20313,#9955,.T.);
#24818=EDGE_CURVE('',#20313,#20314,#9956,.T.);
#24819=EDGE_CURVE('',#20314,#20315,#9957,.T.);
#24820=EDGE_CURVE('',#20315,#20310,#9958,.T.);
#24821=EDGE_CURVE('',#20316,#20317,#9959,.T.);
#24822=EDGE_CURVE('',#20317,#20318,#9960,.T.);
#24823=EDGE_CURVE('',#20318,#20319,#9961,.T.);
#24824=EDGE_CURVE('',#20319,#20320,#9962,.T.);
#24825=EDGE_CURVE('',#20320,#20321,#9963,.T.);
#24826=EDGE_CURVE('',#20321,#20316,#9964,.T.);
#24827=EDGE_CURVE('',#20322,#20323,#9965,.T.);
#24828=EDGE_CURVE('',#20323,#20324,#9966,.T.);
#24829=EDGE_CURVE('',#20324,#20325,#9967,.T.);
#24830=EDGE_CURVE('',#20325,#20326,#9968,.T.);
#24831=EDGE_CURVE('',#20326,#20327,#9969,.T.);
#24832=EDGE_CURVE('',#20327,#20322,#9970,.T.);
#24833=EDGE_CURVE('',#20328,#20329,#9971,.T.);
#24834=EDGE_CURVE('',#20329,#20330,#9972,.T.);
#24835=EDGE_CURVE('',#20330,#20331,#9973,.T.);
#24836=EDGE_CURVE('',#20331,#20332,#9974,.T.);
#24837=EDGE_CURVE('',#20332,#20333,#9975,.T.);
#24838=EDGE_CURVE('',#20333,#20328,#9976,.T.);
#24839=EDGE_CURVE('',#20334,#20335,#9977,.T.);
#24840=EDGE_CURVE('',#20335,#20336,#9978,.T.);
#24841=EDGE_CURVE('',#20336,#20337,#9979,.T.);
#24842=EDGE_CURVE('',#20337,#20338,#9980,.T.);
#24843=EDGE_CURVE('',#20338,#20339,#9981,.T.);
#24844=EDGE_CURVE('',#20339,#20334,#9982,.T.);
#24845=EDGE_CURVE('',#20340,#20341,#9983,.T.);
#24846=EDGE_CURVE('',#20341,#20342,#9984,.T.);
#24847=EDGE_CURVE('',#20342,#20343,#9985,.T.);
#24848=EDGE_CURVE('',#20343,#20344,#9986,.T.);
#24849=EDGE_CURVE('',#20344,#20345,#9987,.T.);
#24850=EDGE_CURVE('',#20345,#20340,#9988,.T.);
#24851=EDGE_CURVE('',#20346,#20347,#9989,.T.);
#24852=EDGE_CURVE('',#20347,#20348,#9990,.T.);
#24853=EDGE_CURVE('',#20348,#20349,#9991,.T.);
#24854=EDGE_CURVE('',#20349,#20350,#9992,.T.);
#24855=EDGE_CURVE('',#20350,#20351,#9993,.T.);
#24856=EDGE_CURVE('',#20351,#20346,#9994,.T.);
#24857=EDGE_CURVE('',#20352,#20353,#9995,.T.);
#24858=EDGE_CURVE('',#20353,#20354,#9996,.T.);
#24859=EDGE_CURVE('',#20354,#20355,#9997,.T.);
#24860=EDGE_CURVE('',#20355,#20356,#9998,.T.);
#24861=EDGE_CURVE('',#20356,#20357,#9999,.T.);
#24862=EDGE_CURVE('',#20357,#20352,#10000,.T.);
#24863=EDGE_CURVE('',#20358,#20359,#10001,.T.);
#24864=EDGE_CURVE('',#20359,#20360,#10002,.T.);
#24865=EDGE_CURVE('',#20360,#20361,#10003,.T.);
#24866=EDGE_CURVE('',#20361,#20362,#10004,.T.);
#24867=EDGE_CURVE('',#20362,#20363,#10005,.T.);
#24868=EDGE_CURVE('',#20363,#20358,#10006,.T.);
#24869=EDGE_CURVE('',#20364,#20365,#10007,.T.);
#24870=EDGE_CURVE('',#20365,#20366,#10008,.T.);
#24871=EDGE_CURVE('',#20366,#20367,#10009,.T.);
#24872=EDGE_CURVE('',#20367,#20368,#10010,.T.);
#24873=EDGE_CURVE('',#20368,#20369,#10011,.T.);
#24874=EDGE_CURVE('',#20369,#20364,#10012,.T.);
#24875=EDGE_CURVE('',#20370,#20371,#10013,.T.);
#24876=EDGE_CURVE('',#20371,#20372,#10014,.T.);
#24877=EDGE_CURVE('',#20372,#20373,#10015,.T.);
#24878=EDGE_CURVE('',#20373,#20374,#10016,.T.);
#24879=EDGE_CURVE('',#20374,#20375,#10017,.T.);
#24880=EDGE_CURVE('',#20375,#20370,#10018,.T.);
#24881=EDGE_CURVE('',#20376,#20377,#10019,.T.);
#24882=EDGE_CURVE('',#20377,#20378,#10020,.T.);
#24883=EDGE_CURVE('',#20378,#20379,#10021,.T.);
#24884=EDGE_CURVE('',#20379,#20380,#10022,.T.);
#24885=EDGE_CURVE('',#20380,#20381,#10023,.T.);
#24886=EDGE_CURVE('',#20381,#20376,#10024,.T.);
#24887=EDGE_CURVE('',#20382,#20383,#10025,.T.);
#24888=EDGE_CURVE('',#20383,#20384,#10026,.T.);
#24889=EDGE_CURVE('',#20384,#20385,#10027,.T.);
#24890=EDGE_CURVE('',#20385,#20386,#10028,.T.);
#24891=EDGE_CURVE('',#20386,#20387,#10029,.T.);
#24892=EDGE_CURVE('',#20387,#20382,#10030,.T.);
#24893=EDGE_CURVE('',#20388,#20389,#10031,.T.);
#24894=EDGE_CURVE('',#20389,#20390,#10032,.T.);
#24895=EDGE_CURVE('',#20390,#20391,#10033,.T.);
#24896=EDGE_CURVE('',#20391,#20392,#10034,.T.);
#24897=EDGE_CURVE('',#20392,#20393,#10035,.T.);
#24898=EDGE_CURVE('',#20393,#20388,#10036,.T.);
#24899=EDGE_CURVE('',#20394,#20395,#10037,.T.);
#24900=EDGE_CURVE('',#20395,#20396,#10038,.T.);
#24901=EDGE_CURVE('',#20396,#20397,#10039,.T.);
#24902=EDGE_CURVE('',#20397,#20398,#10040,.T.);
#24903=EDGE_CURVE('',#20398,#20399,#10041,.T.);
#24904=EDGE_CURVE('',#20399,#20394,#10042,.T.);
#24905=EDGE_CURVE('',#20400,#20401,#10043,.T.);
#24906=EDGE_CURVE('',#20401,#20402,#10044,.T.);
#24907=EDGE_CURVE('',#20402,#20403,#10045,.T.);
#24908=EDGE_CURVE('',#20403,#20404,#10046,.T.);
#24909=EDGE_CURVE('',#20404,#20405,#10047,.T.);
#24910=EDGE_CURVE('',#20405,#20400,#10048,.T.);
#24911=EDGE_CURVE('',#20406,#20407,#10049,.T.);
#24912=EDGE_CURVE('',#20407,#20408,#10050,.T.);
#24913=EDGE_CURVE('',#20408,#20409,#10051,.T.);
#24914=EDGE_CURVE('',#20409,#20410,#10052,.T.);
#24915=EDGE_CURVE('',#20410,#20411,#10053,.T.);
#24916=EDGE_CURVE('',#20411,#20406,#10054,.T.);
#24917=EDGE_CURVE('',#20412,#20413,#10055,.T.);
#24918=EDGE_CURVE('',#20413,#20414,#10056,.T.);
#24919=EDGE_CURVE('',#20414,#20415,#10057,.T.);
#24920=EDGE_CURVE('',#20415,#20416,#10058,.T.);
#24921=EDGE_CURVE('',#20416,#20417,#10059,.T.);
#24922=EDGE_CURVE('',#20417,#20412,#10060,.T.);
#24923=EDGE_CURVE('',#20418,#20419,#10061,.T.);
#24924=EDGE_CURVE('',#20419,#20420,#10062,.T.);
#24925=EDGE_CURVE('',#20420,#20421,#10063,.T.);
#24926=EDGE_CURVE('',#20421,#20422,#10064,.T.);
#24927=EDGE_CURVE('',#20422,#20423,#10065,.T.);
#24928=EDGE_CURVE('',#20423,#20418,#10066,.T.);
#24929=EDGE_CURVE('',#20424,#20425,#10067,.T.);
#24930=EDGE_CURVE('',#20425,#20426,#10068,.T.);
#24931=EDGE_CURVE('',#20426,#20427,#10069,.T.);
#24932=EDGE_CURVE('',#20427,#20428,#10070,.T.);
#24933=EDGE_CURVE('',#20428,#20429,#10071,.T.);
#24934=EDGE_CURVE('',#20429,#20424,#10072,.T.);
#24935=EDGE_CURVE('',#20430,#20431,#10073,.T.);
#24936=EDGE_CURVE('',#20431,#20432,#10074,.T.);
#24937=EDGE_CURVE('',#20432,#20433,#10075,.T.);
#24938=EDGE_CURVE('',#20433,#20434,#10076,.T.);
#24939=EDGE_CURVE('',#20434,#20435,#10077,.T.);
#24940=EDGE_CURVE('',#20435,#20430,#10078,.T.);
#24941=EDGE_CURVE('',#20436,#20437,#10079,.T.);
#24942=EDGE_CURVE('',#20437,#20438,#10080,.T.);
#24943=EDGE_CURVE('',#20438,#20439,#10081,.T.);
#24944=EDGE_CURVE('',#20439,#20440,#10082,.T.);
#24945=EDGE_CURVE('',#20440,#20441,#10083,.T.);
#24946=EDGE_CURVE('',#20441,#20436,#10084,.T.);
#24947=EDGE_CURVE('',#20442,#20443,#10085,.T.);
#24948=EDGE_CURVE('',#20443,#20444,#10086,.T.);
#24949=EDGE_CURVE('',#20444,#20445,#10087,.T.);
#24950=EDGE_CURVE('',#20445,#20446,#10088,.T.);
#24951=EDGE_CURVE('',#20446,#20447,#10089,.T.);
#24952=EDGE_CURVE('',#20447,#20442,#10090,.T.);
#24953=EDGE_CURVE('',#20448,#20449,#10091,.T.);
#24954=EDGE_CURVE('',#20449,#20450,#10092,.T.);
#24955=EDGE_CURVE('',#20450,#20451,#10093,.T.);
#24956=EDGE_CURVE('',#20451,#20452,#10094,.T.);
#24957=EDGE_CURVE('',#20452,#20453,#10095,.T.);
#24958=EDGE_CURVE('',#20453,#20448,#10096,.T.);
#24959=EDGE_CURVE('',#20454,#20455,#10097,.T.);
#24960=EDGE_CURVE('',#20455,#20456,#10098,.T.);
#24961=EDGE_CURVE('',#20456,#20457,#10099,.T.);
#24962=EDGE_CURVE('',#20457,#20458,#10100,.T.);
#24963=EDGE_CURVE('',#20458,#20459,#10101,.T.);
#24964=EDGE_CURVE('',#20459,#20454,#10102,.T.);
#24965=EDGE_CURVE('',#20460,#20461,#10103,.T.);
#24966=EDGE_CURVE('',#20461,#20462,#10104,.T.);
#24967=EDGE_CURVE('',#20462,#20463,#10105,.T.);
#24968=EDGE_CURVE('',#20463,#20464,#10106,.T.);
#24969=EDGE_CURVE('',#20464,#20465,#10107,.T.);
#24970=EDGE_CURVE('',#20465,#20460,#10108,.T.);
#24971=EDGE_CURVE('',#20466,#20467,#10109,.T.);
#24972=EDGE_CURVE('',#20467,#20468,#10110,.T.);
#24973=EDGE_CURVE('',#20468,#20469,#10111,.T.);
#24974=EDGE_CURVE('',#20469,#20470,#10112,.T.);
#24975=EDGE_CURVE('',#20470,#20471,#10113,.T.);
#24976=EDGE_CURVE('',#20471,#20466,#10114,.T.);
#24977=EDGE_CURVE('',#20472,#20473,#10115,.T.);
#24978=EDGE_CURVE('',#20473,#20474,#10116,.T.);
#24979=EDGE_CURVE('',#20474,#20475,#10117,.T.);
#24980=EDGE_CURVE('',#20475,#20476,#10118,.T.);
#24981=EDGE_CURVE('',#20476,#20477,#10119,.T.);
#24982=EDGE_CURVE('',#20477,#20472,#10120,.T.);
#24983=EDGE_CURVE('',#20478,#20479,#10121,.T.);
#24984=EDGE_CURVE('',#20479,#20480,#10122,.T.);
#24985=EDGE_CURVE('',#20480,#20481,#10123,.T.);
#24986=EDGE_CURVE('',#20481,#20482,#10124,.T.);
#24987=EDGE_CURVE('',#20482,#20483,#10125,.T.);
#24988=EDGE_CURVE('',#20483,#20478,#10126,.T.);
#24989=EDGE_CURVE('',#20484,#20485,#10127,.T.);
#24990=EDGE_CURVE('',#20485,#20486,#10128,.T.);
#24991=EDGE_CURVE('',#20486,#20487,#10129,.T.);
#24992=EDGE_CURVE('',#20487,#20488,#10130,.T.);
#24993=EDGE_CURVE('',#20488,#20489,#10131,.T.);
#24994=EDGE_CURVE('',#20489,#20484,#10132,.T.);
#24995=EDGE_CURVE('',#20490,#20491,#10133,.T.);
#24996=EDGE_CURVE('',#20491,#20492,#10134,.T.);
#24997=EDGE_CURVE('',#20492,#20493,#10135,.T.);
#24998=EDGE_CURVE('',#20493,#20494,#10136,.T.);
#24999=EDGE_CURVE('',#20494,#20495,#10137,.T.);
#25000=EDGE_CURVE('',#20495,#20490,#10138,.T.);
#25001=EDGE_CURVE('',#20496,#20497,#10139,.T.);
#25002=EDGE_CURVE('',#20497,#20498,#10140,.T.);
#25003=EDGE_CURVE('',#20498,#20499,#10141,.T.);
#25004=EDGE_CURVE('',#20499,#20500,#10142,.T.);
#25005=EDGE_CURVE('',#20500,#20501,#10143,.T.);
#25006=EDGE_CURVE('',#20501,#20496,#10144,.T.);
#25007=EDGE_CURVE('',#20502,#20503,#10145,.T.);
#25008=EDGE_CURVE('',#20503,#20504,#10146,.T.);
#25009=EDGE_CURVE('',#20504,#20505,#10147,.T.);
#25010=EDGE_CURVE('',#20505,#20506,#10148,.T.);
#25011=EDGE_CURVE('',#20506,#20507,#10149,.T.);
#25012=EDGE_CURVE('',#20507,#20502,#10150,.T.);
#25013=EDGE_CURVE('',#20508,#20509,#10151,.T.);
#25014=EDGE_CURVE('',#20509,#20510,#10152,.T.);
#25015=EDGE_CURVE('',#20510,#20511,#10153,.T.);
#25016=EDGE_CURVE('',#20511,#20512,#10154,.T.);
#25017=EDGE_CURVE('',#20512,#20513,#10155,.T.);
#25018=EDGE_CURVE('',#20513,#20508,#10156,.T.);
#25019=EDGE_CURVE('',#20514,#20515,#10157,.T.);
#25020=EDGE_CURVE('',#20515,#20516,#10158,.T.);
#25021=EDGE_CURVE('',#20516,#20517,#10159,.T.);
#25022=EDGE_CURVE('',#20517,#20518,#10160,.T.);
#25023=EDGE_CURVE('',#20518,#20519,#10161,.T.);
#25024=EDGE_CURVE('',#20519,#20514,#10162,.T.);
#25025=EDGE_CURVE('',#20520,#20521,#10163,.T.);
#25026=EDGE_CURVE('',#20521,#20522,#10164,.T.);
#25027=EDGE_CURVE('',#20522,#20523,#10165,.T.);
#25028=EDGE_CURVE('',#20523,#20524,#10166,.T.);
#25029=EDGE_CURVE('',#20524,#20525,#10167,.T.);
#25030=EDGE_CURVE('',#20525,#20520,#10168,.T.);
#25031=EDGE_CURVE('',#20526,#20527,#10169,.T.);
#25032=EDGE_CURVE('',#20527,#20528,#10170,.T.);
#25033=EDGE_CURVE('',#20528,#20529,#10171,.T.);
#25034=EDGE_CURVE('',#20529,#20530,#10172,.T.);
#25035=EDGE_CURVE('',#20530,#20531,#10173,.T.);
#25036=EDGE_CURVE('',#20531,#20526,#10174,.T.);
#25037=EDGE_CURVE('',#20532,#20533,#10175,.T.);
#25038=EDGE_CURVE('',#20533,#20534,#10176,.T.);
#25039=EDGE_CURVE('',#20534,#20535,#10177,.T.);
#25040=EDGE_CURVE('',#20535,#20536,#10178,.T.);
#25041=EDGE_CURVE('',#20536,#20537,#10179,.T.);
#25042=EDGE_CURVE('',#20537,#20532,#10180,.T.);
#25043=EDGE_CURVE('',#20538,#20539,#10181,.T.);
#25044=EDGE_CURVE('',#20539,#20540,#10182,.T.);
#25045=EDGE_CURVE('',#20540,#20541,#10183,.T.);
#25046=EDGE_CURVE('',#20541,#20542,#10184,.T.);
#25047=EDGE_CURVE('',#20542,#20543,#10185,.T.);
#25048=EDGE_CURVE('',#20543,#20538,#10186,.T.);
#25049=EDGE_CURVE('',#20544,#20545,#10187,.T.);
#25050=EDGE_CURVE('',#20545,#20546,#10188,.T.);
#25051=EDGE_CURVE('',#20546,#20547,#10189,.T.);
#25052=EDGE_CURVE('',#20547,#20548,#10190,.T.);
#25053=EDGE_CURVE('',#20548,#20549,#10191,.T.);
#25054=EDGE_CURVE('',#20549,#20544,#10192,.T.);
#25055=EDGE_CURVE('',#20550,#20551,#10193,.T.);
#25056=EDGE_CURVE('',#20551,#20552,#10194,.T.);
#25057=EDGE_CURVE('',#20552,#20553,#10195,.T.);
#25058=EDGE_CURVE('',#20553,#20554,#10196,.T.);
#25059=EDGE_CURVE('',#20554,#20555,#10197,.T.);
#25060=EDGE_CURVE('',#20555,#20550,#10198,.T.);
#25061=EDGE_CURVE('',#20556,#20557,#10199,.T.);
#25062=EDGE_CURVE('',#20557,#20558,#10200,.T.);
#25063=EDGE_CURVE('',#20558,#20559,#10201,.T.);
#25064=EDGE_CURVE('',#20559,#20560,#10202,.T.);
#25065=EDGE_CURVE('',#20560,#20561,#10203,.T.);
#25066=EDGE_CURVE('',#20561,#20556,#10204,.T.);
#25067=EDGE_CURVE('',#20562,#20563,#10205,.T.);
#25068=EDGE_CURVE('',#20563,#20564,#10206,.T.);
#25069=EDGE_CURVE('',#20564,#20565,#10207,.T.);
#25070=EDGE_CURVE('',#20565,#20566,#10208,.T.);
#25071=EDGE_CURVE('',#20566,#20567,#10209,.T.);
#25072=EDGE_CURVE('',#20567,#20562,#10210,.T.);
#25073=EDGE_CURVE('',#20568,#20569,#10211,.T.);
#25074=EDGE_CURVE('',#20569,#20570,#10212,.T.);
#25075=EDGE_CURVE('',#20570,#20571,#10213,.T.);
#25076=EDGE_CURVE('',#20571,#20572,#10214,.T.);
#25077=EDGE_CURVE('',#20572,#20573,#10215,.T.);
#25078=EDGE_CURVE('',#20573,#20568,#10216,.T.);
#25079=EDGE_CURVE('',#20574,#20575,#10217,.T.);
#25080=EDGE_CURVE('',#20575,#20576,#10218,.T.);
#25081=EDGE_CURVE('',#20576,#20577,#10219,.T.);
#25082=EDGE_CURVE('',#20577,#20578,#10220,.T.);
#25083=EDGE_CURVE('',#20578,#20579,#10221,.T.);
#25084=EDGE_CURVE('',#20579,#20574,#10222,.T.);
#25085=EDGE_CURVE('',#20580,#20581,#10223,.T.);
#25086=EDGE_CURVE('',#20581,#20582,#10224,.T.);
#25087=EDGE_CURVE('',#20582,#20583,#10225,.T.);
#25088=EDGE_CURVE('',#20583,#20584,#10226,.T.);
#25089=EDGE_CURVE('',#20584,#20585,#10227,.T.);
#25090=EDGE_CURVE('',#20585,#20580,#10228,.T.);
#25091=EDGE_CURVE('',#20586,#20587,#10229,.T.);
#25092=EDGE_CURVE('',#20587,#20588,#10230,.T.);
#25093=EDGE_CURVE('',#20588,#20589,#10231,.T.);
#25094=EDGE_CURVE('',#20589,#20590,#10232,.T.);
#25095=EDGE_CURVE('',#20590,#20591,#10233,.T.);
#25096=EDGE_CURVE('',#20591,#20586,#10234,.T.);
#25097=EDGE_CURVE('',#20592,#20593,#10235,.T.);
#25098=EDGE_CURVE('',#20593,#20594,#10236,.T.);
#25099=EDGE_CURVE('',#20594,#20595,#10237,.T.);
#25100=EDGE_CURVE('',#20595,#20596,#10238,.T.);
#25101=EDGE_CURVE('',#20596,#20597,#10239,.T.);
#25102=EDGE_CURVE('',#20597,#20592,#10240,.T.);
#25103=EDGE_CURVE('',#20598,#20599,#10241,.T.);
#25104=EDGE_CURVE('',#20599,#20600,#10242,.T.);
#25105=EDGE_CURVE('',#20600,#20601,#10243,.T.);
#25106=EDGE_CURVE('',#20601,#20602,#10244,.T.);
#25107=EDGE_CURVE('',#20602,#20603,#10245,.T.);
#25108=EDGE_CURVE('',#20603,#20598,#10246,.T.);
#25109=EDGE_CURVE('',#20604,#20605,#10247,.T.);
#25110=EDGE_CURVE('',#20605,#20606,#10248,.T.);
#25111=EDGE_CURVE('',#20606,#20607,#10249,.T.);
#25112=EDGE_CURVE('',#20607,#20608,#10250,.T.);
#25113=EDGE_CURVE('',#20608,#20609,#10251,.T.);
#25114=EDGE_CURVE('',#20609,#20604,#10252,.T.);
#25115=EDGE_CURVE('',#20610,#20611,#10253,.T.);
#25116=EDGE_CURVE('',#20611,#20612,#10254,.T.);
#25117=EDGE_CURVE('',#20612,#20613,#10255,.T.);
#25118=EDGE_CURVE('',#20613,#20614,#10256,.T.);
#25119=EDGE_CURVE('',#20614,#20615,#10257,.T.);
#25120=EDGE_CURVE('',#20615,#20610,#10258,.T.);
#25121=EDGE_CURVE('',#20616,#20617,#10259,.T.);
#25122=EDGE_CURVE('',#20617,#20618,#10260,.T.);
#25123=EDGE_CURVE('',#20618,#20619,#10261,.T.);
#25124=EDGE_CURVE('',#20619,#20620,#10262,.T.);
#25125=EDGE_CURVE('',#20620,#20621,#10263,.T.);
#25126=EDGE_CURVE('',#20621,#20616,#10264,.T.);
#25127=EDGE_CURVE('',#20622,#20623,#10265,.T.);
#25128=EDGE_CURVE('',#20623,#20624,#10266,.T.);
#25129=EDGE_CURVE('',#20624,#20625,#10267,.T.);
#25130=EDGE_CURVE('',#20625,#20626,#10268,.T.);
#25131=EDGE_CURVE('',#20626,#20627,#10269,.T.);
#25132=EDGE_CURVE('',#20627,#20622,#10270,.T.);
#25133=EDGE_CURVE('',#20628,#20629,#10271,.T.);
#25134=EDGE_CURVE('',#20629,#20630,#10272,.T.);
#25135=EDGE_CURVE('',#20630,#20631,#10273,.T.);
#25136=EDGE_CURVE('',#20631,#20632,#10274,.T.);
#25137=EDGE_CURVE('',#20632,#20633,#10275,.T.);
#25138=EDGE_CURVE('',#20633,#20628,#10276,.T.);
#25139=EDGE_CURVE('',#20634,#20635,#10277,.T.);
#25140=EDGE_CURVE('',#20635,#20636,#10278,.T.);
#25141=EDGE_CURVE('',#20636,#20637,#10279,.T.);
#25142=EDGE_CURVE('',#20637,#20638,#10280,.T.);
#25143=EDGE_CURVE('',#20638,#20639,#10281,.T.);
#25144=EDGE_CURVE('',#20639,#20634,#10282,.T.);
#25145=EDGE_CURVE('',#20640,#20641,#10283,.T.);
#25146=EDGE_CURVE('',#20641,#20642,#10284,.T.);
#25147=EDGE_CURVE('',#20642,#20643,#10285,.T.);
#25148=EDGE_CURVE('',#20643,#20644,#10286,.T.);
#25149=EDGE_CURVE('',#20644,#20645,#10287,.T.);
#25150=EDGE_CURVE('',#20645,#20640,#10288,.T.);
#25151=EDGE_CURVE('',#20646,#20647,#10289,.T.);
#25152=EDGE_CURVE('',#20647,#20648,#10290,.T.);
#25153=EDGE_CURVE('',#20648,#20649,#10291,.T.);
#25154=EDGE_CURVE('',#20649,#20650,#10292,.T.);
#25155=EDGE_CURVE('',#20650,#20651,#10293,.T.);
#25156=EDGE_CURVE('',#20651,#20646,#10294,.T.);
#25157=EDGE_CURVE('',#20652,#20653,#10295,.T.);
#25158=EDGE_CURVE('',#20653,#20654,#10296,.T.);
#25159=EDGE_CURVE('',#20654,#20655,#10297,.T.);
#25160=EDGE_CURVE('',#20655,#20656,#10298,.T.);
#25161=EDGE_CURVE('',#20656,#20657,#10299,.T.);
#25162=EDGE_CURVE('',#20657,#20652,#10300,.T.);
#25163=EDGE_CURVE('',#20658,#20659,#10301,.T.);
#25164=EDGE_CURVE('',#20659,#20660,#10302,.T.);
#25165=EDGE_CURVE('',#20660,#20661,#10303,.T.);
#25166=EDGE_CURVE('',#20661,#20662,#10304,.T.);
#25167=EDGE_CURVE('',#20662,#20663,#10305,.T.);
#25168=EDGE_CURVE('',#20663,#20658,#10306,.T.);
#25169=EDGE_CURVE('',#20664,#20665,#10307,.T.);
#25170=EDGE_CURVE('',#20665,#20666,#10308,.T.);
#25171=EDGE_CURVE('',#20666,#20667,#10309,.T.);
#25172=EDGE_CURVE('',#20667,#20668,#10310,.T.);
#25173=EDGE_CURVE('',#20668,#20669,#10311,.T.);
#25174=EDGE_CURVE('',#20669,#20664,#10312,.T.);
#25175=EDGE_CURVE('',#20670,#20671,#10313,.T.);
#25176=EDGE_CURVE('',#20671,#20672,#10314,.T.);
#25177=EDGE_CURVE('',#20672,#20673,#10315,.T.);
#25178=EDGE_CURVE('',#20673,#20674,#10316,.T.);
#25179=EDGE_CURVE('',#20674,#20675,#10317,.T.);
#25180=EDGE_CURVE('',#20675,#20670,#10318,.T.);
#25181=EDGE_CURVE('',#20676,#20677,#10319,.T.);
#25182=EDGE_CURVE('',#20677,#20678,#10320,.T.);
#25183=EDGE_CURVE('',#20678,#20679,#10321,.T.);
#25184=EDGE_CURVE('',#20679,#20680,#10322,.T.);
#25185=EDGE_CURVE('',#20680,#20681,#10323,.T.);
#25186=EDGE_CURVE('',#20681,#20676,#10324,.T.);
#25187=EDGE_CURVE('',#20682,#20683,#10325,.T.);
#25188=EDGE_CURVE('',#20683,#20684,#10326,.T.);
#25189=EDGE_CURVE('',#20684,#20685,#10327,.T.);
#25190=EDGE_CURVE('',#20685,#20686,#10328,.T.);
#25191=EDGE_CURVE('',#20686,#20687,#10329,.T.);
#25192=EDGE_CURVE('',#20687,#20682,#10330,.T.);
#25193=EDGE_CURVE('',#20688,#20689,#10331,.T.);
#25194=EDGE_CURVE('',#20689,#20690,#10332,.T.);
#25195=EDGE_CURVE('',#20690,#20691,#10333,.T.);
#25196=EDGE_CURVE('',#20691,#20692,#10334,.T.);
#25197=EDGE_CURVE('',#20692,#20693,#10335,.T.);
#25198=EDGE_CURVE('',#20693,#20688,#10336,.T.);
#25199=EDGE_CURVE('',#20694,#20695,#10337,.T.);
#25200=EDGE_CURVE('',#20695,#20696,#10338,.T.);
#25201=EDGE_CURVE('',#20696,#20697,#10339,.T.);
#25202=EDGE_CURVE('',#20697,#20698,#10340,.T.);
#25203=EDGE_CURVE('',#20698,#20699,#10341,.T.);
#25204=EDGE_CURVE('',#20699,#20694,#10342,.T.);
#25205=EDGE_CURVE('',#20700,#20701,#10343,.T.);
#25206=EDGE_CURVE('',#20701,#20702,#10344,.T.);
#25207=EDGE_CURVE('',#20702,#20703,#10345,.T.);
#25208=EDGE_CURVE('',#20703,#20704,#10346,.T.);
#25209=EDGE_CURVE('',#20704,#20705,#10347,.T.);
#25210=EDGE_CURVE('',#20705,#20700,#10348,.T.);
#25211=EDGE_CURVE('',#20706,#20707,#10349,.T.);
#25212=EDGE_CURVE('',#20707,#20708,#10350,.T.);
#25213=EDGE_CURVE('',#20708,#20709,#10351,.T.);
#25214=EDGE_CURVE('',#20709,#20710,#10352,.T.);
#25215=EDGE_CURVE('',#20710,#20711,#10353,.T.);
#25216=EDGE_CURVE('',#20711,#20706,#10354,.T.);
#25217=EDGE_CURVE('',#20712,#20713,#10355,.T.);
#25218=EDGE_CURVE('',#20713,#20714,#10356,.T.);
#25219=EDGE_CURVE('',#20714,#20715,#10357,.T.);
#25220=EDGE_CURVE('',#20715,#20716,#10358,.T.);
#25221=EDGE_CURVE('',#20716,#20717,#10359,.T.);
#25222=EDGE_CURVE('',#20717,#20712,#10360,.T.);
#25223=EDGE_CURVE('',#20718,#20719,#10361,.T.);
#25224=EDGE_CURVE('',#20719,#20720,#10362,.T.);
#25225=EDGE_CURVE('',#20720,#20721,#10363,.T.);
#25226=EDGE_CURVE('',#20721,#20722,#10364,.T.);
#25227=EDGE_CURVE('',#20722,#20723,#10365,.T.);
#25228=EDGE_CURVE('',#20723,#20718,#10366,.T.);
#25229=EDGE_CURVE('',#20724,#20725,#10367,.T.);
#25230=EDGE_CURVE('',#20725,#20726,#10368,.T.);
#25231=EDGE_CURVE('',#20726,#20727,#10369,.T.);
#25232=EDGE_CURVE('',#20727,#20728,#10370,.T.);
#25233=EDGE_CURVE('',#20728,#20729,#10371,.T.);
#25234=EDGE_CURVE('',#20729,#20724,#10372,.T.);
#25235=EDGE_CURVE('',#20730,#20731,#10373,.T.);
#25236=EDGE_CURVE('',#20731,#20732,#10374,.T.);
#25237=EDGE_CURVE('',#20732,#20733,#10375,.T.);
#25238=EDGE_CURVE('',#20733,#20734,#10376,.T.);
#25239=EDGE_CURVE('',#20734,#20735,#10377,.T.);
#25240=EDGE_CURVE('',#20735,#20730,#10378,.T.);
#25241=EDGE_CURVE('',#20736,#20737,#10379,.T.);
#25242=EDGE_CURVE('',#20737,#20738,#10380,.T.);
#25243=EDGE_CURVE('',#20738,#20739,#10381,.T.);
#25244=EDGE_CURVE('',#20739,#20740,#10382,.T.);
#25245=EDGE_CURVE('',#20740,#20741,#10383,.T.);
#25246=EDGE_CURVE('',#20741,#20736,#10384,.T.);
#25247=EDGE_CURVE('',#20742,#20743,#10385,.T.);
#25248=EDGE_CURVE('',#20743,#20744,#10386,.T.);
#25249=EDGE_CURVE('',#20744,#20745,#10387,.T.);
#25250=EDGE_CURVE('',#20745,#20746,#10388,.T.);
#25251=EDGE_CURVE('',#20746,#20747,#10389,.T.);
#25252=EDGE_CURVE('',#20747,#20742,#10390,.T.);
#25253=EDGE_CURVE('',#20748,#20749,#10391,.T.);
#25254=EDGE_CURVE('',#20749,#20750,#10392,.T.);
#25255=EDGE_CURVE('',#20750,#20751,#10393,.T.);
#25256=EDGE_CURVE('',#20751,#20752,#10394,.T.);
#25257=EDGE_CURVE('',#20752,#20753,#10395,.T.);
#25258=EDGE_CURVE('',#20753,#20748,#10396,.T.);
#25259=EDGE_CURVE('',#20754,#20755,#10397,.T.);
#25260=EDGE_CURVE('',#20755,#20756,#10398,.T.);
#25261=EDGE_CURVE('',#20756,#20757,#10399,.T.);
#25262=EDGE_CURVE('',#20757,#20758,#10400,.T.);
#25263=EDGE_CURVE('',#20758,#20759,#10401,.T.);
#25264=EDGE_CURVE('',#20759,#20754,#10402,.T.);
#25265=EDGE_CURVE('',#20760,#20761,#10403,.T.);
#25266=EDGE_CURVE('',#20761,#20762,#10404,.T.);
#25267=EDGE_CURVE('',#20762,#20763,#10405,.T.);
#25268=EDGE_CURVE('',#20763,#20764,#10406,.T.);
#25269=EDGE_CURVE('',#20764,#20765,#10407,.T.);
#25270=EDGE_CURVE('',#20765,#20760,#10408,.T.);
#25271=EDGE_CURVE('',#20766,#20767,#10409,.T.);
#25272=EDGE_CURVE('',#20767,#20768,#10410,.T.);
#25273=EDGE_CURVE('',#20768,#20769,#10411,.T.);
#25274=EDGE_CURVE('',#20769,#20770,#10412,.T.);
#25275=EDGE_CURVE('',#20770,#20771,#10413,.T.);
#25276=EDGE_CURVE('',#20771,#20766,#10414,.T.);
#25277=EDGE_CURVE('',#20772,#20773,#10415,.T.);
#25278=EDGE_CURVE('',#20773,#20774,#10416,.T.);
#25279=EDGE_CURVE('',#20774,#20775,#10417,.T.);
#25280=EDGE_CURVE('',#20775,#20776,#10418,.T.);
#25281=EDGE_CURVE('',#20776,#20777,#10419,.T.);
#25282=EDGE_CURVE('',#20777,#20772,#10420,.T.);
#25283=EDGE_CURVE('',#20778,#20779,#10421,.T.);
#25284=EDGE_CURVE('',#20779,#20780,#10422,.T.);
#25285=EDGE_CURVE('',#20780,#20781,#10423,.T.);
#25286=EDGE_CURVE('',#20781,#20782,#10424,.T.);
#25287=EDGE_CURVE('',#20782,#20783,#10425,.T.);
#25288=EDGE_CURVE('',#20783,#20778,#10426,.T.);
#25289=EDGE_CURVE('',#20784,#20785,#10427,.T.);
#25290=EDGE_CURVE('',#20785,#20786,#10428,.T.);
#25291=EDGE_CURVE('',#20786,#20787,#10429,.T.);
#25292=EDGE_CURVE('',#20787,#20788,#10430,.T.);
#25293=EDGE_CURVE('',#20788,#20789,#10431,.T.);
#25294=EDGE_CURVE('',#20789,#20784,#10432,.T.);
#25295=EDGE_CURVE('',#20790,#20791,#10433,.T.);
#25296=EDGE_CURVE('',#20791,#20792,#10434,.T.);
#25297=EDGE_CURVE('',#20792,#20793,#10435,.T.);
#25298=EDGE_CURVE('',#20793,#20794,#10436,.T.);
#25299=EDGE_CURVE('',#20794,#20795,#10437,.T.);
#25300=EDGE_CURVE('',#20795,#20790,#10438,.T.);
#25301=EDGE_CURVE('',#20796,#20797,#10439,.T.);
#25302=EDGE_CURVE('',#20797,#20798,#10440,.T.);
#25303=EDGE_CURVE('',#20798,#20799,#10441,.T.);
#25304=EDGE_CURVE('',#20799,#20800,#10442,.T.);
#25305=EDGE_CURVE('',#20800,#20801,#10443,.T.);
#25306=EDGE_CURVE('',#20801,#20796,#10444,.T.);
#25307=EDGE_CURVE('',#20802,#20803,#10445,.T.);
#25308=EDGE_CURVE('',#20803,#20804,#10446,.T.);
#25309=EDGE_CURVE('',#20804,#20805,#10447,.T.);
#25310=EDGE_CURVE('',#20805,#20806,#10448,.T.);
#25311=EDGE_CURVE('',#20806,#20807,#10449,.T.);
#25312=EDGE_CURVE('',#20807,#20802,#10450,.T.);
#25313=EDGE_CURVE('',#20808,#20809,#10451,.T.);
#25314=EDGE_CURVE('',#20809,#20810,#10452,.T.);
#25315=EDGE_CURVE('',#20810,#20811,#10453,.T.);
#25316=EDGE_CURVE('',#20811,#20812,#10454,.T.);
#25317=EDGE_CURVE('',#20812,#20813,#10455,.T.);
#25318=EDGE_CURVE('',#20813,#20808,#10456,.T.);
#25319=EDGE_CURVE('',#20814,#20815,#10457,.T.);
#25320=EDGE_CURVE('',#20815,#20816,#10458,.T.);
#25321=EDGE_CURVE('',#20816,#20817,#10459,.T.);
#25322=EDGE_CURVE('',#20817,#20818,#10460,.T.);
#25323=EDGE_CURVE('',#20818,#20819,#10461,.T.);
#25324=EDGE_CURVE('',#20819,#20814,#10462,.T.);
#25325=EDGE_CURVE('',#20820,#20821,#10463,.T.);
#25326=EDGE_CURVE('',#20821,#20822,#10464,.T.);
#25327=EDGE_CURVE('',#20822,#20823,#10465,.T.);
#25328=EDGE_CURVE('',#20823,#20824,#10466,.T.);
#25329=EDGE_CURVE('',#20824,#20825,#10467,.T.);
#25330=EDGE_CURVE('',#20825,#20820,#10468,.T.);
#25331=EDGE_CURVE('',#20826,#20827,#10469,.T.);
#25332=EDGE_CURVE('',#20827,#20828,#10470,.T.);
#25333=EDGE_CURVE('',#20828,#20829,#10471,.T.);
#25334=EDGE_CURVE('',#20829,#20830,#10472,.T.);
#25335=EDGE_CURVE('',#20830,#20831,#10473,.T.);
#25336=EDGE_CURVE('',#20831,#20826,#10474,.T.);
#25337=EDGE_CURVE('',#20832,#20833,#10475,.T.);
#25338=EDGE_CURVE('',#20833,#20834,#10476,.T.);
#25339=EDGE_CURVE('',#20834,#20835,#10477,.T.);
#25340=EDGE_CURVE('',#20835,#20836,#10478,.T.);
#25341=EDGE_CURVE('',#20836,#20837,#10479,.T.);
#25342=EDGE_CURVE('',#20837,#20832,#10480,.T.);
#25343=EDGE_CURVE('',#20838,#20839,#10481,.T.);
#25344=EDGE_CURVE('',#20839,#20840,#10482,.T.);
#25345=EDGE_CURVE('',#20840,#20841,#10483,.T.);
#25346=EDGE_CURVE('',#20841,#20842,#10484,.T.);
#25347=EDGE_CURVE('',#20842,#20843,#10485,.T.);
#25348=EDGE_CURVE('',#20843,#20838,#10486,.T.);
#25349=EDGE_CURVE('',#20844,#20845,#10487,.T.);
#25350=EDGE_CURVE('',#20845,#20846,#10488,.T.);
#25351=EDGE_CURVE('',#20846,#20847,#10489,.T.);
#25352=EDGE_CURVE('',#20847,#20848,#10490,.T.);
#25353=EDGE_CURVE('',#20848,#20849,#10491,.T.);
#25354=EDGE_CURVE('',#20849,#20844,#10492,.T.);
#25355=EDGE_CURVE('',#20850,#20851,#10493,.T.);
#25356=EDGE_CURVE('',#20851,#20852,#10494,.T.);
#25357=EDGE_CURVE('',#20852,#20853,#10495,.T.);
#25358=EDGE_CURVE('',#20853,#20854,#10496,.T.);
#25359=EDGE_CURVE('',#20854,#20855,#10497,.T.);
#25360=EDGE_CURVE('',#20855,#20850,#10498,.T.);
#25361=EDGE_CURVE('',#20851,#19734,#10499,.T.);
#25362=EDGE_CURVE('',#20852,#19735,#10500,.T.);
#25363=EDGE_CURVE('',#20850,#19736,#10501,.T.);
#25364=EDGE_CURVE('',#20855,#19737,#10502,.T.);
#25365=EDGE_CURVE('',#20854,#19738,#10503,.T.);
#25366=EDGE_CURVE('',#20853,#19739,#10504,.T.);
#25367=EDGE_CURVE('',#20845,#19728,#10505,.T.);
#25368=EDGE_CURVE('',#20846,#19729,#10506,.T.);
#25369=EDGE_CURVE('',#20844,#19730,#10507,.T.);
#25370=EDGE_CURVE('',#20849,#19731,#10508,.T.);
#25371=EDGE_CURVE('',#20848,#19732,#10509,.T.);
#25372=EDGE_CURVE('',#20847,#19733,#10510,.T.);
#25373=EDGE_CURVE('',#20839,#19722,#10511,.T.);
#25374=EDGE_CURVE('',#20840,#19723,#10512,.T.);
#25375=EDGE_CURVE('',#20838,#19724,#10513,.T.);
#25376=EDGE_CURVE('',#20843,#19725,#10514,.T.);
#25377=EDGE_CURVE('',#20842,#19726,#10515,.T.);
#25378=EDGE_CURVE('',#20841,#19727,#10516,.T.);
#25379=EDGE_CURVE('',#20833,#19716,#10517,.T.);
#25380=EDGE_CURVE('',#20834,#19717,#10518,.T.);
#25381=EDGE_CURVE('',#20832,#19718,#10519,.T.);
#25382=EDGE_CURVE('',#20837,#19719,#10520,.T.);
#25383=EDGE_CURVE('',#20836,#19720,#10521,.T.);
#25384=EDGE_CURVE('',#20835,#19721,#10522,.T.);
#25385=EDGE_CURVE('',#20827,#19710,#10523,.T.);
#25386=EDGE_CURVE('',#20828,#19711,#10524,.T.);
#25387=EDGE_CURVE('',#20826,#19712,#10525,.T.);
#25388=EDGE_CURVE('',#20831,#19713,#10526,.T.);
#25389=EDGE_CURVE('',#20830,#19714,#10527,.T.);
#25390=EDGE_CURVE('',#20829,#19715,#10528,.T.);
#25391=EDGE_CURVE('',#20821,#19704,#10529,.T.);
#25392=EDGE_CURVE('',#20822,#19705,#10530,.T.);
#25393=EDGE_CURVE('',#20820,#19706,#10531,.T.);
#25394=EDGE_CURVE('',#20825,#19707,#10532,.T.);
#25395=EDGE_CURVE('',#20824,#19708,#10533,.T.);
#25396=EDGE_CURVE('',#20823,#19709,#10534,.T.);
#25397=EDGE_CURVE('',#20815,#19698,#10535,.T.);
#25398=EDGE_CURVE('',#20816,#19699,#10536,.T.);
#25399=EDGE_CURVE('',#20814,#19700,#10537,.T.);
#25400=EDGE_CURVE('',#20819,#19701,#10538,.T.);
#25401=EDGE_CURVE('',#20818,#19702,#10539,.T.);
#25402=EDGE_CURVE('',#20817,#19703,#10540,.T.);
#25403=EDGE_CURVE('',#20809,#19692,#10541,.T.);
#25404=EDGE_CURVE('',#20810,#19693,#10542,.T.);
#25405=EDGE_CURVE('',#20808,#19694,#10543,.T.);
#25406=EDGE_CURVE('',#20813,#19695,#10544,.T.);
#25407=EDGE_CURVE('',#20812,#19696,#10545,.T.);
#25408=EDGE_CURVE('',#20811,#19697,#10546,.T.);
#25409=EDGE_CURVE('',#20803,#19686,#10547,.T.);
#25410=EDGE_CURVE('',#20804,#19687,#10548,.T.);
#25411=EDGE_CURVE('',#20802,#19688,#10549,.T.);
#25412=EDGE_CURVE('',#20807,#19689,#10550,.T.);
#25413=EDGE_CURVE('',#20806,#19690,#10551,.T.);
#25414=EDGE_CURVE('',#20805,#19691,#10552,.T.);
#25415=EDGE_CURVE('',#20797,#19680,#10553,.T.);
#25416=EDGE_CURVE('',#20798,#19681,#10554,.T.);
#25417=EDGE_CURVE('',#20796,#19682,#10555,.T.);
#25418=EDGE_CURVE('',#20801,#19683,#10556,.T.);
#25419=EDGE_CURVE('',#20800,#19684,#10557,.T.);
#25420=EDGE_CURVE('',#20799,#19685,#10558,.T.);
#25421=EDGE_CURVE('',#20791,#19674,#10559,.T.);
#25422=EDGE_CURVE('',#20792,#19675,#10560,.T.);
#25423=EDGE_CURVE('',#20790,#19676,#10561,.T.);
#25424=EDGE_CURVE('',#20795,#19677,#10562,.T.);
#25425=EDGE_CURVE('',#20794,#19678,#10563,.T.);
#25426=EDGE_CURVE('',#20793,#19679,#10564,.T.);
#25427=EDGE_CURVE('',#20785,#19668,#10565,.T.);
#25428=EDGE_CURVE('',#20786,#19669,#10566,.T.);
#25429=EDGE_CURVE('',#20784,#19670,#10567,.T.);
#25430=EDGE_CURVE('',#20789,#19671,#10568,.T.);
#25431=EDGE_CURVE('',#20788,#19672,#10569,.T.);
#25432=EDGE_CURVE('',#20787,#19673,#10570,.T.);
#25433=EDGE_CURVE('',#20779,#19662,#10571,.T.);
#25434=EDGE_CURVE('',#20780,#19663,#10572,.T.);
#25435=EDGE_CURVE('',#20778,#19664,#10573,.T.);
#25436=EDGE_CURVE('',#20783,#19665,#10574,.T.);
#25437=EDGE_CURVE('',#20782,#19666,#10575,.T.);
#25438=EDGE_CURVE('',#20781,#19667,#10576,.T.);
#25439=EDGE_CURVE('',#20773,#19656,#10577,.T.);
#25440=EDGE_CURVE('',#20774,#19657,#10578,.T.);
#25441=EDGE_CURVE('',#20772,#19658,#10579,.T.);
#25442=EDGE_CURVE('',#20777,#19659,#10580,.T.);
#25443=EDGE_CURVE('',#20776,#19660,#10581,.T.);
#25444=EDGE_CURVE('',#20775,#19661,#10582,.T.);
#25445=EDGE_CURVE('',#20767,#19650,#10583,.T.);
#25446=EDGE_CURVE('',#20768,#19651,#10584,.T.);
#25447=EDGE_CURVE('',#20766,#19652,#10585,.T.);
#25448=EDGE_CURVE('',#20771,#19653,#10586,.T.);
#25449=EDGE_CURVE('',#20770,#19654,#10587,.T.);
#25450=EDGE_CURVE('',#20769,#19655,#10588,.T.);
#25451=EDGE_CURVE('',#20761,#19644,#10589,.T.);
#25452=EDGE_CURVE('',#20762,#19645,#10590,.T.);
#25453=EDGE_CURVE('',#20760,#19646,#10591,.T.);
#25454=EDGE_CURVE('',#20765,#19647,#10592,.T.);
#25455=EDGE_CURVE('',#20764,#19648,#10593,.T.);
#25456=EDGE_CURVE('',#20763,#19649,#10594,.T.);
#25457=EDGE_CURVE('',#20755,#19638,#10595,.T.);
#25458=EDGE_CURVE('',#20756,#19639,#10596,.T.);
#25459=EDGE_CURVE('',#20754,#19640,#10597,.T.);
#25460=EDGE_CURVE('',#20759,#19641,#10598,.T.);
#25461=EDGE_CURVE('',#20758,#19642,#10599,.T.);
#25462=EDGE_CURVE('',#20757,#19643,#10600,.T.);
#25463=EDGE_CURVE('',#20749,#19632,#10601,.T.);
#25464=EDGE_CURVE('',#20750,#19633,#10602,.T.);
#25465=EDGE_CURVE('',#20748,#19634,#10603,.T.);
#25466=EDGE_CURVE('',#20753,#19635,#10604,.T.);
#25467=EDGE_CURVE('',#20752,#19636,#10605,.T.);
#25468=EDGE_CURVE('',#20751,#19637,#10606,.T.);
#25469=EDGE_CURVE('',#20743,#19626,#10607,.T.);
#25470=EDGE_CURVE('',#20744,#19627,#10608,.T.);
#25471=EDGE_CURVE('',#20742,#19628,#10609,.T.);
#25472=EDGE_CURVE('',#20747,#19629,#10610,.T.);
#25473=EDGE_CURVE('',#20746,#19630,#10611,.T.);
#25474=EDGE_CURVE('',#20745,#19631,#10612,.T.);
#25475=EDGE_CURVE('',#20737,#19620,#10613,.T.);
#25476=EDGE_CURVE('',#20738,#19621,#10614,.T.);
#25477=EDGE_CURVE('',#20736,#19622,#10615,.T.);
#25478=EDGE_CURVE('',#20741,#19623,#10616,.T.);
#25479=EDGE_CURVE('',#20740,#19624,#10617,.T.);
#25480=EDGE_CURVE('',#20739,#19625,#10618,.T.);
#25481=EDGE_CURVE('',#20731,#19614,#10619,.T.);
#25482=EDGE_CURVE('',#20732,#19615,#10620,.T.);
#25483=EDGE_CURVE('',#20730,#19616,#10621,.T.);
#25484=EDGE_CURVE('',#20735,#19617,#10622,.T.);
#25485=EDGE_CURVE('',#20734,#19618,#10623,.T.);
#25486=EDGE_CURVE('',#20733,#19619,#10624,.T.);
#25487=EDGE_CURVE('',#20725,#19608,#10625,.T.);
#25488=EDGE_CURVE('',#20726,#19609,#10626,.T.);
#25489=EDGE_CURVE('',#20724,#19610,#10627,.T.);
#25490=EDGE_CURVE('',#20729,#19611,#10628,.T.);
#25491=EDGE_CURVE('',#20728,#19612,#10629,.T.);
#25492=EDGE_CURVE('',#20727,#19613,#10630,.T.);
#25493=EDGE_CURVE('',#20719,#19602,#10631,.T.);
#25494=EDGE_CURVE('',#20720,#19603,#10632,.T.);
#25495=EDGE_CURVE('',#20718,#19604,#10633,.T.);
#25496=EDGE_CURVE('',#20723,#19605,#10634,.T.);
#25497=EDGE_CURVE('',#20722,#19606,#10635,.T.);
#25498=EDGE_CURVE('',#20721,#19607,#10636,.T.);
#25499=EDGE_CURVE('',#20713,#19596,#10637,.T.);
#25500=EDGE_CURVE('',#20714,#19597,#10638,.T.);
#25501=EDGE_CURVE('',#20712,#19598,#10639,.T.);
#25502=EDGE_CURVE('',#20717,#19599,#10640,.T.);
#25503=EDGE_CURVE('',#20716,#19600,#10641,.T.);
#25504=EDGE_CURVE('',#20715,#19601,#10642,.T.);
#25505=EDGE_CURVE('',#20707,#19590,#10643,.T.);
#25506=EDGE_CURVE('',#20708,#19591,#10644,.T.);
#25507=EDGE_CURVE('',#20706,#19592,#10645,.T.);
#25508=EDGE_CURVE('',#20711,#19593,#10646,.T.);
#25509=EDGE_CURVE('',#20710,#19594,#10647,.T.);
#25510=EDGE_CURVE('',#20709,#19595,#10648,.T.);
#25511=EDGE_CURVE('',#20701,#19584,#10649,.T.);
#25512=EDGE_CURVE('',#20702,#19585,#10650,.T.);
#25513=EDGE_CURVE('',#20700,#19586,#10651,.T.);
#25514=EDGE_CURVE('',#20705,#19587,#10652,.T.);
#25515=EDGE_CURVE('',#20704,#19588,#10653,.T.);
#25516=EDGE_CURVE('',#20703,#19589,#10654,.T.);
#25517=EDGE_CURVE('',#20695,#19578,#10655,.T.);
#25518=EDGE_CURVE('',#20696,#19579,#10656,.T.);
#25519=EDGE_CURVE('',#20694,#19580,#10657,.T.);
#25520=EDGE_CURVE('',#20699,#19581,#10658,.T.);
#25521=EDGE_CURVE('',#20698,#19582,#10659,.T.);
#25522=EDGE_CURVE('',#20697,#19583,#10660,.T.);
#25523=EDGE_CURVE('',#20689,#19572,#10661,.T.);
#25524=EDGE_CURVE('',#20690,#19573,#10662,.T.);
#25525=EDGE_CURVE('',#20688,#19574,#10663,.T.);
#25526=EDGE_CURVE('',#20693,#19575,#10664,.T.);
#25527=EDGE_CURVE('',#20692,#19576,#10665,.T.);
#25528=EDGE_CURVE('',#20691,#19577,#10666,.T.);
#25529=EDGE_CURVE('',#20683,#19566,#10667,.T.);
#25530=EDGE_CURVE('',#20684,#19567,#10668,.T.);
#25531=EDGE_CURVE('',#20682,#19568,#10669,.T.);
#25532=EDGE_CURVE('',#20687,#19569,#10670,.T.);
#25533=EDGE_CURVE('',#20686,#19570,#10671,.T.);
#25534=EDGE_CURVE('',#20685,#19571,#10672,.T.);
#25535=EDGE_CURVE('',#20677,#19560,#10673,.T.);
#25536=EDGE_CURVE('',#20678,#19561,#10674,.T.);
#25537=EDGE_CURVE('',#20676,#19562,#10675,.T.);
#25538=EDGE_CURVE('',#20681,#19563,#10676,.T.);
#25539=EDGE_CURVE('',#20680,#19564,#10677,.T.);
#25540=EDGE_CURVE('',#20679,#19565,#10678,.T.);
#25541=EDGE_CURVE('',#20671,#19554,#10679,.T.);
#25542=EDGE_CURVE('',#20672,#19555,#10680,.T.);
#25543=EDGE_CURVE('',#20670,#19556,#10681,.T.);
#25544=EDGE_CURVE('',#20675,#19557,#10682,.T.);
#25545=EDGE_CURVE('',#20674,#19558,#10683,.T.);
#25546=EDGE_CURVE('',#20673,#19559,#10684,.T.);
#25547=EDGE_CURVE('',#20665,#19548,#10685,.T.);
#25548=EDGE_CURVE('',#20666,#19549,#10686,.T.);
#25549=EDGE_CURVE('',#20664,#19550,#10687,.T.);
#25550=EDGE_CURVE('',#20669,#19551,#10688,.T.);
#25551=EDGE_CURVE('',#20668,#19552,#10689,.T.);
#25552=EDGE_CURVE('',#20667,#19553,#10690,.T.);
#25553=EDGE_CURVE('',#20659,#19542,#10691,.T.);
#25554=EDGE_CURVE('',#20660,#19543,#10692,.T.);
#25555=EDGE_CURVE('',#20658,#19544,#10693,.T.);
#25556=EDGE_CURVE('',#20663,#19545,#10694,.T.);
#25557=EDGE_CURVE('',#20662,#19546,#10695,.T.);
#25558=EDGE_CURVE('',#20661,#19547,#10696,.T.);
#25559=EDGE_CURVE('',#20653,#19536,#10697,.T.);
#25560=EDGE_CURVE('',#20654,#19537,#10698,.T.);
#25561=EDGE_CURVE('',#20652,#19538,#10699,.T.);
#25562=EDGE_CURVE('',#20657,#19539,#10700,.T.);
#25563=EDGE_CURVE('',#20656,#19540,#10701,.T.);
#25564=EDGE_CURVE('',#20655,#19541,#10702,.T.);
#25565=EDGE_CURVE('',#20647,#19530,#10703,.T.);
#25566=EDGE_CURVE('',#20648,#19531,#10704,.T.);
#25567=EDGE_CURVE('',#20646,#19532,#10705,.T.);
#25568=EDGE_CURVE('',#20651,#19533,#10706,.T.);
#25569=EDGE_CURVE('',#20650,#19534,#10707,.T.);
#25570=EDGE_CURVE('',#20649,#19535,#10708,.T.);
#25571=EDGE_CURVE('',#20641,#19524,#10709,.T.);
#25572=EDGE_CURVE('',#20642,#19525,#10710,.T.);
#25573=EDGE_CURVE('',#20640,#19526,#10711,.T.);
#25574=EDGE_CURVE('',#20645,#19527,#10712,.T.);
#25575=EDGE_CURVE('',#20644,#19528,#10713,.T.);
#25576=EDGE_CURVE('',#20643,#19529,#10714,.T.);
#25577=EDGE_CURVE('',#20635,#19518,#10715,.T.);
#25578=EDGE_CURVE('',#20636,#19519,#10716,.T.);
#25579=EDGE_CURVE('',#20634,#19520,#10717,.T.);
#25580=EDGE_CURVE('',#20639,#19521,#10718,.T.);
#25581=EDGE_CURVE('',#20638,#19522,#10719,.T.);
#25582=EDGE_CURVE('',#20637,#19523,#10720,.T.);
#25583=EDGE_CURVE('',#20629,#19512,#10721,.T.);
#25584=EDGE_CURVE('',#20630,#19513,#10722,.T.);
#25585=EDGE_CURVE('',#20628,#19514,#10723,.T.);
#25586=EDGE_CURVE('',#20633,#19515,#10724,.T.);
#25587=EDGE_CURVE('',#20632,#19516,#10725,.T.);
#25588=EDGE_CURVE('',#20631,#19517,#10726,.T.);
#25589=EDGE_CURVE('',#20623,#19506,#10727,.T.);
#25590=EDGE_CURVE('',#20624,#19507,#10728,.T.);
#25591=EDGE_CURVE('',#20622,#19508,#10729,.T.);
#25592=EDGE_CURVE('',#20627,#19509,#10730,.T.);
#25593=EDGE_CURVE('',#20626,#19510,#10731,.T.);
#25594=EDGE_CURVE('',#20625,#19511,#10732,.T.);
#25595=EDGE_CURVE('',#20617,#19500,#10733,.T.);
#25596=EDGE_CURVE('',#20618,#19501,#10734,.T.);
#25597=EDGE_CURVE('',#20616,#19502,#10735,.T.);
#25598=EDGE_CURVE('',#20621,#19503,#10736,.T.);
#25599=EDGE_CURVE('',#20620,#19504,#10737,.T.);
#25600=EDGE_CURVE('',#20619,#19505,#10738,.T.);
#25601=EDGE_CURVE('',#20611,#19494,#10739,.T.);
#25602=EDGE_CURVE('',#20612,#19495,#10740,.T.);
#25603=EDGE_CURVE('',#20610,#19496,#10741,.T.);
#25604=EDGE_CURVE('',#20615,#19497,#10742,.T.);
#25605=EDGE_CURVE('',#20614,#19498,#10743,.T.);
#25606=EDGE_CURVE('',#20613,#19499,#10744,.T.);
#25607=EDGE_CURVE('',#20605,#19488,#10745,.T.);
#25608=EDGE_CURVE('',#20606,#19489,#10746,.T.);
#25609=EDGE_CURVE('',#20604,#19490,#10747,.T.);
#25610=EDGE_CURVE('',#20609,#19491,#10748,.T.);
#25611=EDGE_CURVE('',#20608,#19492,#10749,.T.);
#25612=EDGE_CURVE('',#20607,#19493,#10750,.T.);
#25613=EDGE_CURVE('',#20599,#19482,#10751,.T.);
#25614=EDGE_CURVE('',#20600,#19483,#10752,.T.);
#25615=EDGE_CURVE('',#20598,#19484,#10753,.T.);
#25616=EDGE_CURVE('',#20603,#19485,#10754,.T.);
#25617=EDGE_CURVE('',#20602,#19486,#10755,.T.);
#25618=EDGE_CURVE('',#20601,#19487,#10756,.T.);
#25619=EDGE_CURVE('',#20593,#19476,#10757,.T.);
#25620=EDGE_CURVE('',#20594,#19477,#10758,.T.);
#25621=EDGE_CURVE('',#20592,#19478,#10759,.T.);
#25622=EDGE_CURVE('',#20597,#19479,#10760,.T.);
#25623=EDGE_CURVE('',#20596,#19480,#10761,.T.);
#25624=EDGE_CURVE('',#20595,#19481,#10762,.T.);
#25625=EDGE_CURVE('',#20587,#19470,#10763,.T.);
#25626=EDGE_CURVE('',#20588,#19471,#10764,.T.);
#25627=EDGE_CURVE('',#20586,#19472,#10765,.T.);
#25628=EDGE_CURVE('',#20591,#19473,#10766,.T.);
#25629=EDGE_CURVE('',#20590,#19474,#10767,.T.);
#25630=EDGE_CURVE('',#20589,#19475,#10768,.T.);
#25631=EDGE_CURVE('',#20581,#19464,#10769,.T.);
#25632=EDGE_CURVE('',#20582,#19465,#10770,.T.);
#25633=EDGE_CURVE('',#20580,#19466,#10771,.T.);
#25634=EDGE_CURVE('',#20585,#19467,#10772,.T.);
#25635=EDGE_CURVE('',#20584,#19468,#10773,.T.);
#25636=EDGE_CURVE('',#20583,#19469,#10774,.T.);
#25637=EDGE_CURVE('',#20575,#19458,#10775,.T.);
#25638=EDGE_CURVE('',#20576,#19459,#10776,.T.);
#25639=EDGE_CURVE('',#20574,#19460,#10777,.T.);
#25640=EDGE_CURVE('',#20579,#19461,#10778,.T.);
#25641=EDGE_CURVE('',#20578,#19462,#10779,.T.);
#25642=EDGE_CURVE('',#20577,#19463,#10780,.T.);
#25643=EDGE_CURVE('',#20569,#19452,#10781,.T.);
#25644=EDGE_CURVE('',#20570,#19453,#10782,.T.);
#25645=EDGE_CURVE('',#20568,#19454,#10783,.T.);
#25646=EDGE_CURVE('',#20573,#19455,#10784,.T.);
#25647=EDGE_CURVE('',#20572,#19456,#10785,.T.);
#25648=EDGE_CURVE('',#20571,#19457,#10786,.T.);
#25649=EDGE_CURVE('',#20563,#19446,#10787,.T.);
#25650=EDGE_CURVE('',#20564,#19447,#10788,.T.);
#25651=EDGE_CURVE('',#20562,#19448,#10789,.T.);
#25652=EDGE_CURVE('',#20567,#19449,#10790,.T.);
#25653=EDGE_CURVE('',#20566,#19450,#10791,.T.);
#25654=EDGE_CURVE('',#20565,#19451,#10792,.T.);
#25655=EDGE_CURVE('',#20557,#19440,#10793,.T.);
#25656=EDGE_CURVE('',#20558,#19441,#10794,.T.);
#25657=EDGE_CURVE('',#20556,#19442,#10795,.T.);
#25658=EDGE_CURVE('',#20561,#19443,#10796,.T.);
#25659=EDGE_CURVE('',#20560,#19444,#10797,.T.);
#25660=EDGE_CURVE('',#20559,#19445,#10798,.T.);
#25661=EDGE_CURVE('',#20551,#19434,#10799,.T.);
#25662=EDGE_CURVE('',#20552,#19435,#10800,.T.);
#25663=EDGE_CURVE('',#20550,#19436,#10801,.T.);
#25664=EDGE_CURVE('',#20555,#19437,#10802,.T.);
#25665=EDGE_CURVE('',#20554,#19438,#10803,.T.);
#25666=EDGE_CURVE('',#20553,#19439,#10804,.T.);
#25667=EDGE_CURVE('',#20545,#19428,#10805,.T.);
#25668=EDGE_CURVE('',#20546,#19429,#10806,.T.);
#25669=EDGE_CURVE('',#20544,#19430,#10807,.T.);
#25670=EDGE_CURVE('',#20549,#19431,#10808,.T.);
#25671=EDGE_CURVE('',#20548,#19432,#10809,.T.);
#25672=EDGE_CURVE('',#20547,#19433,#10810,.T.);
#25673=EDGE_CURVE('',#20539,#19422,#10811,.T.);
#25674=EDGE_CURVE('',#20540,#19423,#10812,.T.);
#25675=EDGE_CURVE('',#20538,#19424,#10813,.T.);
#25676=EDGE_CURVE('',#20543,#19425,#10814,.T.);
#25677=EDGE_CURVE('',#20542,#19426,#10815,.T.);
#25678=EDGE_CURVE('',#20541,#19427,#10816,.T.);
#25679=EDGE_CURVE('',#20533,#19416,#10817,.T.);
#25680=EDGE_CURVE('',#20534,#19417,#10818,.T.);
#25681=EDGE_CURVE('',#20532,#19418,#10819,.T.);
#25682=EDGE_CURVE('',#20537,#19419,#10820,.T.);
#25683=EDGE_CURVE('',#20536,#19420,#10821,.T.);
#25684=EDGE_CURVE('',#20535,#19421,#10822,.T.);
#25685=EDGE_CURVE('',#20527,#19410,#10823,.T.);
#25686=EDGE_CURVE('',#20528,#19411,#10824,.T.);
#25687=EDGE_CURVE('',#20526,#19412,#10825,.T.);
#25688=EDGE_CURVE('',#20531,#19413,#10826,.T.);
#25689=EDGE_CURVE('',#20530,#19414,#10827,.T.);
#25690=EDGE_CURVE('',#20529,#19415,#10828,.T.);
#25691=EDGE_CURVE('',#20521,#19404,#10829,.T.);
#25692=EDGE_CURVE('',#20522,#19405,#10830,.T.);
#25693=EDGE_CURVE('',#20520,#19406,#10831,.T.);
#25694=EDGE_CURVE('',#20525,#19407,#10832,.T.);
#25695=EDGE_CURVE('',#20524,#19408,#10833,.T.);
#25696=EDGE_CURVE('',#20523,#19409,#10834,.T.);
#25697=EDGE_CURVE('',#20515,#19398,#10835,.T.);
#25698=EDGE_CURVE('',#20516,#19399,#10836,.T.);
#25699=EDGE_CURVE('',#20514,#19400,#10837,.T.);
#25700=EDGE_CURVE('',#20519,#19401,#10838,.T.);
#25701=EDGE_CURVE('',#20518,#19402,#10839,.T.);
#25702=EDGE_CURVE('',#20517,#19403,#10840,.T.);
#25703=EDGE_CURVE('',#20509,#19392,#10841,.T.);
#25704=EDGE_CURVE('',#20510,#19393,#10842,.T.);
#25705=EDGE_CURVE('',#20508,#19394,#10843,.T.);
#25706=EDGE_CURVE('',#20513,#19395,#10844,.T.);
#25707=EDGE_CURVE('',#20512,#19396,#10845,.T.);
#25708=EDGE_CURVE('',#20511,#19397,#10846,.T.);
#25709=EDGE_CURVE('',#20503,#19386,#10847,.T.);
#25710=EDGE_CURVE('',#20504,#19387,#10848,.T.);
#25711=EDGE_CURVE('',#20502,#19388,#10849,.T.);
#25712=EDGE_CURVE('',#20507,#19389,#10850,.T.);
#25713=EDGE_CURVE('',#20506,#19390,#10851,.T.);
#25714=EDGE_CURVE('',#20505,#19391,#10852,.T.);
#25715=EDGE_CURVE('',#20497,#19380,#10853,.T.);
#25716=EDGE_CURVE('',#20498,#19381,#10854,.T.);
#25717=EDGE_CURVE('',#20496,#19382,#10855,.T.);
#25718=EDGE_CURVE('',#20501,#19383,#10856,.T.);
#25719=EDGE_CURVE('',#20500,#19384,#10857,.T.);
#25720=EDGE_CURVE('',#20499,#19385,#10858,.T.);
#25721=EDGE_CURVE('',#20491,#19374,#10859,.T.);
#25722=EDGE_CURVE('',#20492,#19375,#10860,.T.);
#25723=EDGE_CURVE('',#20490,#19376,#10861,.T.);
#25724=EDGE_CURVE('',#20495,#19377,#10862,.T.);
#25725=EDGE_CURVE('',#20494,#19378,#10863,.T.);
#25726=EDGE_CURVE('',#20493,#19379,#10864,.T.);
#25727=EDGE_CURVE('',#20485,#19368,#10865,.T.);
#25728=EDGE_CURVE('',#20486,#19369,#10866,.T.);
#25729=EDGE_CURVE('',#20484,#19370,#10867,.T.);
#25730=EDGE_CURVE('',#20489,#19371,#10868,.T.);
#25731=EDGE_CURVE('',#20488,#19372,#10869,.T.);
#25732=EDGE_CURVE('',#20487,#19373,#10870,.T.);
#25733=EDGE_CURVE('',#20479,#19362,#10871,.T.);
#25734=EDGE_CURVE('',#20480,#19363,#10872,.T.);
#25735=EDGE_CURVE('',#20478,#19364,#10873,.T.);
#25736=EDGE_CURVE('',#20483,#19365,#10874,.T.);
#25737=EDGE_CURVE('',#20482,#19366,#10875,.T.);
#25738=EDGE_CURVE('',#20481,#19367,#10876,.T.);
#25739=EDGE_CURVE('',#20473,#19356,#10877,.T.);
#25740=EDGE_CURVE('',#20474,#19357,#10878,.T.);
#25741=EDGE_CURVE('',#20472,#19358,#10879,.T.);
#25742=EDGE_CURVE('',#20477,#19359,#10880,.T.);
#25743=EDGE_CURVE('',#20476,#19360,#10881,.T.);
#25744=EDGE_CURVE('',#20475,#19361,#10882,.T.);
#25745=EDGE_CURVE('',#20467,#19350,#10883,.T.);
#25746=EDGE_CURVE('',#20468,#19351,#10884,.T.);
#25747=EDGE_CURVE('',#20466,#19352,#10885,.T.);
#25748=EDGE_CURVE('',#20471,#19353,#10886,.T.);
#25749=EDGE_CURVE('',#20470,#19354,#10887,.T.);
#25750=EDGE_CURVE('',#20469,#19355,#10888,.T.);
#25751=EDGE_CURVE('',#20461,#19344,#10889,.T.);
#25752=EDGE_CURVE('',#20462,#19345,#10890,.T.);
#25753=EDGE_CURVE('',#20460,#19346,#10891,.T.);
#25754=EDGE_CURVE('',#20465,#19347,#10892,.T.);
#25755=EDGE_CURVE('',#20464,#19348,#10893,.T.);
#25756=EDGE_CURVE('',#20463,#19349,#10894,.T.);
#25757=EDGE_CURVE('',#20455,#19338,#10895,.T.);
#25758=EDGE_CURVE('',#20456,#19339,#10896,.T.);
#25759=EDGE_CURVE('',#20454,#19340,#10897,.T.);
#25760=EDGE_CURVE('',#20459,#19341,#10898,.T.);
#25761=EDGE_CURVE('',#20458,#19342,#10899,.T.);
#25762=EDGE_CURVE('',#20457,#19343,#10900,.T.);
#25763=EDGE_CURVE('',#20449,#19332,#10901,.T.);
#25764=EDGE_CURVE('',#20450,#19333,#10902,.T.);
#25765=EDGE_CURVE('',#20448,#19334,#10903,.T.);
#25766=EDGE_CURVE('',#20453,#19335,#10904,.T.);
#25767=EDGE_CURVE('',#20452,#19336,#10905,.T.);
#25768=EDGE_CURVE('',#20451,#19337,#10906,.T.);
#25769=EDGE_CURVE('',#20443,#19326,#10907,.T.);
#25770=EDGE_CURVE('',#20444,#19327,#10908,.T.);
#25771=EDGE_CURVE('',#20442,#19328,#10909,.T.);
#25772=EDGE_CURVE('',#20447,#19329,#10910,.T.);
#25773=EDGE_CURVE('',#20446,#19330,#10911,.T.);
#25774=EDGE_CURVE('',#20445,#19331,#10912,.T.);
#25775=EDGE_CURVE('',#20437,#19320,#10913,.T.);
#25776=EDGE_CURVE('',#20438,#19321,#10914,.T.);
#25777=EDGE_CURVE('',#20436,#19322,#10915,.T.);
#25778=EDGE_CURVE('',#20441,#19323,#10916,.T.);
#25779=EDGE_CURVE('',#20440,#19324,#10917,.T.);
#25780=EDGE_CURVE('',#20439,#19325,#10918,.T.);
#25781=EDGE_CURVE('',#20431,#19314,#10919,.T.);
#25782=EDGE_CURVE('',#20432,#19315,#10920,.T.);
#25783=EDGE_CURVE('',#20430,#19316,#10921,.T.);
#25784=EDGE_CURVE('',#20435,#19317,#10922,.T.);
#25785=EDGE_CURVE('',#20434,#19318,#10923,.T.);
#25786=EDGE_CURVE('',#20433,#19319,#10924,.T.);
#25787=EDGE_CURVE('',#20425,#19308,#10925,.T.);
#25788=EDGE_CURVE('',#20426,#19309,#10926,.T.);
#25789=EDGE_CURVE('',#20424,#19310,#10927,.T.);
#25790=EDGE_CURVE('',#20429,#19311,#10928,.T.);
#25791=EDGE_CURVE('',#20428,#19312,#10929,.T.);
#25792=EDGE_CURVE('',#20427,#19313,#10930,.T.);
#25793=EDGE_CURVE('',#20419,#19302,#10931,.T.);
#25794=EDGE_CURVE('',#20420,#19303,#10932,.T.);
#25795=EDGE_CURVE('',#20418,#19304,#10933,.T.);
#25796=EDGE_CURVE('',#20423,#19305,#10934,.T.);
#25797=EDGE_CURVE('',#20422,#19306,#10935,.T.);
#25798=EDGE_CURVE('',#20421,#19307,#10936,.T.);
#25799=EDGE_CURVE('',#20413,#19296,#10937,.T.);
#25800=EDGE_CURVE('',#20414,#19297,#10938,.T.);
#25801=EDGE_CURVE('',#20412,#19298,#10939,.T.);
#25802=EDGE_CURVE('',#20417,#19299,#10940,.T.);
#25803=EDGE_CURVE('',#20416,#19300,#10941,.T.);
#25804=EDGE_CURVE('',#20415,#19301,#10942,.T.);
#25805=EDGE_CURVE('',#20407,#19290,#10943,.T.);
#25806=EDGE_CURVE('',#20408,#19291,#10944,.T.);
#25807=EDGE_CURVE('',#20406,#19292,#10945,.T.);
#25808=EDGE_CURVE('',#20411,#19293,#10946,.T.);
#25809=EDGE_CURVE('',#20410,#19294,#10947,.T.);
#25810=EDGE_CURVE('',#20409,#19295,#10948,.T.);
#25811=EDGE_CURVE('',#20401,#19284,#10949,.T.);
#25812=EDGE_CURVE('',#20402,#19285,#10950,.T.);
#25813=EDGE_CURVE('',#20400,#19286,#10951,.T.);
#25814=EDGE_CURVE('',#20405,#19287,#10952,.T.);
#25815=EDGE_CURVE('',#20404,#19288,#10953,.T.);
#25816=EDGE_CURVE('',#20403,#19289,#10954,.T.);
#25817=EDGE_CURVE('',#20395,#19278,#10955,.T.);
#25818=EDGE_CURVE('',#20396,#19279,#10956,.T.);
#25819=EDGE_CURVE('',#20394,#19280,#10957,.T.);
#25820=EDGE_CURVE('',#20399,#19281,#10958,.T.);
#25821=EDGE_CURVE('',#20398,#19282,#10959,.T.);
#25822=EDGE_CURVE('',#20397,#19283,#10960,.T.);
#25823=EDGE_CURVE('',#20389,#19272,#10961,.T.);
#25824=EDGE_CURVE('',#20390,#19273,#10962,.T.);
#25825=EDGE_CURVE('',#20388,#19274,#10963,.T.);
#25826=EDGE_CURVE('',#20393,#19275,#10964,.T.);
#25827=EDGE_CURVE('',#20392,#19276,#10965,.T.);
#25828=EDGE_CURVE('',#20391,#19277,#10966,.T.);
#25829=EDGE_CURVE('',#20383,#19266,#10967,.T.);
#25830=EDGE_CURVE('',#20384,#19267,#10968,.T.);
#25831=EDGE_CURVE('',#20382,#19268,#10969,.T.);
#25832=EDGE_CURVE('',#20387,#19269,#10970,.T.);
#25833=EDGE_CURVE('',#20386,#19270,#10971,.T.);
#25834=EDGE_CURVE('',#20385,#19271,#10972,.T.);
#25835=EDGE_CURVE('',#20377,#19260,#10973,.T.);
#25836=EDGE_CURVE('',#20378,#19261,#10974,.T.);
#25837=EDGE_CURVE('',#20376,#19262,#10975,.T.);
#25838=EDGE_CURVE('',#20381,#19263,#10976,.T.);
#25839=EDGE_CURVE('',#20380,#19264,#10977,.T.);
#25840=EDGE_CURVE('',#20379,#19265,#10978,.T.);
#25841=EDGE_CURVE('',#20371,#19254,#10979,.T.);
#25842=EDGE_CURVE('',#20372,#19255,#10980,.T.);
#25843=EDGE_CURVE('',#20370,#19256,#10981,.T.);
#25844=EDGE_CURVE('',#20375,#19257,#10982,.T.);
#25845=EDGE_CURVE('',#20374,#19258,#10983,.T.);
#25846=EDGE_CURVE('',#20373,#19259,#10984,.T.);
#25847=EDGE_CURVE('',#20365,#19248,#10985,.T.);
#25848=EDGE_CURVE('',#20366,#19249,#10986,.T.);
#25849=EDGE_CURVE('',#20364,#19250,#10987,.T.);
#25850=EDGE_CURVE('',#20369,#19251,#10988,.T.);
#25851=EDGE_CURVE('',#20368,#19252,#10989,.T.);
#25852=EDGE_CURVE('',#20367,#19253,#10990,.T.);
#25853=EDGE_CURVE('',#20359,#19242,#10991,.T.);
#25854=EDGE_CURVE('',#20360,#19243,#10992,.T.);
#25855=EDGE_CURVE('',#20358,#19244,#10993,.T.);
#25856=EDGE_CURVE('',#20363,#19245,#10994,.T.);
#25857=EDGE_CURVE('',#20362,#19246,#10995,.T.);
#25858=EDGE_CURVE('',#20361,#19247,#10996,.T.);
#25859=EDGE_CURVE('',#20353,#19236,#10997,.T.);
#25860=EDGE_CURVE('',#20354,#19237,#10998,.T.);
#25861=EDGE_CURVE('',#20352,#19238,#10999,.T.);
#25862=EDGE_CURVE('',#20357,#19239,#11000,.T.);
#25863=EDGE_CURVE('',#20356,#19240,#11001,.T.);
#25864=EDGE_CURVE('',#20355,#19241,#11002,.T.);
#25865=EDGE_CURVE('',#20347,#19230,#11003,.T.);
#25866=EDGE_CURVE('',#20348,#19231,#11004,.T.);
#25867=EDGE_CURVE('',#20346,#19232,#11005,.T.);
#25868=EDGE_CURVE('',#20351,#19233,#11006,.T.);
#25869=EDGE_CURVE('',#20350,#19234,#11007,.T.);
#25870=EDGE_CURVE('',#20349,#19235,#11008,.T.);
#25871=EDGE_CURVE('',#20341,#19224,#11009,.T.);
#25872=EDGE_CURVE('',#20342,#19225,#11010,.T.);
#25873=EDGE_CURVE('',#20340,#19226,#11011,.T.);
#25874=EDGE_CURVE('',#20345,#19227,#11012,.T.);
#25875=EDGE_CURVE('',#20344,#19228,#11013,.T.);
#25876=EDGE_CURVE('',#20343,#19229,#11014,.T.);
#25877=EDGE_CURVE('',#20335,#19218,#11015,.T.);
#25878=EDGE_CURVE('',#20336,#19219,#11016,.T.);
#25879=EDGE_CURVE('',#20334,#19220,#11017,.T.);
#25880=EDGE_CURVE('',#20339,#19221,#11018,.T.);
#25881=EDGE_CURVE('',#20338,#19222,#11019,.T.);
#25882=EDGE_CURVE('',#20337,#19223,#11020,.T.);
#25883=EDGE_CURVE('',#20329,#19212,#11021,.T.);
#25884=EDGE_CURVE('',#20330,#19213,#11022,.T.);
#25885=EDGE_CURVE('',#20328,#19214,#11023,.T.);
#25886=EDGE_CURVE('',#20333,#19215,#11024,.T.);
#25887=EDGE_CURVE('',#20332,#19216,#11025,.T.);
#25888=EDGE_CURVE('',#20331,#19217,#11026,.T.);
#25889=EDGE_CURVE('',#20323,#19206,#11027,.T.);
#25890=EDGE_CURVE('',#20324,#19207,#11028,.T.);
#25891=EDGE_CURVE('',#20322,#19208,#11029,.T.);
#25892=EDGE_CURVE('',#20327,#19209,#11030,.T.);
#25893=EDGE_CURVE('',#20326,#19210,#11031,.T.);
#25894=EDGE_CURVE('',#20325,#19211,#11032,.T.);
#25895=EDGE_CURVE('',#20317,#19200,#11033,.T.);
#25896=EDGE_CURVE('',#20318,#19201,#11034,.T.);
#25897=EDGE_CURVE('',#20316,#19202,#11035,.T.);
#25898=EDGE_CURVE('',#20321,#19203,#11036,.T.);
#25899=EDGE_CURVE('',#20320,#19204,#11037,.T.);
#25900=EDGE_CURVE('',#20319,#19205,#11038,.T.);
#25901=EDGE_CURVE('',#20311,#19194,#11039,.T.);
#25902=EDGE_CURVE('',#20312,#19195,#11040,.T.);
#25903=EDGE_CURVE('',#20310,#19196,#11041,.T.);
#25904=EDGE_CURVE('',#20315,#19197,#11042,.T.);
#25905=EDGE_CURVE('',#20314,#19198,#11043,.T.);
#25906=EDGE_CURVE('',#20313,#19199,#11044,.T.);
#25907=EDGE_CURVE('',#20305,#19188,#11045,.T.);
#25908=EDGE_CURVE('',#20306,#19189,#11046,.T.);
#25909=EDGE_CURVE('',#20304,#19190,#11047,.T.);
#25910=EDGE_CURVE('',#20309,#19191,#11048,.T.);
#25911=EDGE_CURVE('',#20308,#19192,#11049,.T.);
#25912=EDGE_CURVE('',#20307,#19193,#11050,.T.);
#25913=EDGE_CURVE('',#20299,#19182,#11051,.T.);
#25914=EDGE_CURVE('',#20300,#19183,#11052,.T.);
#25915=EDGE_CURVE('',#20298,#19184,#11053,.T.);
#25916=EDGE_CURVE('',#20303,#19185,#11054,.T.);
#25917=EDGE_CURVE('',#20302,#19186,#11055,.T.);
#25918=EDGE_CURVE('',#20301,#19187,#11056,.T.);
#25919=EDGE_CURVE('',#20293,#19176,#11057,.T.);
#25920=EDGE_CURVE('',#20294,#19177,#11058,.T.);
#25921=EDGE_CURVE('',#20292,#19178,#11059,.T.);
#25922=EDGE_CURVE('',#20297,#19179,#11060,.T.);
#25923=EDGE_CURVE('',#20296,#19180,#11061,.T.);
#25924=EDGE_CURVE('',#20295,#19181,#11062,.T.);
#25925=EDGE_CURVE('',#20287,#19170,#11063,.T.);
#25926=EDGE_CURVE('',#20288,#19171,#11064,.T.);
#25927=EDGE_CURVE('',#20286,#19172,#11065,.T.);
#25928=EDGE_CURVE('',#20291,#19173,#11066,.T.);
#25929=EDGE_CURVE('',#20290,#19174,#11067,.T.);
#25930=EDGE_CURVE('',#20289,#19175,#11068,.T.);
#25931=EDGE_CURVE('',#20281,#19164,#11069,.T.);
#25932=EDGE_CURVE('',#20282,#19165,#11070,.T.);
#25933=EDGE_CURVE('',#20280,#19166,#11071,.T.);
#25934=EDGE_CURVE('',#20285,#19167,#11072,.T.);
#25935=EDGE_CURVE('',#20284,#19168,#11073,.T.);
#25936=EDGE_CURVE('',#20283,#19169,#11074,.T.);
#25937=EDGE_CURVE('',#20275,#19158,#11075,.T.);
#25938=EDGE_CURVE('',#20276,#19159,#11076,.T.);
#25939=EDGE_CURVE('',#20274,#19160,#11077,.T.);
#25940=EDGE_CURVE('',#20279,#19161,#11078,.T.);
#25941=EDGE_CURVE('',#20278,#19162,#11079,.T.);
#25942=EDGE_CURVE('',#20277,#19163,#11080,.T.);
#25943=EDGE_CURVE('',#20269,#19152,#11081,.T.);
#25944=EDGE_CURVE('',#20270,#19153,#11082,.T.);
#25945=EDGE_CURVE('',#20268,#19154,#11083,.T.);
#25946=EDGE_CURVE('',#20273,#19155,#11084,.T.);
#25947=EDGE_CURVE('',#20272,#19156,#11085,.T.);
#25948=EDGE_CURVE('',#20271,#19157,#11086,.T.);
#25949=EDGE_CURVE('',#20263,#19146,#11087,.T.);
#25950=EDGE_CURVE('',#20264,#19147,#11088,.T.);
#25951=EDGE_CURVE('',#20262,#19148,#11089,.T.);
#25952=EDGE_CURVE('',#20267,#19149,#11090,.T.);
#25953=EDGE_CURVE('',#20266,#19150,#11091,.T.);
#25954=EDGE_CURVE('',#20265,#19151,#11092,.T.);
#25955=EDGE_CURVE('',#20257,#19140,#11093,.T.);
#25956=EDGE_CURVE('',#20258,#19141,#11094,.T.);
#25957=EDGE_CURVE('',#20256,#19142,#11095,.T.);
#25958=EDGE_CURVE('',#20261,#19143,#11096,.T.);
#25959=EDGE_CURVE('',#20260,#19144,#11097,.T.);
#25960=EDGE_CURVE('',#20259,#19145,#11098,.T.);
#25961=EDGE_CURVE('',#20251,#19134,#11099,.T.);
#25962=EDGE_CURVE('',#20252,#19135,#11100,.T.);
#25963=EDGE_CURVE('',#20250,#19136,#11101,.T.);
#25964=EDGE_CURVE('',#20255,#19137,#11102,.T.);
#25965=EDGE_CURVE('',#20254,#19138,#11103,.T.);
#25966=EDGE_CURVE('',#20253,#19139,#11104,.T.);
#25967=EDGE_CURVE('',#20245,#19128,#11105,.T.);
#25968=EDGE_CURVE('',#20246,#19129,#11106,.T.);
#25969=EDGE_CURVE('',#20244,#19130,#11107,.T.);
#25970=EDGE_CURVE('',#20249,#19131,#11108,.T.);
#25971=EDGE_CURVE('',#20248,#19132,#11109,.T.);
#25972=EDGE_CURVE('',#20247,#19133,#11110,.T.);
#25973=EDGE_CURVE('',#20239,#19122,#11111,.T.);
#25974=EDGE_CURVE('',#20240,#19123,#11112,.T.);
#25975=EDGE_CURVE('',#20238,#19124,#11113,.T.);
#25976=EDGE_CURVE('',#20243,#19125,#11114,.T.);
#25977=EDGE_CURVE('',#20242,#19126,#11115,.T.);
#25978=EDGE_CURVE('',#20241,#19127,#11116,.T.);
#25979=EDGE_CURVE('',#20233,#19116,#11117,.T.);
#25980=EDGE_CURVE('',#20234,#19117,#11118,.T.);
#25981=EDGE_CURVE('',#20232,#19118,#11119,.T.);
#25982=EDGE_CURVE('',#20237,#19119,#11120,.T.);
#25983=EDGE_CURVE('',#20236,#19120,#11121,.T.);
#25984=EDGE_CURVE('',#20235,#19121,#11122,.T.);
#25985=EDGE_CURVE('',#20227,#19110,#11123,.T.);
#25986=EDGE_CURVE('',#20228,#19111,#11124,.T.);
#25987=EDGE_CURVE('',#20226,#19112,#11125,.T.);
#25988=EDGE_CURVE('',#20231,#19113,#11126,.T.);
#25989=EDGE_CURVE('',#20230,#19114,#11127,.T.);
#25990=EDGE_CURVE('',#20229,#19115,#11128,.T.);
#25991=EDGE_CURVE('',#20221,#19104,#11129,.T.);
#25992=EDGE_CURVE('',#20222,#19105,#11130,.T.);
#25993=EDGE_CURVE('',#20220,#19106,#11131,.T.);
#25994=EDGE_CURVE('',#20225,#19107,#11132,.T.);
#25995=EDGE_CURVE('',#20224,#19108,#11133,.T.);
#25996=EDGE_CURVE('',#20223,#19109,#11134,.T.);
#25997=EDGE_CURVE('',#20215,#19098,#11135,.T.);
#25998=EDGE_CURVE('',#20216,#19099,#11136,.T.);
#25999=EDGE_CURVE('',#20214,#19100,#11137,.T.);
#26000=EDGE_CURVE('',#20219,#19101,#11138,.T.);
#26001=EDGE_CURVE('',#20218,#19102,#11139,.T.);
#26002=EDGE_CURVE('',#20217,#19103,#11140,.T.);
#26003=EDGE_CURVE('',#20209,#19092,#11141,.T.);
#26004=EDGE_CURVE('',#20210,#19093,#11142,.T.);
#26005=EDGE_CURVE('',#20208,#19094,#11143,.T.);
#26006=EDGE_CURVE('',#20213,#19095,#11144,.T.);
#26007=EDGE_CURVE('',#20212,#19096,#11145,.T.);
#26008=EDGE_CURVE('',#20211,#19097,#11146,.T.);
#26009=EDGE_CURVE('',#20203,#19086,#11147,.T.);
#26010=EDGE_CURVE('',#20204,#19087,#11148,.T.);
#26011=EDGE_CURVE('',#20202,#19088,#11149,.T.);
#26012=EDGE_CURVE('',#20207,#19089,#11150,.T.);
#26013=EDGE_CURVE('',#20206,#19090,#11151,.T.);
#26014=EDGE_CURVE('',#20205,#19091,#11152,.T.);
#26015=EDGE_CURVE('',#20197,#19080,#11153,.T.);
#26016=EDGE_CURVE('',#20198,#19081,#11154,.T.);
#26017=EDGE_CURVE('',#20196,#19082,#11155,.T.);
#26018=EDGE_CURVE('',#20201,#19083,#11156,.T.);
#26019=EDGE_CURVE('',#20200,#19084,#11157,.T.);
#26020=EDGE_CURVE('',#20199,#19085,#11158,.T.);
#26021=EDGE_CURVE('',#20191,#19074,#11159,.T.);
#26022=EDGE_CURVE('',#20192,#19075,#11160,.T.);
#26023=EDGE_CURVE('',#20190,#19076,#11161,.T.);
#26024=EDGE_CURVE('',#20195,#19077,#11162,.T.);
#26025=EDGE_CURVE('',#20194,#19078,#11163,.T.);
#26026=EDGE_CURVE('',#20193,#19079,#11164,.T.);
#26027=EDGE_CURVE('',#20185,#19068,#11165,.T.);
#26028=EDGE_CURVE('',#20186,#19069,#11166,.T.);
#26029=EDGE_CURVE('',#20184,#19070,#11167,.T.);
#26030=EDGE_CURVE('',#20189,#19071,#11168,.T.);
#26031=EDGE_CURVE('',#20188,#19072,#11169,.T.);
#26032=EDGE_CURVE('',#20187,#19073,#11170,.T.);
#26033=EDGE_CURVE('',#20179,#19062,#11171,.T.);
#26034=EDGE_CURVE('',#20180,#19063,#11172,.T.);
#26035=EDGE_CURVE('',#20178,#19064,#11173,.T.);
#26036=EDGE_CURVE('',#20183,#19065,#11174,.T.);
#26037=EDGE_CURVE('',#20182,#19066,#11175,.T.);
#26038=EDGE_CURVE('',#20181,#19067,#11176,.T.);
#26039=EDGE_CURVE('',#20173,#19056,#11177,.T.);
#26040=EDGE_CURVE('',#20174,#19057,#11178,.T.);
#26041=EDGE_CURVE('',#20172,#19058,#11179,.T.);
#26042=EDGE_CURVE('',#20177,#19059,#11180,.T.);
#26043=EDGE_CURVE('',#20176,#19060,#11181,.T.);
#26044=EDGE_CURVE('',#20175,#19061,#11182,.T.);
#26045=EDGE_CURVE('',#20167,#19050,#11183,.T.);
#26046=EDGE_CURVE('',#20168,#19051,#11184,.T.);
#26047=EDGE_CURVE('',#20166,#19052,#11185,.T.);
#26048=EDGE_CURVE('',#20171,#19053,#11186,.T.);
#26049=EDGE_CURVE('',#20170,#19054,#11187,.T.);
#26050=EDGE_CURVE('',#20169,#19055,#11188,.T.);
#26051=EDGE_CURVE('',#20161,#19044,#11189,.T.);
#26052=EDGE_CURVE('',#20162,#19045,#11190,.T.);
#26053=EDGE_CURVE('',#20160,#19046,#11191,.T.);
#26054=EDGE_CURVE('',#20165,#19047,#11192,.T.);
#26055=EDGE_CURVE('',#20164,#19048,#11193,.T.);
#26056=EDGE_CURVE('',#20163,#19049,#11194,.T.);
#26057=EDGE_CURVE('',#20155,#19038,#11195,.T.);
#26058=EDGE_CURVE('',#20156,#19039,#11196,.T.);
#26059=EDGE_CURVE('',#20154,#19040,#11197,.T.);
#26060=EDGE_CURVE('',#20159,#19041,#11198,.T.);
#26061=EDGE_CURVE('',#20158,#19042,#11199,.T.);
#26062=EDGE_CURVE('',#20157,#19043,#11200,.T.);
#26063=EDGE_CURVE('',#20149,#19032,#11201,.T.);
#26064=EDGE_CURVE('',#20150,#19033,#11202,.T.);
#26065=EDGE_CURVE('',#20148,#19034,#11203,.T.);
#26066=EDGE_CURVE('',#20153,#19035,#11204,.T.);
#26067=EDGE_CURVE('',#20152,#19036,#11205,.T.);
#26068=EDGE_CURVE('',#20151,#19037,#11206,.T.);
#26069=EDGE_CURVE('',#20143,#19026,#11207,.T.);
#26070=EDGE_CURVE('',#20144,#19027,#11208,.T.);
#26071=EDGE_CURVE('',#20142,#19028,#11209,.T.);
#26072=EDGE_CURVE('',#20147,#19029,#11210,.T.);
#26073=EDGE_CURVE('',#20146,#19030,#11211,.T.);
#26074=EDGE_CURVE('',#20145,#19031,#11212,.T.);
#26075=EDGE_CURVE('',#20137,#19020,#11213,.T.);
#26076=EDGE_CURVE('',#20138,#19021,#11214,.T.);
#26077=EDGE_CURVE('',#20136,#19022,#11215,.T.);
#26078=EDGE_CURVE('',#20141,#19023,#11216,.T.);
#26079=EDGE_CURVE('',#20140,#19024,#11217,.T.);
#26080=EDGE_CURVE('',#20139,#19025,#11218,.T.);
#26081=EDGE_CURVE('',#20131,#19014,#11219,.T.);
#26082=EDGE_CURVE('',#20132,#19015,#11220,.T.);
#26083=EDGE_CURVE('',#20130,#19016,#11221,.T.);
#26084=EDGE_CURVE('',#20135,#19017,#11222,.T.);
#26085=EDGE_CURVE('',#20134,#19018,#11223,.T.);
#26086=EDGE_CURVE('',#20133,#19019,#11224,.T.);
#26087=EDGE_CURVE('',#20125,#19008,#11225,.T.);
#26088=EDGE_CURVE('',#20126,#19009,#11226,.T.);
#26089=EDGE_CURVE('',#20124,#19010,#11227,.T.);
#26090=EDGE_CURVE('',#20129,#19011,#11228,.T.);
#26091=EDGE_CURVE('',#20128,#19012,#11229,.T.);
#26092=EDGE_CURVE('',#20127,#19013,#11230,.T.);
#26093=EDGE_CURVE('',#20119,#19002,#11231,.T.);
#26094=EDGE_CURVE('',#20120,#19003,#11232,.T.);
#26095=EDGE_CURVE('',#20118,#19004,#11233,.T.);
#26096=EDGE_CURVE('',#20123,#19005,#11234,.T.);
#26097=EDGE_CURVE('',#20122,#19006,#11235,.T.);
#26098=EDGE_CURVE('',#20121,#19007,#11236,.T.);
#26099=EDGE_CURVE('',#20113,#18996,#11237,.T.);
#26100=EDGE_CURVE('',#20114,#18997,#11238,.T.);
#26101=EDGE_CURVE('',#20112,#18998,#11239,.T.);
#26102=EDGE_CURVE('',#20117,#18999,#11240,.T.);
#26103=EDGE_CURVE('',#20116,#19000,#11241,.T.);
#26104=EDGE_CURVE('',#20115,#19001,#11242,.T.);
#26105=EDGE_CURVE('',#20107,#18990,#11243,.T.);
#26106=EDGE_CURVE('',#20108,#18991,#11244,.T.);
#26107=EDGE_CURVE('',#20106,#18992,#11245,.T.);
#26108=EDGE_CURVE('',#20111,#18993,#11246,.T.);
#26109=EDGE_CURVE('',#20110,#18994,#11247,.T.);
#26110=EDGE_CURVE('',#20109,#18995,#11248,.T.);
#26111=EDGE_CURVE('',#20101,#18984,#11249,.T.);
#26112=EDGE_CURVE('',#20102,#18985,#11250,.T.);
#26113=EDGE_CURVE('',#20100,#18986,#11251,.T.);
#26114=EDGE_CURVE('',#20105,#18987,#11252,.T.);
#26115=EDGE_CURVE('',#20104,#18988,#11253,.T.);
#26116=EDGE_CURVE('',#20103,#18989,#11254,.T.);
#26117=EDGE_CURVE('',#20095,#18978,#11255,.T.);
#26118=EDGE_CURVE('',#20096,#18979,#11256,.T.);
#26119=EDGE_CURVE('',#20094,#18980,#11257,.T.);
#26120=EDGE_CURVE('',#20099,#18981,#11258,.T.);
#26121=EDGE_CURVE('',#20098,#18982,#11259,.T.);
#26122=EDGE_CURVE('',#20097,#18983,#11260,.T.);
#26123=EDGE_CURVE('',#20089,#18972,#11261,.T.);
#26124=EDGE_CURVE('',#20090,#18973,#11262,.T.);
#26125=EDGE_CURVE('',#20088,#18974,#11263,.T.);
#26126=EDGE_CURVE('',#20093,#18975,#11264,.T.);
#26127=EDGE_CURVE('',#20092,#18976,#11265,.T.);
#26128=EDGE_CURVE('',#20091,#18977,#11266,.T.);
#26129=EDGE_CURVE('',#20083,#18966,#11267,.T.);
#26130=EDGE_CURVE('',#20084,#18967,#11268,.T.);
#26131=EDGE_CURVE('',#20082,#18968,#11269,.T.);
#26132=EDGE_CURVE('',#20087,#18969,#11270,.T.);
#26133=EDGE_CURVE('',#20086,#18970,#11271,.T.);
#26134=EDGE_CURVE('',#20085,#18971,#11272,.T.);
#26135=EDGE_CURVE('',#20077,#18960,#11273,.T.);
#26136=EDGE_CURVE('',#20078,#18961,#11274,.T.);
#26137=EDGE_CURVE('',#20076,#18962,#11275,.T.);
#26138=EDGE_CURVE('',#20081,#18963,#11276,.T.);
#26139=EDGE_CURVE('',#20080,#18964,#11277,.T.);
#26140=EDGE_CURVE('',#20079,#18965,#11278,.T.);
#26141=EDGE_CURVE('',#20071,#18954,#11279,.T.);
#26142=EDGE_CURVE('',#20072,#18955,#11280,.T.);
#26143=EDGE_CURVE('',#20070,#18956,#11281,.T.);
#26144=EDGE_CURVE('',#20075,#18957,#11282,.T.);
#26145=EDGE_CURVE('',#20074,#18958,#11283,.T.);
#26146=EDGE_CURVE('',#20073,#18959,#11284,.T.);
#26147=EDGE_CURVE('',#20065,#18948,#11285,.T.);
#26148=EDGE_CURVE('',#20066,#18949,#11286,.T.);
#26149=EDGE_CURVE('',#20064,#18950,#11287,.T.);
#26150=EDGE_CURVE('',#20069,#18951,#11288,.T.);
#26151=EDGE_CURVE('',#20068,#18952,#11289,.T.);
#26152=EDGE_CURVE('',#20067,#18953,#11290,.T.);
#26153=EDGE_CURVE('',#20059,#18942,#11291,.T.);
#26154=EDGE_CURVE('',#20060,#18943,#11292,.T.);
#26155=EDGE_CURVE('',#20058,#18944,#11293,.T.);
#26156=EDGE_CURVE('',#20063,#18945,#11294,.T.);
#26157=EDGE_CURVE('',#20062,#18946,#11295,.T.);
#26158=EDGE_CURVE('',#20061,#18947,#11296,.T.);
#26159=EDGE_CURVE('',#20053,#18936,#11297,.T.);
#26160=EDGE_CURVE('',#20054,#18937,#11298,.T.);
#26161=EDGE_CURVE('',#20052,#18938,#11299,.T.);
#26162=EDGE_CURVE('',#20057,#18939,#11300,.T.);
#26163=EDGE_CURVE('',#20056,#18940,#11301,.T.);
#26164=EDGE_CURVE('',#20055,#18941,#11302,.T.);
#26165=EDGE_CURVE('',#20047,#18930,#11303,.T.);
#26166=EDGE_CURVE('',#20048,#18931,#11304,.T.);
#26167=EDGE_CURVE('',#20046,#18932,#11305,.T.);
#26168=EDGE_CURVE('',#20051,#18933,#11306,.T.);
#26169=EDGE_CURVE('',#20050,#18934,#11307,.T.);
#26170=EDGE_CURVE('',#20049,#18935,#11308,.T.);
#26171=EDGE_CURVE('',#20041,#18924,#11309,.T.);
#26172=EDGE_CURVE('',#20042,#18925,#11310,.T.);
#26173=EDGE_CURVE('',#20040,#18926,#11311,.T.);
#26174=EDGE_CURVE('',#20045,#18927,#11312,.T.);
#26175=EDGE_CURVE('',#20044,#18928,#11313,.T.);
#26176=EDGE_CURVE('',#20043,#18929,#11314,.T.);
#26177=EDGE_CURVE('',#20035,#18918,#11315,.T.);
#26178=EDGE_CURVE('',#20036,#18919,#11316,.T.);
#26179=EDGE_CURVE('',#20034,#18920,#11317,.T.);
#26180=EDGE_CURVE('',#20039,#18921,#11318,.T.);
#26181=EDGE_CURVE('',#20038,#18922,#11319,.T.);
#26182=EDGE_CURVE('',#20037,#18923,#11320,.T.);
#26183=EDGE_CURVE('',#20029,#18912,#11321,.T.);
#26184=EDGE_CURVE('',#20030,#18913,#11322,.T.);
#26185=EDGE_CURVE('',#20028,#18914,#11323,.T.);
#26186=EDGE_CURVE('',#20033,#18915,#11324,.T.);
#26187=EDGE_CURVE('',#20032,#18916,#11325,.T.);
#26188=EDGE_CURVE('',#20031,#18917,#11326,.T.);
#26189=EDGE_CURVE('',#20023,#18906,#11327,.T.);
#26190=EDGE_CURVE('',#20024,#18907,#11328,.T.);
#26191=EDGE_CURVE('',#20022,#18908,#11329,.T.);
#26192=EDGE_CURVE('',#20027,#18909,#11330,.T.);
#26193=EDGE_CURVE('',#20026,#18910,#11331,.T.);
#26194=EDGE_CURVE('',#20025,#18911,#11332,.T.);
#26195=EDGE_CURVE('',#20017,#18900,#11333,.T.);
#26196=EDGE_CURVE('',#20018,#18901,#11334,.T.);
#26197=EDGE_CURVE('',#20016,#18902,#11335,.T.);
#26198=EDGE_CURVE('',#20021,#18903,#11336,.T.);
#26199=EDGE_CURVE('',#20020,#18904,#11337,.T.);
#26200=EDGE_CURVE('',#20019,#18905,#11338,.T.);
#26201=EDGE_CURVE('',#20011,#18894,#11339,.T.);
#26202=EDGE_CURVE('',#20012,#18895,#11340,.T.);
#26203=EDGE_CURVE('',#20010,#18896,#11341,.T.);
#26204=EDGE_CURVE('',#20015,#18897,#11342,.T.);
#26205=EDGE_CURVE('',#20014,#18898,#11343,.T.);
#26206=EDGE_CURVE('',#20013,#18899,#11344,.T.);
#26207=EDGE_CURVE('',#20005,#18888,#11345,.T.);
#26208=EDGE_CURVE('',#20006,#18889,#11346,.T.);
#26209=EDGE_CURVE('',#20004,#18890,#11347,.T.);
#26210=EDGE_CURVE('',#20009,#18891,#11348,.T.);
#26211=EDGE_CURVE('',#20008,#18892,#11349,.T.);
#26212=EDGE_CURVE('',#20007,#18893,#11350,.T.);
#26213=EDGE_CURVE('',#19999,#18882,#11351,.T.);
#26214=EDGE_CURVE('',#20000,#18883,#11352,.T.);
#26215=EDGE_CURVE('',#19998,#18884,#11353,.T.);
#26216=EDGE_CURVE('',#20003,#18885,#11354,.T.);
#26217=EDGE_CURVE('',#20002,#18886,#11355,.T.);
#26218=EDGE_CURVE('',#20001,#18887,#11356,.T.);
#26219=EDGE_CURVE('',#19993,#18876,#11357,.T.);
#26220=EDGE_CURVE('',#19994,#18877,#11358,.T.);
#26221=EDGE_CURVE('',#19992,#18878,#11359,.T.);
#26222=EDGE_CURVE('',#19997,#18879,#11360,.T.);
#26223=EDGE_CURVE('',#19996,#18880,#11361,.T.);
#26224=EDGE_CURVE('',#19995,#18881,#11362,.T.);
#26225=EDGE_CURVE('',#19987,#18870,#11363,.T.);
#26226=EDGE_CURVE('',#19988,#18871,#11364,.T.);
#26227=EDGE_CURVE('',#19986,#18872,#11365,.T.);
#26228=EDGE_CURVE('',#19991,#18873,#11366,.T.);
#26229=EDGE_CURVE('',#19990,#18874,#11367,.T.);
#26230=EDGE_CURVE('',#19989,#18875,#11368,.T.);
#26231=EDGE_CURVE('',#19981,#18864,#11369,.T.);
#26232=EDGE_CURVE('',#19982,#18865,#11370,.T.);
#26233=EDGE_CURVE('',#19980,#18866,#11371,.T.);
#26234=EDGE_CURVE('',#19985,#18867,#11372,.T.);
#26235=EDGE_CURVE('',#19984,#18868,#11373,.T.);
#26236=EDGE_CURVE('',#19983,#18869,#11374,.T.);
#26237=EDGE_CURVE('',#19975,#18858,#11375,.T.);
#26238=EDGE_CURVE('',#19976,#18859,#11376,.T.);
#26239=EDGE_CURVE('',#19974,#18860,#11377,.T.);
#26240=EDGE_CURVE('',#19979,#18861,#11378,.T.);
#26241=EDGE_CURVE('',#19978,#18862,#11379,.T.);
#26242=EDGE_CURVE('',#19977,#18863,#11380,.T.);
#26243=EDGE_CURVE('',#19969,#18852,#11381,.T.);
#26244=EDGE_CURVE('',#19970,#18853,#11382,.T.);
#26245=EDGE_CURVE('',#19968,#18854,#11383,.T.);
#26246=EDGE_CURVE('',#19973,#18855,#11384,.T.);
#26247=EDGE_CURVE('',#19972,#18856,#11385,.T.);
#26248=EDGE_CURVE('',#19971,#18857,#11386,.T.);
#26249=EDGE_CURVE('',#19963,#18846,#11387,.T.);
#26250=EDGE_CURVE('',#19964,#18847,#11388,.T.);
#26251=EDGE_CURVE('',#19962,#18848,#11389,.T.);
#26252=EDGE_CURVE('',#19967,#18849,#11390,.T.);
#26253=EDGE_CURVE('',#19966,#18850,#11391,.T.);
#26254=EDGE_CURVE('',#19965,#18851,#11392,.T.);
#26255=EDGE_CURVE('',#19957,#18840,#11393,.T.);
#26256=EDGE_CURVE('',#19958,#18841,#11394,.T.);
#26257=EDGE_CURVE('',#19956,#18842,#11395,.T.);
#26258=EDGE_CURVE('',#19961,#18843,#11396,.T.);
#26259=EDGE_CURVE('',#19960,#18844,#11397,.T.);
#26260=EDGE_CURVE('',#19959,#18845,#11398,.T.);
#26261=EDGE_CURVE('',#19951,#18834,#11399,.T.);
#26262=EDGE_CURVE('',#19952,#18835,#11400,.T.);
#26263=EDGE_CURVE('',#19950,#18836,#11401,.T.);
#26264=EDGE_CURVE('',#19955,#18837,#11402,.T.);
#26265=EDGE_CURVE('',#19954,#18838,#11403,.T.);
#26266=EDGE_CURVE('',#19953,#18839,#11404,.T.);
#26267=EDGE_CURVE('',#19945,#18828,#11405,.T.);
#26268=EDGE_CURVE('',#19946,#18829,#11406,.T.);
#26269=EDGE_CURVE('',#19944,#18830,#11407,.T.);
#26270=EDGE_CURVE('',#19949,#18831,#11408,.T.);
#26271=EDGE_CURVE('',#19948,#18832,#11409,.T.);
#26272=EDGE_CURVE('',#19947,#18833,#11410,.T.);
#26273=EDGE_CURVE('',#19939,#18822,#11411,.T.);
#26274=EDGE_CURVE('',#19940,#18823,#11412,.T.);
#26275=EDGE_CURVE('',#19938,#18824,#11413,.T.);
#26276=EDGE_CURVE('',#19943,#18825,#11414,.T.);
#26277=EDGE_CURVE('',#19942,#18826,#11415,.T.);
#26278=EDGE_CURVE('',#19941,#18827,#11416,.T.);
#26279=EDGE_CURVE('',#19933,#18816,#11417,.T.);
#26280=EDGE_CURVE('',#19934,#18817,#11418,.T.);
#26281=EDGE_CURVE('',#19932,#18818,#11419,.T.);
#26282=EDGE_CURVE('',#19937,#18819,#11420,.T.);
#26283=EDGE_CURVE('',#19936,#18820,#11421,.T.);
#26284=EDGE_CURVE('',#19935,#18821,#11422,.T.);
#26285=EDGE_CURVE('',#19927,#18810,#11423,.T.);
#26286=EDGE_CURVE('',#19928,#18811,#11424,.T.);
#26287=EDGE_CURVE('',#19926,#18812,#11425,.T.);
#26288=EDGE_CURVE('',#19931,#18813,#11426,.T.);
#26289=EDGE_CURVE('',#19930,#18814,#11427,.T.);
#26290=EDGE_CURVE('',#19929,#18815,#11428,.T.);
#26291=EDGE_CURVE('',#19921,#18804,#11429,.T.);
#26292=EDGE_CURVE('',#19922,#18805,#11430,.T.);
#26293=EDGE_CURVE('',#19920,#18806,#11431,.T.);
#26294=EDGE_CURVE('',#19925,#18807,#11432,.T.);
#26295=EDGE_CURVE('',#19924,#18808,#11433,.T.);
#26296=EDGE_CURVE('',#19923,#18809,#11434,.T.);
#26297=EDGE_CURVE('',#19915,#18798,#11435,.T.);
#26298=EDGE_CURVE('',#19916,#18799,#11436,.T.);
#26299=EDGE_CURVE('',#19914,#18800,#11437,.T.);
#26300=EDGE_CURVE('',#19919,#18801,#11438,.T.);
#26301=EDGE_CURVE('',#19918,#18802,#11439,.T.);
#26302=EDGE_CURVE('',#19917,#18803,#11440,.T.);
#26303=EDGE_CURVE('',#19909,#18792,#11441,.T.);
#26304=EDGE_CURVE('',#19910,#18793,#11442,.T.);
#26305=EDGE_CURVE('',#19908,#18794,#11443,.T.);
#26306=EDGE_CURVE('',#19913,#18795,#11444,.T.);
#26307=EDGE_CURVE('',#19912,#18796,#11445,.T.);
#26308=EDGE_CURVE('',#19911,#18797,#11446,.T.);
#26309=EDGE_CURVE('',#19903,#18786,#11447,.T.);
#26310=EDGE_CURVE('',#19904,#18787,#11448,.T.);
#26311=EDGE_CURVE('',#19902,#18788,#11449,.T.);
#26312=EDGE_CURVE('',#19907,#18789,#11450,.T.);
#26313=EDGE_CURVE('',#19906,#18790,#11451,.T.);
#26314=EDGE_CURVE('',#19905,#18791,#11452,.T.);
#26315=EDGE_CURVE('',#19897,#18780,#11453,.T.);
#26316=EDGE_CURVE('',#19898,#18781,#11454,.T.);
#26317=EDGE_CURVE('',#19896,#18782,#11455,.T.);
#26318=EDGE_CURVE('',#19901,#18783,#11456,.T.);
#26319=EDGE_CURVE('',#19900,#18784,#11457,.T.);
#26320=EDGE_CURVE('',#19899,#18785,#11458,.T.);
#26321=EDGE_CURVE('',#19891,#18774,#11459,.T.);
#26322=EDGE_CURVE('',#19892,#18775,#11460,.T.);
#26323=EDGE_CURVE('',#19890,#18776,#11461,.T.);
#26324=EDGE_CURVE('',#19895,#18777,#11462,.T.);
#26325=EDGE_CURVE('',#19894,#18778,#11463,.T.);
#26326=EDGE_CURVE('',#19893,#18779,#11464,.T.);
#26327=EDGE_CURVE('',#19885,#18768,#11465,.T.);
#26328=EDGE_CURVE('',#19886,#18769,#11466,.T.);
#26329=EDGE_CURVE('',#19884,#18770,#11467,.T.);
#26330=EDGE_CURVE('',#19889,#18771,#11468,.T.);
#26331=EDGE_CURVE('',#19888,#18772,#11469,.T.);
#26332=EDGE_CURVE('',#19887,#18773,#11470,.T.);
#26333=EDGE_CURVE('',#19879,#18762,#11471,.T.);
#26334=EDGE_CURVE('',#19880,#18763,#11472,.T.);
#26335=EDGE_CURVE('',#19878,#18764,#11473,.T.);
#26336=EDGE_CURVE('',#19883,#18765,#11474,.T.);
#26337=EDGE_CURVE('',#19882,#18766,#11475,.T.);
#26338=EDGE_CURVE('',#19881,#18767,#11476,.T.);
#26339=EDGE_CURVE('',#19873,#18756,#11477,.T.);
#26340=EDGE_CURVE('',#19874,#18757,#11478,.T.);
#26341=EDGE_CURVE('',#19872,#18758,#11479,.T.);
#26342=EDGE_CURVE('',#19877,#18759,#11480,.T.);
#26343=EDGE_CURVE('',#19876,#18760,#11481,.T.);
#26344=EDGE_CURVE('',#19875,#18761,#11482,.T.);
#26345=EDGE_CURVE('',#19867,#18750,#11483,.T.);
#26346=EDGE_CURVE('',#19868,#18751,#11484,.T.);
#26347=EDGE_CURVE('',#19866,#18752,#11485,.T.);
#26348=EDGE_CURVE('',#19871,#18753,#11486,.T.);
#26349=EDGE_CURVE('',#19870,#18754,#11487,.T.);
#26350=EDGE_CURVE('',#19869,#18755,#11488,.T.);
#26351=EDGE_CURVE('',#19861,#18744,#11489,.T.);
#26352=EDGE_CURVE('',#19862,#18745,#11490,.T.);
#26353=EDGE_CURVE('',#19860,#18746,#11491,.T.);
#26354=EDGE_CURVE('',#19865,#18747,#11492,.T.);
#26355=EDGE_CURVE('',#19864,#18748,#11493,.T.);
#26356=EDGE_CURVE('',#19863,#18749,#11494,.T.);
#26357=EDGE_CURVE('',#19855,#18738,#11495,.T.);
#26358=EDGE_CURVE('',#19856,#18739,#11496,.T.);
#26359=EDGE_CURVE('',#19854,#18740,#11497,.T.);
#26360=EDGE_CURVE('',#19859,#18741,#11498,.T.);
#26361=EDGE_CURVE('',#19858,#18742,#11499,.T.);
#26362=EDGE_CURVE('',#19857,#18743,#11500,.T.);
#26363=EDGE_CURVE('',#19849,#18732,#11501,.T.);
#26364=EDGE_CURVE('',#19850,#18733,#11502,.T.);
#26365=EDGE_CURVE('',#19848,#18734,#11503,.T.);
#26366=EDGE_CURVE('',#19853,#18735,#11504,.T.);
#26367=EDGE_CURVE('',#19852,#18736,#11505,.T.);
#26368=EDGE_CURVE('',#19851,#18737,#11506,.T.);
#26369=EDGE_CURVE('',#19843,#18726,#11507,.T.);
#26370=EDGE_CURVE('',#19844,#18727,#11508,.T.);
#26371=EDGE_CURVE('',#19842,#18728,#11509,.T.);
#26372=EDGE_CURVE('',#19847,#18729,#11510,.T.);
#26373=EDGE_CURVE('',#19846,#18730,#11511,.T.);
#26374=EDGE_CURVE('',#19845,#18731,#11512,.T.);
#26375=EDGE_CURVE('',#19837,#18720,#11513,.T.);
#26376=EDGE_CURVE('',#19838,#18721,#11514,.T.);
#26377=EDGE_CURVE('',#19836,#18722,#11515,.T.);
#26378=EDGE_CURVE('',#19841,#18723,#11516,.T.);
#26379=EDGE_CURVE('',#19840,#18724,#11517,.T.);
#26380=EDGE_CURVE('',#19839,#18725,#11518,.T.);
#26381=EDGE_CURVE('',#19831,#18714,#11519,.T.);
#26382=EDGE_CURVE('',#19832,#18715,#11520,.T.);
#26383=EDGE_CURVE('',#19830,#18716,#11521,.T.);
#26384=EDGE_CURVE('',#19835,#18717,#11522,.T.);
#26385=EDGE_CURVE('',#19834,#18718,#11523,.T.);
#26386=EDGE_CURVE('',#19833,#18719,#11524,.T.);
#26387=EDGE_CURVE('',#19825,#18708,#11525,.T.);
#26388=EDGE_CURVE('',#19826,#18709,#11526,.T.);
#26389=EDGE_CURVE('',#19824,#18710,#11527,.T.);
#26390=EDGE_CURVE('',#19829,#18711,#11528,.T.);
#26391=EDGE_CURVE('',#19828,#18712,#11529,.T.);
#26392=EDGE_CURVE('',#19827,#18713,#11530,.T.);
#26393=EDGE_CURVE('',#19819,#18702,#11531,.T.);
#26394=EDGE_CURVE('',#19820,#18703,#11532,.T.);
#26395=EDGE_CURVE('',#19818,#18704,#11533,.T.);
#26396=EDGE_CURVE('',#19823,#18705,#11534,.T.);
#26397=EDGE_CURVE('',#19822,#18706,#11535,.T.);
#26398=EDGE_CURVE('',#19821,#18707,#11536,.T.);
#26399=EDGE_CURVE('',#19813,#18696,#11537,.T.);
#26400=EDGE_CURVE('',#19814,#18697,#11538,.T.);
#26401=EDGE_CURVE('',#19812,#18698,#11539,.T.);
#26402=EDGE_CURVE('',#19817,#18699,#11540,.T.);
#26403=EDGE_CURVE('',#19816,#18700,#11541,.T.);
#26404=EDGE_CURVE('',#19815,#18701,#11542,.T.);
#26405=EDGE_CURVE('',#19807,#18690,#11543,.T.);
#26406=EDGE_CURVE('',#19808,#18691,#11544,.T.);
#26407=EDGE_CURVE('',#19806,#18692,#11545,.T.);
#26408=EDGE_CURVE('',#19811,#18693,#11546,.T.);
#26409=EDGE_CURVE('',#19810,#18694,#11547,.T.);
#26410=EDGE_CURVE('',#19809,#18695,#11548,.T.);
#26411=EDGE_CURVE('',#19801,#18684,#11549,.T.);
#26412=EDGE_CURVE('',#19802,#18685,#11550,.T.);
#26413=EDGE_CURVE('',#19800,#18686,#11551,.T.);
#26414=EDGE_CURVE('',#19805,#18687,#11552,.T.);
#26415=EDGE_CURVE('',#19804,#18688,#11553,.T.);
#26416=EDGE_CURVE('',#19803,#18689,#11554,.T.);
#26417=EDGE_CURVE('',#19795,#18678,#11555,.T.);
#26418=EDGE_CURVE('',#19796,#18679,#11556,.T.);
#26419=EDGE_CURVE('',#19794,#18680,#11557,.T.);
#26420=EDGE_CURVE('',#19799,#18681,#11558,.T.);
#26421=EDGE_CURVE('',#19798,#18682,#11559,.T.);
#26422=EDGE_CURVE('',#19797,#18683,#11560,.T.);
#26423=EDGE_CURVE('',#19789,#18672,#11561,.T.);
#26424=EDGE_CURVE('',#19790,#18673,#11562,.T.);
#26425=EDGE_CURVE('',#19788,#18674,#11563,.T.);
#26426=EDGE_CURVE('',#19793,#18675,#11564,.T.);
#26427=EDGE_CURVE('',#19792,#18676,#11565,.T.);
#26428=EDGE_CURVE('',#19791,#18677,#11566,.T.);
#26429=EDGE_CURVE('',#19783,#18666,#11567,.T.);
#26430=EDGE_CURVE('',#19784,#18667,#11568,.T.);
#26431=EDGE_CURVE('',#19782,#18668,#11569,.T.);
#26432=EDGE_CURVE('',#19787,#18669,#11570,.T.);
#26433=EDGE_CURVE('',#19786,#18670,#11571,.T.);
#26434=EDGE_CURVE('',#19785,#18671,#11572,.T.);
#26435=EDGE_CURVE('',#19777,#18660,#11573,.T.);
#26436=EDGE_CURVE('',#19778,#18661,#11574,.T.);
#26437=EDGE_CURVE('',#19776,#18662,#11575,.T.);
#26438=EDGE_CURVE('',#19781,#18663,#11576,.T.);
#26439=EDGE_CURVE('',#19780,#18664,#11577,.T.);
#26440=EDGE_CURVE('',#19779,#18665,#11578,.T.);
#26441=EDGE_CURVE('',#19771,#18654,#11579,.T.);
#26442=EDGE_CURVE('',#19772,#18655,#11580,.T.);
#26443=EDGE_CURVE('',#19770,#18656,#11581,.T.);
#26444=EDGE_CURVE('',#19775,#18657,#11582,.T.);
#26445=EDGE_CURVE('',#19774,#18658,#11583,.T.);
#26446=EDGE_CURVE('',#19773,#18659,#11584,.T.);
#26447=EDGE_CURVE('',#19765,#18648,#11585,.T.);
#26448=EDGE_CURVE('',#19766,#18649,#11586,.T.);
#26449=EDGE_CURVE('',#19764,#18650,#11587,.T.);
#26450=EDGE_CURVE('',#19769,#18651,#11588,.T.);
#26451=EDGE_CURVE('',#19768,#18652,#11589,.T.);
#26452=EDGE_CURVE('',#19767,#18653,#11590,.T.);
#26453=EDGE_CURVE('',#19759,#18642,#11591,.T.);
#26454=EDGE_CURVE('',#19760,#18643,#11592,.T.);
#26455=EDGE_CURVE('',#19758,#18644,#11593,.T.);
#26456=EDGE_CURVE('',#19763,#18645,#11594,.T.);
#26457=EDGE_CURVE('',#19762,#18646,#11595,.T.);
#26458=EDGE_CURVE('',#19761,#18647,#11596,.T.);
#26459=EDGE_CURVE('',#19753,#18636,#11597,.T.);
#26460=EDGE_CURVE('',#19754,#18637,#11598,.T.);
#26461=EDGE_CURVE('',#19752,#18638,#11599,.T.);
#26462=EDGE_CURVE('',#19757,#18639,#11600,.T.);
#26463=EDGE_CURVE('',#19756,#18640,#11601,.T.);
#26464=EDGE_CURVE('',#19755,#18641,#11602,.T.);
#26465=EDGE_CURVE('',#19747,#18630,#11603,.T.);
#26466=EDGE_CURVE('',#19748,#18631,#11604,.T.);
#26467=EDGE_CURVE('',#19746,#18632,#11605,.T.);
#26468=EDGE_CURVE('',#19751,#18633,#11606,.T.);
#26469=EDGE_CURVE('',#19750,#18634,#11607,.T.);
#26470=EDGE_CURVE('',#19749,#18635,#11608,.T.);
#26471=EDGE_CURVE('',#19741,#18624,#11609,.T.);
#26472=EDGE_CURVE('',#19742,#18625,#11610,.T.);
#26473=EDGE_CURVE('',#19740,#18626,#11611,.T.);
#26474=EDGE_CURVE('',#19745,#18627,#11612,.T.);
#26475=EDGE_CURVE('',#19744,#18628,#11613,.T.);
#26476=EDGE_CURVE('',#19743,#18629,#11614,.T.);
#26477=ORIENTED_EDGE('',*,*,#20856,.F.);
#26478=ORIENTED_EDGE('',*,*,#20857,.T.);
#26479=ORIENTED_EDGE('',*,*,#20858,.T.);
#26480=ORIENTED_EDGE('',*,*,#20857,.F.);
#26481=ORIENTED_EDGE('',*,*,#20859,.F.);
#26482=ORIENTED_EDGE('',*,*,#20860,.T.);
#26483=ORIENTED_EDGE('',*,*,#20861,.T.);
#26484=ORIENTED_EDGE('',*,*,#20860,.F.);
#26485=ORIENTED_EDGE('',*,*,#20862,.F.);
#26486=ORIENTED_EDGE('',*,*,#20863,.T.);
#26487=ORIENTED_EDGE('',*,*,#20864,.T.);
#26488=ORIENTED_EDGE('',*,*,#20863,.F.);
#26489=ORIENTED_EDGE('',*,*,#20865,.F.);
#26490=ORIENTED_EDGE('',*,*,#20866,.T.);
#26491=ORIENTED_EDGE('',*,*,#20867,.T.);
#26492=ORIENTED_EDGE('',*,*,#20866,.F.);
#26493=ORIENTED_EDGE('',*,*,#20868,.F.);
#26494=ORIENTED_EDGE('',*,*,#20869,.T.);
#26495=ORIENTED_EDGE('',*,*,#20870,.T.);
#26496=ORIENTED_EDGE('',*,*,#20869,.F.);
#26497=ORIENTED_EDGE('',*,*,#20871,.T.);
#26498=ORIENTED_EDGE('',*,*,#20872,.T.);
#26499=ORIENTED_EDGE('',*,*,#20873,.F.);
#26500=ORIENTED_EDGE('',*,*,#20872,.F.);
#26501=ORIENTED_EDGE('',*,*,#20874,.F.);
#26502=ORIENTED_EDGE('',*,*,#20875,.T.);
#26503=ORIENTED_EDGE('',*,*,#20876,.T.);
#26504=ORIENTED_EDGE('',*,*,#20877,.F.);
#26505=ORIENTED_EDGE('',*,*,#20878,.T.);
#26506=ORIENTED_EDGE('',*,*,#20879,.T.);
#26507=ORIENTED_EDGE('',*,*,#20880,.F.);
#26508=ORIENTED_EDGE('',*,*,#20881,.F.);
#26509=ORIENTED_EDGE('',*,*,#20882,.T.);
#26510=ORIENTED_EDGE('',*,*,#20883,.T.);
#26511=ORIENTED_EDGE('',*,*,#20884,.F.);
#26512=ORIENTED_EDGE('',*,*,#20885,.F.);
#26513=ORIENTED_EDGE('',*,*,#20886,.T.);
#26514=ORIENTED_EDGE('',*,*,#20887,.T.);
#26515=ORIENTED_EDGE('',*,*,#20888,.F.);
#26516=ORIENTED_EDGE('',*,*,#20889,.F.);
#26517=ORIENTED_EDGE('',*,*,#20890,.T.);
#26518=ORIENTED_EDGE('',*,*,#20891,.T.);
#26519=ORIENTED_EDGE('',*,*,#20892,.F.);
#26520=ORIENTED_EDGE('',*,*,#20893,.F.);
#26521=ORIENTED_EDGE('',*,*,#20894,.T.);
#26522=ORIENTED_EDGE('',*,*,#20895,.T.);
#26523=ORIENTED_EDGE('',*,*,#20896,.F.);
#26524=ORIENTED_EDGE('',*,*,#20897,.F.);
#26525=ORIENTED_EDGE('',*,*,#20898,.F.);
#26526=ORIENTED_EDGE('',*,*,#20899,.T.);
#26527=ORIENTED_EDGE('',*,*,#20900,.T.);
#26528=ORIENTED_EDGE('',*,*,#20901,.F.);
#26529=ORIENTED_EDGE('',*,*,#20902,.F.);
#26530=ORIENTED_EDGE('',*,*,#20903,.T.);
#26531=ORIENTED_EDGE('',*,*,#20904,.T.);
#26532=ORIENTED_EDGE('',*,*,#20905,.F.);
#26533=ORIENTED_EDGE('',*,*,#20906,.F.);
#26534=ORIENTED_EDGE('',*,*,#20907,.T.);
#26535=ORIENTED_EDGE('',*,*,#20908,.T.);
#26536=ORIENTED_EDGE('',*,*,#20909,.F.);
#26537=ORIENTED_EDGE('',*,*,#20910,.F.);
#26538=ORIENTED_EDGE('',*,*,#20911,.T.);
#26539=ORIENTED_EDGE('',*,*,#20912,.T.);
#26540=ORIENTED_EDGE('',*,*,#20913,.F.);
#26541=ORIENTED_EDGE('',*,*,#20914,.F.);
#26542=ORIENTED_EDGE('',*,*,#20915,.T.);
#26543=ORIENTED_EDGE('',*,*,#20916,.T.);
#26544=ORIENTED_EDGE('',*,*,#20917,.F.);
#26545=ORIENTED_EDGE('',*,*,#20918,.F.);
#26546=ORIENTED_EDGE('',*,*,#20919,.T.);
#26547=ORIENTED_EDGE('',*,*,#20920,.T.);
#26548=ORIENTED_EDGE('',*,*,#20921,.F.);
#26549=ORIENTED_EDGE('',*,*,#20922,.F.);
#26550=ORIENTED_EDGE('',*,*,#20923,.T.);
#26551=ORIENTED_EDGE('',*,*,#20924,.T.);
#26552=ORIENTED_EDGE('',*,*,#20925,.F.);
#26553=ORIENTED_EDGE('',*,*,#20926,.T.);
#26554=ORIENTED_EDGE('',*,*,#20927,.T.);
#26555=ORIENTED_EDGE('',*,*,#20928,.F.);
#26556=ORIENTED_EDGE('',*,*,#20929,.F.);
#26557=ORIENTED_EDGE('',*,*,#20930,.T.);
#26558=ORIENTED_EDGE('',*,*,#20931,.T.);
#26559=ORIENTED_EDGE('',*,*,#20932,.F.);
#26560=ORIENTED_EDGE('',*,*,#20933,.F.);
#26561=ORIENTED_EDGE('',*,*,#20934,.T.);
#26562=ORIENTED_EDGE('',*,*,#20935,.T.);
#26563=ORIENTED_EDGE('',*,*,#20936,.F.);
#26564=ORIENTED_EDGE('',*,*,#20937,.F.);
#26565=ORIENTED_EDGE('',*,*,#20938,.T.);
#26566=ORIENTED_EDGE('',*,*,#20939,.T.);
#26567=ORIENTED_EDGE('',*,*,#20940,.F.);
#26568=ORIENTED_EDGE('',*,*,#20941,.F.);
#26569=ORIENTED_EDGE('',*,*,#20942,.F.);
#26570=ORIENTED_EDGE('',*,*,#20943,.T.);
#26571=ORIENTED_EDGE('',*,*,#20944,.T.);
#26572=ORIENTED_EDGE('',*,*,#20945,.F.);
#26573=ORIENTED_EDGE('',*,*,#20946,.F.);
#26574=ORIENTED_EDGE('',*,*,#20947,.T.);
#26575=ORIENTED_EDGE('',*,*,#20948,.T.);
#26576=ORIENTED_EDGE('',*,*,#20949,.F.);
#26577=ORIENTED_EDGE('',*,*,#20950,.T.);
#26578=ORIENTED_EDGE('',*,*,#20951,.T.);
#26579=ORIENTED_EDGE('',*,*,#20952,.F.);
#26580=ORIENTED_EDGE('',*,*,#20953,.F.);
#26581=ORIENTED_EDGE('',*,*,#20954,.F.);
#26582=ORIENTED_EDGE('',*,*,#20955,.T.);
#26583=ORIENTED_EDGE('',*,*,#20956,.T.);
#26584=ORIENTED_EDGE('',*,*,#20957,.F.);
#26585=ORIENTED_EDGE('',*,*,#20958,.T.);
#26586=ORIENTED_EDGE('',*,*,#20959,.T.);
#26587=ORIENTED_EDGE('',*,*,#20960,.F.);
#26588=ORIENTED_EDGE('',*,*,#20961,.F.);
#26589=ORIENTED_EDGE('',*,*,#20962,.T.);
#26590=ORIENTED_EDGE('',*,*,#20963,.T.);
#26591=ORIENTED_EDGE('',*,*,#20964,.F.);
#26592=ORIENTED_EDGE('',*,*,#20965,.F.);
#26593=ORIENTED_EDGE('',*,*,#20966,.F.);
#26594=ORIENTED_EDGE('',*,*,#20967,.T.);
#26595=ORIENTED_EDGE('',*,*,#20968,.T.);
#26596=ORIENTED_EDGE('',*,*,#20969,.F.);
#26597=ORIENTED_EDGE('',*,*,#20970,.T.);
#26598=ORIENTED_EDGE('',*,*,#20971,.T.);
#26599=ORIENTED_EDGE('',*,*,#20972,.F.);
#26600=ORIENTED_EDGE('',*,*,#20973,.F.);
#26601=ORIENTED_EDGE('',*,*,#20974,.F.);
#26602=ORIENTED_EDGE('',*,*,#20975,.T.);
#26603=ORIENTED_EDGE('',*,*,#20976,.T.);
#26604=ORIENTED_EDGE('',*,*,#20977,.F.);
#26605=ORIENTED_EDGE('',*,*,#20978,.F.);
#26606=ORIENTED_EDGE('',*,*,#20979,.T.);
#26607=ORIENTED_EDGE('',*,*,#20980,.T.);
#26608=ORIENTED_EDGE('',*,*,#20981,.F.);
#26609=ORIENTED_EDGE('',*,*,#20982,.F.);
#26610=ORIENTED_EDGE('',*,*,#20983,.T.);
#26611=ORIENTED_EDGE('',*,*,#20984,.T.);
#26612=ORIENTED_EDGE('',*,*,#20985,.F.);
#26613=ORIENTED_EDGE('',*,*,#20986,.F.);
#26614=ORIENTED_EDGE('',*,*,#20987,.T.);
#26615=ORIENTED_EDGE('',*,*,#20988,.T.);
#26616=ORIENTED_EDGE('',*,*,#20989,.F.);
#26617=ORIENTED_EDGE('',*,*,#20990,.F.);
#26618=ORIENTED_EDGE('',*,*,#20991,.T.);
#26619=ORIENTED_EDGE('',*,*,#20992,.T.);
#26620=ORIENTED_EDGE('',*,*,#20993,.F.);
#26621=ORIENTED_EDGE('',*,*,#20994,.T.);
#26622=ORIENTED_EDGE('',*,*,#20995,.T.);
#26623=ORIENTED_EDGE('',*,*,#20996,.F.);
#26624=ORIENTED_EDGE('',*,*,#20997,.F.);
#26625=ORIENTED_EDGE('',*,*,#20998,.T.);
#26626=ORIENTED_EDGE('',*,*,#20999,.T.);
#26627=ORIENTED_EDGE('',*,*,#21000,.F.);
#26628=ORIENTED_EDGE('',*,*,#21001,.F.);
#26629=ORIENTED_EDGE('',*,*,#21002,.T.);
#26630=ORIENTED_EDGE('',*,*,#21003,.T.);
#26631=ORIENTED_EDGE('',*,*,#21004,.F.);
#26632=ORIENTED_EDGE('',*,*,#21005,.F.);
#26633=ORIENTED_EDGE('',*,*,#21006,.T.);
#26634=ORIENTED_EDGE('',*,*,#21007,.T.);
#26635=ORIENTED_EDGE('',*,*,#21008,.F.);
#26636=ORIENTED_EDGE('',*,*,#21009,.F.);
#26637=ORIENTED_EDGE('',*,*,#21010,.T.);
#26638=ORIENTED_EDGE('',*,*,#21011,.T.);
#26639=ORIENTED_EDGE('',*,*,#21012,.F.);
#26640=ORIENTED_EDGE('',*,*,#21013,.F.);
#26641=ORIENTED_EDGE('',*,*,#21014,.T.);
#26642=ORIENTED_EDGE('',*,*,#21015,.T.);
#26643=ORIENTED_EDGE('',*,*,#21016,.F.);
#26644=ORIENTED_EDGE('',*,*,#21017,.F.);
#26645=ORIENTED_EDGE('',*,*,#21018,.T.);
#26646=ORIENTED_EDGE('',*,*,#21019,.T.);
#26647=ORIENTED_EDGE('',*,*,#21020,.F.);
#26648=ORIENTED_EDGE('',*,*,#21021,.F.);
#26649=ORIENTED_EDGE('',*,*,#21022,.F.);
#26650=ORIENTED_EDGE('',*,*,#21023,.T.);
#26651=ORIENTED_EDGE('',*,*,#21024,.T.);
#26652=ORIENTED_EDGE('',*,*,#21025,.F.);
#26653=ORIENTED_EDGE('',*,*,#21026,.F.);
#26654=ORIENTED_EDGE('',*,*,#21027,.T.);
#26655=ORIENTED_EDGE('',*,*,#21028,.T.);
#26656=ORIENTED_EDGE('',*,*,#21029,.F.);
#26657=ORIENTED_EDGE('',*,*,#21030,.F.);
#26658=ORIENTED_EDGE('',*,*,#21031,.T.);
#26659=ORIENTED_EDGE('',*,*,#21032,.T.);
#26660=ORIENTED_EDGE('',*,*,#21033,.F.);
#26661=ORIENTED_EDGE('',*,*,#21034,.F.);
#26662=ORIENTED_EDGE('',*,*,#21035,.T.);
#26663=ORIENTED_EDGE('',*,*,#21036,.T.);
#26664=ORIENTED_EDGE('',*,*,#21037,.F.);
#26665=ORIENTED_EDGE('',*,*,#21038,.T.);
#26666=ORIENTED_EDGE('',*,*,#21039,.T.);
#26667=ORIENTED_EDGE('',*,*,#21040,.F.);
#26668=ORIENTED_EDGE('',*,*,#21041,.F.);
#26669=ORIENTED_EDGE('',*,*,#21042,.T.);
#26670=ORIENTED_EDGE('',*,*,#21043,.T.);
#26671=ORIENTED_EDGE('',*,*,#21044,.F.);
#26672=ORIENTED_EDGE('',*,*,#21045,.F.);
#26673=ORIENTED_EDGE('',*,*,#21046,.F.);
#26674=ORIENTED_EDGE('',*,*,#21047,.T.);
#26675=ORIENTED_EDGE('',*,*,#21048,.T.);
#26676=ORIENTED_EDGE('',*,*,#21049,.F.);
#26677=ORIENTED_EDGE('',*,*,#21050,.T.);
#26678=ORIENTED_EDGE('',*,*,#21051,.T.);
#26679=ORIENTED_EDGE('',*,*,#21052,.F.);
#26680=ORIENTED_EDGE('',*,*,#21053,.F.);
#26681=ORIENTED_EDGE('',*,*,#21054,.F.);
#26682=ORIENTED_EDGE('',*,*,#21055,.T.);
#26683=ORIENTED_EDGE('',*,*,#21056,.T.);
#26684=ORIENTED_EDGE('',*,*,#21057,.F.);
#26685=ORIENTED_EDGE('',*,*,#21058,.F.);
#26686=ORIENTED_EDGE('',*,*,#21059,.T.);
#26687=ORIENTED_EDGE('',*,*,#21060,.T.);
#26688=ORIENTED_EDGE('',*,*,#21061,.F.);
#26689=ORIENTED_EDGE('',*,*,#21062,.T.);
#26690=ORIENTED_EDGE('',*,*,#21063,.T.);
#26691=ORIENTED_EDGE('',*,*,#21064,.F.);
#26692=ORIENTED_EDGE('',*,*,#21065,.F.);
#26693=ORIENTED_EDGE('',*,*,#21066,.F.);
#26694=ORIENTED_EDGE('',*,*,#21067,.F.);
#26695=ORIENTED_EDGE('',*,*,#21068,.F.);
#26696=ORIENTED_EDGE('',*,*,#21069,.F.);
#26697=ORIENTED_EDGE('',*,*,#21070,.F.);
#26698=ORIENTED_EDGE('',*,*,#21071,.F.);
#26699=ORIENTED_EDGE('',*,*,#21072,.F.);
#26700=ORIENTED_EDGE('',*,*,#21073,.F.);
#26701=ORIENTED_EDGE('',*,*,#21074,.F.);
#26702=ORIENTED_EDGE('',*,*,#21075,.F.);
#26703=ORIENTED_EDGE('',*,*,#21076,.F.);
#26704=ORIENTED_EDGE('',*,*,#21077,.F.);
#26705=ORIENTED_EDGE('',*,*,#21078,.F.);
#26706=ORIENTED_EDGE('',*,*,#21079,.F.);
#26707=ORIENTED_EDGE('',*,*,#21080,.F.);
#26708=ORIENTED_EDGE('',*,*,#21081,.F.);
#26709=ORIENTED_EDGE('',*,*,#21082,.F.);
#26710=ORIENTED_EDGE('',*,*,#21083,.F.);
#26711=ORIENTED_EDGE('',*,*,#21084,.F.);
#26712=ORIENTED_EDGE('',*,*,#21085,.F.);
#26713=ORIENTED_EDGE('',*,*,#21086,.F.);
#26714=ORIENTED_EDGE('',*,*,#21087,.F.);
#26715=ORIENTED_EDGE('',*,*,#21088,.F.);
#26716=ORIENTED_EDGE('',*,*,#21089,.F.);
#26717=ORIENTED_EDGE('',*,*,#21090,.F.);
#26718=ORIENTED_EDGE('',*,*,#21091,.F.);
#26719=ORIENTED_EDGE('',*,*,#21092,.F.);
#26720=ORIENTED_EDGE('',*,*,#21093,.F.);
#26721=ORIENTED_EDGE('',*,*,#21094,.F.);
#26722=ORIENTED_EDGE('',*,*,#21095,.F.);
#26723=ORIENTED_EDGE('',*,*,#21096,.F.);
#26724=ORIENTED_EDGE('',*,*,#21097,.F.);
#26725=ORIENTED_EDGE('',*,*,#21098,.F.);
#26726=ORIENTED_EDGE('',*,*,#21099,.F.);
#26727=ORIENTED_EDGE('',*,*,#21100,.F.);
#26728=ORIENTED_EDGE('',*,*,#21101,.F.);
#26729=ORIENTED_EDGE('',*,*,#21102,.F.);
#26730=ORIENTED_EDGE('',*,*,#21103,.F.);
#26731=ORIENTED_EDGE('',*,*,#21104,.F.);
#26732=ORIENTED_EDGE('',*,*,#21105,.F.);
#26733=ORIENTED_EDGE('',*,*,#21106,.F.);
#26734=ORIENTED_EDGE('',*,*,#21107,.F.);
#26735=ORIENTED_EDGE('',*,*,#21108,.F.);
#26736=ORIENTED_EDGE('',*,*,#21109,.F.);
#26737=ORIENTED_EDGE('',*,*,#21110,.F.);
#26738=ORIENTED_EDGE('',*,*,#21111,.F.);
#26739=ORIENTED_EDGE('',*,*,#21112,.F.);
#26740=ORIENTED_EDGE('',*,*,#21113,.F.);
#26741=ORIENTED_EDGE('',*,*,#21114,.F.);
#26742=ORIENTED_EDGE('',*,*,#21115,.F.);
#26743=ORIENTED_EDGE('',*,*,#21116,.F.);
#26744=ORIENTED_EDGE('',*,*,#21117,.F.);
#26745=ORIENTED_EDGE('',*,*,#21118,.F.);
#26746=ORIENTED_EDGE('',*,*,#21119,.F.);
#26747=ORIENTED_EDGE('',*,*,#21120,.F.);
#26748=ORIENTED_EDGE('',*,*,#21121,.F.);
#26749=ORIENTED_EDGE('',*,*,#21122,.F.);
#26750=ORIENTED_EDGE('',*,*,#21123,.F.);
#26751=ORIENTED_EDGE('',*,*,#21124,.F.);
#26752=ORIENTED_EDGE('',*,*,#21125,.F.);
#26753=ORIENTED_EDGE('',*,*,#21126,.F.);
#26754=ORIENTED_EDGE('',*,*,#21127,.F.);
#26755=ORIENTED_EDGE('',*,*,#21128,.F.);
#26756=ORIENTED_EDGE('',*,*,#21129,.F.);
#26757=ORIENTED_EDGE('',*,*,#21130,.F.);
#26758=ORIENTED_EDGE('',*,*,#21131,.F.);
#26759=ORIENTED_EDGE('',*,*,#21132,.F.);
#26760=ORIENTED_EDGE('',*,*,#21133,.F.);
#26761=ORIENTED_EDGE('',*,*,#21134,.F.);
#26762=ORIENTED_EDGE('',*,*,#21135,.F.);
#26763=ORIENTED_EDGE('',*,*,#21136,.F.);
#26764=ORIENTED_EDGE('',*,*,#21137,.F.);
#26765=ORIENTED_EDGE('',*,*,#21138,.F.);
#26766=ORIENTED_EDGE('',*,*,#21139,.T.);
#26767=ORIENTED_EDGE('',*,*,#21140,.F.);
#26768=ORIENTED_EDGE('',*,*,#21141,.T.);
#26769=ORIENTED_EDGE('',*,*,#21142,.F.);
#26770=ORIENTED_EDGE('',*,*,#21143,.T.);
#26771=ORIENTED_EDGE('',*,*,#21144,.F.);
#26772=ORIENTED_EDGE('',*,*,#21145,.T.);
#26773=ORIENTED_EDGE('',*,*,#21146,.T.);
#26774=ORIENTED_EDGE('',*,*,#21147,.T.);
#26775=ORIENTED_EDGE('',*,*,#21148,.F.);
#26776=ORIENTED_EDGE('',*,*,#21149,.T.);
#26777=ORIENTED_EDGE('',*,*,#21150,.F.);
#26778=ORIENTED_EDGE('',*,*,#21151,.T.);
#26779=ORIENTED_EDGE('',*,*,#21152,.F.);
#26780=ORIENTED_EDGE('',*,*,#21153,.T.);
#26781=ORIENTED_EDGE('',*,*,#21154,.T.);
#26782=ORIENTED_EDGE('',*,*,#21155,.T.);
#26783=ORIENTED_EDGE('',*,*,#21156,.F.);
#26784=ORIENTED_EDGE('',*,*,#21157,.T.);
#26785=ORIENTED_EDGE('',*,*,#21158,.T.);
#26786=ORIENTED_EDGE('',*,*,#21159,.T.);
#26787=ORIENTED_EDGE('',*,*,#21160,.F.);
#26788=ORIENTED_EDGE('',*,*,#21159,.F.);
#26789=ORIENTED_EDGE('',*,*,#21161,.F.);
#26790=ORIENTED_EDGE('',*,*,#21162,.T.);
#26791=ORIENTED_EDGE('',*,*,#21163,.T.);
#26792=ORIENTED_EDGE('',*,*,#21162,.F.);
#26793=ORIENTED_EDGE('',*,*,#21164,.T.);
#26794=ORIENTED_EDGE('',*,*,#21165,.T.);
#26795=ORIENTED_EDGE('',*,*,#21166,.F.);
#26796=ORIENTED_EDGE('',*,*,#21165,.F.);
#26797=ORIENTED_EDGE('',*,*,#21167,.F.);
#26798=ORIENTED_EDGE('',*,*,#21168,.T.);
#26799=ORIENTED_EDGE('',*,*,#21169,.T.);
#26800=ORIENTED_EDGE('',*,*,#21168,.F.);
#26801=ORIENTED_EDGE('',*,*,#21170,.F.);
#26802=ORIENTED_EDGE('',*,*,#21171,.T.);
#26803=ORIENTED_EDGE('',*,*,#21172,.T.);
#26804=ORIENTED_EDGE('',*,*,#21171,.F.);
#26805=ORIENTED_EDGE('',*,*,#21173,.F.);
#26806=ORIENTED_EDGE('',*,*,#21174,.T.);
#26807=ORIENTED_EDGE('',*,*,#21175,.T.);
#26808=ORIENTED_EDGE('',*,*,#21174,.F.);
#26809=ORIENTED_EDGE('',*,*,#21176,.F.);
#26810=ORIENTED_EDGE('',*,*,#21177,.T.);
#26811=ORIENTED_EDGE('',*,*,#21173,.T.);
#26812=ORIENTED_EDGE('',*,*,#21177,.F.);
#26813=ORIENTED_EDGE('',*,*,#21178,.T.);
#26814=ORIENTED_EDGE('',*,*,#21179,.T.);
#26815=ORIENTED_EDGE('',*,*,#21170,.T.);
#26816=ORIENTED_EDGE('',*,*,#21179,.F.);
#26817=ORIENTED_EDGE('',*,*,#21180,.T.);
#26818=ORIENTED_EDGE('',*,*,#21181,.T.);
#26819=ORIENTED_EDGE('',*,*,#21182,.F.);
#26820=ORIENTED_EDGE('',*,*,#21181,.F.);
#26821=ORIENTED_EDGE('',*,*,#21183,.T.);
#26822=ORIENTED_EDGE('',*,*,#21184,.T.);
#26823=ORIENTED_EDGE('',*,*,#21185,.F.);
#26824=ORIENTED_EDGE('',*,*,#21184,.F.);
#26825=ORIENTED_EDGE('',*,*,#21186,.T.);
#26826=ORIENTED_EDGE('',*,*,#21187,.T.);
#26827=ORIENTED_EDGE('',*,*,#21188,.F.);
#26828=ORIENTED_EDGE('',*,*,#21187,.F.);
#26829=ORIENTED_EDGE('',*,*,#21189,.T.);
#26830=ORIENTED_EDGE('',*,*,#21190,.T.);
#26831=ORIENTED_EDGE('',*,*,#21191,.F.);
#26832=ORIENTED_EDGE('',*,*,#21190,.F.);
#26833=ORIENTED_EDGE('',*,*,#21192,.T.);
#26834=ORIENTED_EDGE('',*,*,#21193,.T.);
#26835=ORIENTED_EDGE('',*,*,#21194,.F.);
#26836=ORIENTED_EDGE('',*,*,#21195,.T.);
#26837=ORIENTED_EDGE('',*,*,#21196,.F.);
#26838=ORIENTED_EDGE('',*,*,#21197,.T.);
#26839=ORIENTED_EDGE('',*,*,#21198,.F.);
#26840=ORIENTED_EDGE('',*,*,#21199,.F.);
#26841=ORIENTED_EDGE('',*,*,#21200,.F.);
#26842=ORIENTED_EDGE('',*,*,#21201,.F.);
#26843=ORIENTED_EDGE('',*,*,#21202,.F.);
#26844=ORIENTED_EDGE('',*,*,#21203,.F.);
#26845=ORIENTED_EDGE('',*,*,#21204,.F.);
#26846=ORIENTED_EDGE('',*,*,#21205,.F.);
#26847=ORIENTED_EDGE('',*,*,#21206,.F.);
#26848=ORIENTED_EDGE('',*,*,#21207,.F.);
#26849=ORIENTED_EDGE('',*,*,#21208,.F.);
#26850=ORIENTED_EDGE('',*,*,#21209,.F.);
#26851=ORIENTED_EDGE('',*,*,#21210,.F.);
#26852=ORIENTED_EDGE('',*,*,#21211,.F.);
#26853=ORIENTED_EDGE('',*,*,#21212,.F.);
#26854=ORIENTED_EDGE('',*,*,#21213,.F.);
#26855=ORIENTED_EDGE('',*,*,#21214,.T.);
#26856=ORIENTED_EDGE('',*,*,#21215,.F.);
#26857=ORIENTED_EDGE('',*,*,#21216,.F.);
#26858=ORIENTED_EDGE('',*,*,#21217,.T.);
#26859=ORIENTED_EDGE('',*,*,#21218,.F.);
#26860=ORIENTED_EDGE('',*,*,#21219,.F.);
#26861=ORIENTED_EDGE('',*,*,#21220,.F.);
#26862=ORIENTED_EDGE('',*,*,#21221,.F.);
#26863=ORIENTED_EDGE('',*,*,#21222,.F.);
#26864=ORIENTED_EDGE('',*,*,#21223,.F.);
#26865=ORIENTED_EDGE('',*,*,#21224,.F.);
#26866=ORIENTED_EDGE('',*,*,#21225,.T.);
#26867=ORIENTED_EDGE('',*,*,#21226,.F.);
#26868=ORIENTED_EDGE('',*,*,#21227,.T.);
#26869=ORIENTED_EDGE('',*,*,#21228,.F.);
#26870=ORIENTED_EDGE('',*,*,#21229,.F.);
#26871=ORIENTED_EDGE('',*,*,#21230,.F.);
#26872=ORIENTED_EDGE('',*,*,#21231,.T.);
#26873=ORIENTED_EDGE('',*,*,#21232,.F.);
#26874=ORIENTED_EDGE('',*,*,#21233,.T.);
#26875=ORIENTED_EDGE('',*,*,#21234,.F.);
#26876=ORIENTED_EDGE('',*,*,#21235,.T.);
#26877=ORIENTED_EDGE('',*,*,#21236,.F.);
#26878=ORIENTED_EDGE('',*,*,#21237,.F.);
#26879=ORIENTED_EDGE('',*,*,#21238,.F.);
#26880=ORIENTED_EDGE('',*,*,#21239,.T.);
#26881=ORIENTED_EDGE('',*,*,#21240,.F.);
#26882=ORIENTED_EDGE('',*,*,#21241,.T.);
#26883=ORIENTED_EDGE('',*,*,#21242,.F.);
#26884=ORIENTED_EDGE('',*,*,#21243,.T.);
#26885=ORIENTED_EDGE('',*,*,#21244,.F.);
#26886=ORIENTED_EDGE('',*,*,#21245,.F.);
#26887=ORIENTED_EDGE('',*,*,#21246,.F.);
#26888=ORIENTED_EDGE('',*,*,#21247,.T.);
#26889=ORIENTED_EDGE('',*,*,#21248,.F.);
#26890=ORIENTED_EDGE('',*,*,#21249,.T.);
#26891=ORIENTED_EDGE('',*,*,#21250,.F.);
#26892=ORIENTED_EDGE('',*,*,#21251,.T.);
#26893=ORIENTED_EDGE('',*,*,#21252,.F.);
#26894=ORIENTED_EDGE('',*,*,#21253,.F.);
#26895=ORIENTED_EDGE('',*,*,#21254,.F.);
#26896=ORIENTED_EDGE('',*,*,#21255,.T.);
#26897=ORIENTED_EDGE('',*,*,#21256,.F.);
#26898=ORIENTED_EDGE('',*,*,#21257,.T.);
#26899=ORIENTED_EDGE('',*,*,#21258,.T.);
#26900=ORIENTED_EDGE('',*,*,#21259,.T.);
#26901=ORIENTED_EDGE('',*,*,#21260,.T.);
#26902=ORIENTED_EDGE('',*,*,#21261,.T.);
#26903=ORIENTED_EDGE('',*,*,#21262,.T.);
#26904=ORIENTED_EDGE('',*,*,#21263,.T.);
#26905=ORIENTED_EDGE('',*,*,#21264,.F.);
#26906=ORIENTED_EDGE('',*,*,#21265,.F.);
#26907=ORIENTED_EDGE('',*,*,#21266,.F.);
#26908=ORIENTED_EDGE('',*,*,#21267,.F.);
#26909=ORIENTED_EDGE('',*,*,#21268,.F.);
#26910=ORIENTED_EDGE('',*,*,#21269,.F.);
#26911=ORIENTED_EDGE('',*,*,#21270,.T.);
#26912=ORIENTED_EDGE('',*,*,#21271,.T.);
#26913=ORIENTED_EDGE('',*,*,#21272,.T.);
#26914=ORIENTED_EDGE('',*,*,#21273,.T.);
#26915=ORIENTED_EDGE('',*,*,#21274,.T.);
#26916=ORIENTED_EDGE('',*,*,#21275,.T.);
#26917=ORIENTED_EDGE('',*,*,#21276,.T.);
#26918=ORIENTED_EDGE('',*,*,#21277,.T.);
#26919=ORIENTED_EDGE('',*,*,#21278,.T.);
#26920=ORIENTED_EDGE('',*,*,#21279,.F.);
#26921=ORIENTED_EDGE('',*,*,#21280,.F.);
#26922=ORIENTED_EDGE('',*,*,#21281,.T.);
#26923=ORIENTED_EDGE('',*,*,#21282,.F.);
#26924=ORIENTED_EDGE('',*,*,#21283,.F.);
#26925=ORIENTED_EDGE('',*,*,#21284,.F.);
#26926=ORIENTED_EDGE('',*,*,#21285,.F.);
#26927=ORIENTED_EDGE('',*,*,#21286,.T.);
#26928=ORIENTED_EDGE('',*,*,#21287,.F.);
#26929=ORIENTED_EDGE('',*,*,#21288,.F.);
#26930=ORIENTED_EDGE('',*,*,#21289,.F.);
#26931=ORIENTED_EDGE('',*,*,#21290,.T.);
#26932=ORIENTED_EDGE('',*,*,#21291,.F.);
#26933=ORIENTED_EDGE('',*,*,#21292,.F.);
#26934=ORIENTED_EDGE('',*,*,#21293,.F.);
#26935=ORIENTED_EDGE('',*,*,#21294,.T.);
#26936=ORIENTED_EDGE('',*,*,#21295,.F.);
#26937=ORIENTED_EDGE('',*,*,#21296,.F.);
#26938=ORIENTED_EDGE('',*,*,#21297,.F.);
#26939=ORIENTED_EDGE('',*,*,#21298,.T.);
#26940=ORIENTED_EDGE('',*,*,#21299,.F.);
#26941=ORIENTED_EDGE('',*,*,#21197,.F.);
#26942=ORIENTED_EDGE('',*,*,#21300,.T.);
#26943=ORIENTED_EDGE('',*,*,#21256,.T.);
#26944=ORIENTED_EDGE('',*,*,#21301,.F.);
#26945=ORIENTED_EDGE('',*,*,#21264,.T.);
#26946=ORIENTED_EDGE('',*,*,#21302,.F.);
#26947=ORIENTED_EDGE('',*,*,#21217,.F.);
#26948=ORIENTED_EDGE('',*,*,#21303,.F.);
#26949=ORIENTED_EDGE('',*,*,#21304,.F.);
#26950=ORIENTED_EDGE('',*,*,#21305,.F.);
#26951=ORIENTED_EDGE('',*,*,#21306,.F.);
#26952=ORIENTED_EDGE('',*,*,#21307,.F.);
#26953=ORIENTED_EDGE('',*,*,#21308,.F.);
#26954=ORIENTED_EDGE('',*,*,#21309,.F.);
#26955=ORIENTED_EDGE('',*,*,#21310,.T.);
#26956=ORIENTED_EDGE('',*,*,#21311,.T.);
#26957=ORIENTED_EDGE('',*,*,#21312,.F.);
#26958=ORIENTED_EDGE('',*,*,#21313,.T.);
#26959=ORIENTED_EDGE('',*,*,#21314,.T.);
#26960=ORIENTED_EDGE('',*,*,#21315,.T.);
#26961=ORIENTED_EDGE('',*,*,#21316,.T.);
#26962=ORIENTED_EDGE('',*,*,#21317,.T.);
#26963=ORIENTED_EDGE('',*,*,#21318,.F.);
#26964=ORIENTED_EDGE('',*,*,#21319,.T.);
#26965=ORIENTED_EDGE('',*,*,#21320,.F.);
#26966=ORIENTED_EDGE('',*,*,#21321,.T.);
#26967=ORIENTED_EDGE('',*,*,#21322,.F.);
#26968=ORIENTED_EDGE('',*,*,#21323,.T.);
#26969=ORIENTED_EDGE('',*,*,#21324,.T.);
#26970=ORIENTED_EDGE('',*,*,#21325,.T.);
#26971=ORIENTED_EDGE('',*,*,#21326,.F.);
#26972=ORIENTED_EDGE('',*,*,#21327,.T.);
#26973=ORIENTED_EDGE('',*,*,#21328,.T.);
#26974=ORIENTED_EDGE('',*,*,#21329,.T.);
#26975=ORIENTED_EDGE('',*,*,#21330,.T.);
#26976=ORIENTED_EDGE('',*,*,#21331,.T.);
#26977=ORIENTED_EDGE('',*,*,#21332,.F.);
#26978=ORIENTED_EDGE('',*,*,#21333,.F.);
#26979=ORIENTED_EDGE('',*,*,#21334,.T.);
#26980=ORIENTED_EDGE('',*,*,#21335,.F.);
#26981=ORIENTED_EDGE('',*,*,#21336,.T.);
#26982=ORIENTED_EDGE('',*,*,#21337,.T.);
#26983=ORIENTED_EDGE('',*,*,#21338,.T.);
#26984=ORIENTED_EDGE('',*,*,#21339,.F.);
#26985=ORIENTED_EDGE('',*,*,#21211,.T.);
#26986=ORIENTED_EDGE('',*,*,#21340,.T.);
#26987=ORIENTED_EDGE('',*,*,#21270,.F.);
#26988=ORIENTED_EDGE('',*,*,#21341,.F.);
#26989=ORIENTED_EDGE('',*,*,#21278,.F.);
#26990=ORIENTED_EDGE('',*,*,#21342,.F.);
#26991=ORIENTED_EDGE('',*,*,#21203,.T.);
#26992=ORIENTED_EDGE('',*,*,#21343,.F.);
#26993=ORIENTED_EDGE('',*,*,#21344,.F.);
#26994=ORIENTED_EDGE('',*,*,#21345,.T.);
#26995=ORIENTED_EDGE('',*,*,#21346,.F.);
#26996=ORIENTED_EDGE('',*,*,#21347,.T.);
#26997=ORIENTED_EDGE('',*,*,#21348,.T.);
#26998=ORIENTED_EDGE('',*,*,#21349,.F.);
#26999=ORIENTED_EDGE('',*,*,#21350,.F.);
#27000=ORIENTED_EDGE('',*,*,#21351,.T.);
#27001=ORIENTED_EDGE('',*,*,#21352,.F.);
#27002=ORIENTED_EDGE('',*,*,#21353,.F.);
#27003=ORIENTED_EDGE('',*,*,#21354,.T.);
#27004=ORIENTED_EDGE('',*,*,#21064,.T.);
#27005=ORIENTED_EDGE('',*,*,#21355,.F.);
#27006=ORIENTED_EDGE('',*,*,#21356,.T.);
#27007=ORIENTED_EDGE('',*,*,#21357,.T.);
#27008=ORIENTED_EDGE('',*,*,#21052,.T.);
#27009=ORIENTED_EDGE('',*,*,#21358,.F.);
#27010=ORIENTED_EDGE('',*,*,#21359,.T.);
#27011=ORIENTED_EDGE('',*,*,#21360,.T.);
#27012=ORIENTED_EDGE('',*,*,#21044,.T.);
#27013=ORIENTED_EDGE('',*,*,#21361,.F.);
#27014=ORIENTED_EDGE('',*,*,#21362,.T.);
#27015=ORIENTED_EDGE('',*,*,#21363,.T.);
#27016=ORIENTED_EDGE('',*,*,#21040,.T.);
#27017=ORIENTED_EDGE('',*,*,#21364,.F.);
#27018=ORIENTED_EDGE('',*,*,#21365,.T.);
#27019=ORIENTED_EDGE('',*,*,#21366,.T.);
#27020=ORIENTED_EDGE('',*,*,#21020,.T.);
#27021=ORIENTED_EDGE('',*,*,#21367,.F.);
#27022=ORIENTED_EDGE('',*,*,#21368,.T.);
#27023=ORIENTED_EDGE('',*,*,#21369,.T.);
#27024=ORIENTED_EDGE('',*,*,#21016,.T.);
#27025=ORIENTED_EDGE('',*,*,#21370,.F.);
#27026=ORIENTED_EDGE('',*,*,#21371,.T.);
#27027=ORIENTED_EDGE('',*,*,#21372,.T.);
#27028=ORIENTED_EDGE('',*,*,#21012,.T.);
#27029=ORIENTED_EDGE('',*,*,#21373,.F.);
#27030=ORIENTED_EDGE('',*,*,#21374,.T.);
#27031=ORIENTED_EDGE('',*,*,#21375,.T.);
#27032=ORIENTED_EDGE('',*,*,#21008,.T.);
#27033=ORIENTED_EDGE('',*,*,#21376,.F.);
#27034=ORIENTED_EDGE('',*,*,#21377,.T.);
#27035=ORIENTED_EDGE('',*,*,#21378,.T.);
#27036=ORIENTED_EDGE('',*,*,#21004,.T.);
#27037=ORIENTED_EDGE('',*,*,#21379,.F.);
#27038=ORIENTED_EDGE('',*,*,#21380,.T.);
#27039=ORIENTED_EDGE('',*,*,#21381,.T.);
#27040=ORIENTED_EDGE('',*,*,#21000,.T.);
#27041=ORIENTED_EDGE('',*,*,#21382,.F.);
#27042=ORIENTED_EDGE('',*,*,#21383,.T.);
#27043=ORIENTED_EDGE('',*,*,#21384,.T.);
#27044=ORIENTED_EDGE('',*,*,#20996,.T.);
#27045=ORIENTED_EDGE('',*,*,#21385,.F.);
#27046=ORIENTED_EDGE('',*,*,#21386,.T.);
#27047=ORIENTED_EDGE('',*,*,#21387,.T.);
#27048=ORIENTED_EDGE('',*,*,#20972,.T.);
#27049=ORIENTED_EDGE('',*,*,#21388,.F.);
#27050=ORIENTED_EDGE('',*,*,#21389,.T.);
#27051=ORIENTED_EDGE('',*,*,#20964,.T.);
#27052=ORIENTED_EDGE('',*,*,#21390,.T.);
#27053=ORIENTED_EDGE('',*,*,#21391,.T.);
#27054=ORIENTED_EDGE('',*,*,#21392,.F.);
#27055=ORIENTED_EDGE('',*,*,#20960,.T.);
#27056=ORIENTED_EDGE('',*,*,#21393,.T.);
#27057=ORIENTED_EDGE('',*,*,#21394,.T.);
#27058=ORIENTED_EDGE('',*,*,#21395,.F.);
#27059=ORIENTED_EDGE('',*,*,#20952,.T.);
#27060=ORIENTED_EDGE('',*,*,#21396,.T.);
#27061=ORIENTED_EDGE('',*,*,#21397,.T.);
#27062=ORIENTED_EDGE('',*,*,#21398,.F.);
#27063=ORIENTED_EDGE('',*,*,#20940,.T.);
#27064=ORIENTED_EDGE('',*,*,#21399,.T.);
#27065=ORIENTED_EDGE('',*,*,#21400,.T.);
#27066=ORIENTED_EDGE('',*,*,#21401,.F.);
#27067=ORIENTED_EDGE('',*,*,#20936,.T.);
#27068=ORIENTED_EDGE('',*,*,#21402,.T.);
#27069=ORIENTED_EDGE('',*,*,#21403,.T.);
#27070=ORIENTED_EDGE('',*,*,#21404,.F.);
#27071=ORIENTED_EDGE('',*,*,#20932,.T.);
#27072=ORIENTED_EDGE('',*,*,#21405,.T.);
#27073=ORIENTED_EDGE('',*,*,#21406,.T.);
#27074=ORIENTED_EDGE('',*,*,#21407,.F.);
#27075=ORIENTED_EDGE('',*,*,#20928,.T.);
#27076=ORIENTED_EDGE('',*,*,#21408,.T.);
#27077=ORIENTED_EDGE('',*,*,#21409,.T.);
#27078=ORIENTED_EDGE('',*,*,#21410,.F.);
#27079=ORIENTED_EDGE('',*,*,#20896,.T.);
#27080=ORIENTED_EDGE('',*,*,#21411,.T.);
#27081=ORIENTED_EDGE('',*,*,#21412,.T.);
#27082=ORIENTED_EDGE('',*,*,#21413,.F.);
#27083=ORIENTED_EDGE('',*,*,#20892,.T.);
#27084=ORIENTED_EDGE('',*,*,#21414,.T.);
#27085=ORIENTED_EDGE('',*,*,#21415,.T.);
#27086=ORIENTED_EDGE('',*,*,#21416,.F.);
#27087=ORIENTED_EDGE('',*,*,#20888,.T.);
#27088=ORIENTED_EDGE('',*,*,#21417,.T.);
#27089=ORIENTED_EDGE('',*,*,#21418,.T.);
#27090=ORIENTED_EDGE('',*,*,#21419,.F.);
#27091=ORIENTED_EDGE('',*,*,#20884,.T.);
#27092=ORIENTED_EDGE('',*,*,#21420,.T.);
#27093=ORIENTED_EDGE('',*,*,#21421,.T.);
#27094=ORIENTED_EDGE('',*,*,#21422,.F.);
#27095=ORIENTED_EDGE('',*,*,#20880,.T.);
#27096=ORIENTED_EDGE('',*,*,#21423,.T.);
#27097=ORIENTED_EDGE('',*,*,#21424,.T.);
#27098=ORIENTED_EDGE('',*,*,#21425,.F.);
#27099=ORIENTED_EDGE('',*,*,#20876,.F.);
#27100=ORIENTED_EDGE('',*,*,#21426,.F.);
#27101=ORIENTED_EDGE('',*,*,#21427,.F.);
#27102=ORIENTED_EDGE('',*,*,#21428,.T.);
#27103=ORIENTED_EDGE('',*,*,#20900,.F.);
#27104=ORIENTED_EDGE('',*,*,#21429,.F.);
#27105=ORIENTED_EDGE('',*,*,#21430,.F.);
#27106=ORIENTED_EDGE('',*,*,#21431,.T.);
#27107=ORIENTED_EDGE('',*,*,#20904,.F.);
#27108=ORIENTED_EDGE('',*,*,#21432,.F.);
#27109=ORIENTED_EDGE('',*,*,#21433,.F.);
#27110=ORIENTED_EDGE('',*,*,#21434,.T.);
#27111=ORIENTED_EDGE('',*,*,#20908,.F.);
#27112=ORIENTED_EDGE('',*,*,#21435,.F.);
#27113=ORIENTED_EDGE('',*,*,#21436,.F.);
#27114=ORIENTED_EDGE('',*,*,#21437,.T.);
#27115=ORIENTED_EDGE('',*,*,#20912,.F.);
#27116=ORIENTED_EDGE('',*,*,#21438,.F.);
#27117=ORIENTED_EDGE('',*,*,#21439,.F.);
#27118=ORIENTED_EDGE('',*,*,#21440,.T.);
#27119=ORIENTED_EDGE('',*,*,#20916,.F.);
#27120=ORIENTED_EDGE('',*,*,#21441,.F.);
#27121=ORIENTED_EDGE('',*,*,#21442,.F.);
#27122=ORIENTED_EDGE('',*,*,#21443,.T.);
#27123=ORIENTED_EDGE('',*,*,#20920,.F.);
#27124=ORIENTED_EDGE('',*,*,#21444,.F.);
#27125=ORIENTED_EDGE('',*,*,#21445,.F.);
#27126=ORIENTED_EDGE('',*,*,#21446,.T.);
#27127=ORIENTED_EDGE('',*,*,#20924,.F.);
#27128=ORIENTED_EDGE('',*,*,#21447,.F.);
#27129=ORIENTED_EDGE('',*,*,#21448,.F.);
#27130=ORIENTED_EDGE('',*,*,#21449,.T.);
#27131=ORIENTED_EDGE('',*,*,#20944,.F.);
#27132=ORIENTED_EDGE('',*,*,#21450,.F.);
#27133=ORIENTED_EDGE('',*,*,#21451,.F.);
#27134=ORIENTED_EDGE('',*,*,#21452,.T.);
#27135=ORIENTED_EDGE('',*,*,#20948,.F.);
#27136=ORIENTED_EDGE('',*,*,#21453,.F.);
#27137=ORIENTED_EDGE('',*,*,#21454,.F.);
#27138=ORIENTED_EDGE('',*,*,#21455,.T.);
#27139=ORIENTED_EDGE('',*,*,#20956,.F.);
#27140=ORIENTED_EDGE('',*,*,#21456,.F.);
#27141=ORIENTED_EDGE('',*,*,#21457,.F.);
#27142=ORIENTED_EDGE('',*,*,#21458,.T.);
#27143=ORIENTED_EDGE('',*,*,#20968,.F.);
#27144=ORIENTED_EDGE('',*,*,#21459,.F.);
#27145=ORIENTED_EDGE('',*,*,#21460,.F.);
#27146=ORIENTED_EDGE('',*,*,#21461,.T.);
#27147=ORIENTED_EDGE('',*,*,#21462,.F.);
#27148=ORIENTED_EDGE('',*,*,#20976,.F.);
#27149=ORIENTED_EDGE('',*,*,#21463,.T.);
#27150=ORIENTED_EDGE('',*,*,#21464,.F.);
#27151=ORIENTED_EDGE('',*,*,#21465,.F.);
#27152=ORIENTED_EDGE('',*,*,#20980,.F.);
#27153=ORIENTED_EDGE('',*,*,#21466,.T.);
#27154=ORIENTED_EDGE('',*,*,#21467,.F.);
#27155=ORIENTED_EDGE('',*,*,#21468,.F.);
#27156=ORIENTED_EDGE('',*,*,#20984,.F.);
#27157=ORIENTED_EDGE('',*,*,#21469,.T.);
#27158=ORIENTED_EDGE('',*,*,#21470,.F.);
#27159=ORIENTED_EDGE('',*,*,#21471,.F.);
#27160=ORIENTED_EDGE('',*,*,#20988,.F.);
#27161=ORIENTED_EDGE('',*,*,#21472,.T.);
#27162=ORIENTED_EDGE('',*,*,#21473,.F.);
#27163=ORIENTED_EDGE('',*,*,#21474,.F.);
#27164=ORIENTED_EDGE('',*,*,#20992,.F.);
#27165=ORIENTED_EDGE('',*,*,#21475,.T.);
#27166=ORIENTED_EDGE('',*,*,#21476,.F.);
#27167=ORIENTED_EDGE('',*,*,#21477,.F.);
#27168=ORIENTED_EDGE('',*,*,#21024,.F.);
#27169=ORIENTED_EDGE('',*,*,#21478,.T.);
#27170=ORIENTED_EDGE('',*,*,#21479,.F.);
#27171=ORIENTED_EDGE('',*,*,#21480,.F.);
#27172=ORIENTED_EDGE('',*,*,#21028,.F.);
#27173=ORIENTED_EDGE('',*,*,#21481,.T.);
#27174=ORIENTED_EDGE('',*,*,#21482,.F.);
#27175=ORIENTED_EDGE('',*,*,#21483,.F.);
#27176=ORIENTED_EDGE('',*,*,#21032,.F.);
#27177=ORIENTED_EDGE('',*,*,#21484,.T.);
#27178=ORIENTED_EDGE('',*,*,#21485,.F.);
#27179=ORIENTED_EDGE('',*,*,#21486,.F.);
#27180=ORIENTED_EDGE('',*,*,#21036,.F.);
#27181=ORIENTED_EDGE('',*,*,#21487,.T.);
#27182=ORIENTED_EDGE('',*,*,#21488,.F.);
#27183=ORIENTED_EDGE('',*,*,#21489,.F.);
#27184=ORIENTED_EDGE('',*,*,#21048,.F.);
#27185=ORIENTED_EDGE('',*,*,#21490,.T.);
#27186=ORIENTED_EDGE('',*,*,#21491,.F.);
#27187=ORIENTED_EDGE('',*,*,#21492,.F.);
#27188=ORIENTED_EDGE('',*,*,#21056,.F.);
#27189=ORIENTED_EDGE('',*,*,#21493,.T.);
#27190=ORIENTED_EDGE('',*,*,#21494,.F.);
#27191=ORIENTED_EDGE('',*,*,#21495,.F.);
#27192=ORIENTED_EDGE('',*,*,#21060,.F.);
#27193=ORIENTED_EDGE('',*,*,#21496,.T.);
#27194=ORIENTED_EDGE('',*,*,#21497,.F.);
#27195=ORIENTED_EDGE('',*,*,#21498,.T.);
#27196=ORIENTED_EDGE('',*,*,#21499,.T.);
#27197=ORIENTED_EDGE('',*,*,#21500,.T.);
#27198=ORIENTED_EDGE('',*,*,#21501,.F.);
#27199=ORIENTED_EDGE('',*,*,#21502,.T.);
#27200=ORIENTED_EDGE('',*,*,#21503,.F.);
#27201=ORIENTED_EDGE('',*,*,#21504,.F.);
#27202=ORIENTED_EDGE('',*,*,#21505,.F.);
#27203=ORIENTED_EDGE('',*,*,#21506,.F.);
#27204=ORIENTED_EDGE('',*,*,#21507,.T.);
#27205=ORIENTED_EDGE('',*,*,#21058,.T.);
#27206=ORIENTED_EDGE('',*,*,#21508,.T.);
#27207=ORIENTED_EDGE('',*,*,#21509,.T.);
#27208=ORIENTED_EDGE('',*,*,#21510,.F.);
#27209=ORIENTED_EDGE('',*,*,#21054,.T.);
#27210=ORIENTED_EDGE('',*,*,#21511,.T.);
#27211=ORIENTED_EDGE('',*,*,#21512,.T.);
#27212=ORIENTED_EDGE('',*,*,#21513,.F.);
#27213=ORIENTED_EDGE('',*,*,#21050,.F.);
#27214=ORIENTED_EDGE('',*,*,#21514,.F.);
#27215=ORIENTED_EDGE('',*,*,#21515,.F.);
#27216=ORIENTED_EDGE('',*,*,#21516,.T.);
#27217=ORIENTED_EDGE('',*,*,#21038,.F.);
#27218=ORIENTED_EDGE('',*,*,#21517,.F.);
#27219=ORIENTED_EDGE('',*,*,#21518,.F.);
#27220=ORIENTED_EDGE('',*,*,#21519,.T.);
#27221=ORIENTED_EDGE('',*,*,#21014,.F.);
#27222=ORIENTED_EDGE('',*,*,#21520,.F.);
#27223=ORIENTED_EDGE('',*,*,#21521,.F.);
#27224=ORIENTED_EDGE('',*,*,#21522,.T.);
#27225=ORIENTED_EDGE('',*,*,#21006,.F.);
#27226=ORIENTED_EDGE('',*,*,#21523,.F.);
#27227=ORIENTED_EDGE('',*,*,#21524,.F.);
#27228=ORIENTED_EDGE('',*,*,#21525,.T.);
#27229=ORIENTED_EDGE('',*,*,#20998,.F.);
#27230=ORIENTED_EDGE('',*,*,#21526,.F.);
#27231=ORIENTED_EDGE('',*,*,#21527,.F.);
#27232=ORIENTED_EDGE('',*,*,#21528,.T.);
#27233=ORIENTED_EDGE('',*,*,#20990,.T.);
#27234=ORIENTED_EDGE('',*,*,#21529,.T.);
#27235=ORIENTED_EDGE('',*,*,#21530,.T.);
#27236=ORIENTED_EDGE('',*,*,#21531,.F.);
#27237=ORIENTED_EDGE('',*,*,#20986,.T.);
#27238=ORIENTED_EDGE('',*,*,#21532,.T.);
#27239=ORIENTED_EDGE('',*,*,#21533,.T.);
#27240=ORIENTED_EDGE('',*,*,#21534,.F.);
#27241=ORIENTED_EDGE('',*,*,#20982,.T.);
#27242=ORIENTED_EDGE('',*,*,#21535,.T.);
#27243=ORIENTED_EDGE('',*,*,#21536,.T.);
#27244=ORIENTED_EDGE('',*,*,#21537,.F.);
#27245=ORIENTED_EDGE('',*,*,#20978,.T.);
#27246=ORIENTED_EDGE('',*,*,#21538,.T.);
#27247=ORIENTED_EDGE('',*,*,#21539,.T.);
#27248=ORIENTED_EDGE('',*,*,#21540,.F.);
#27249=ORIENTED_EDGE('',*,*,#20974,.T.);
#27250=ORIENTED_EDGE('',*,*,#21541,.T.);
#27251=ORIENTED_EDGE('',*,*,#21542,.T.);
#27252=ORIENTED_EDGE('',*,*,#21543,.F.);
#27253=ORIENTED_EDGE('',*,*,#20970,.F.);
#27254=ORIENTED_EDGE('',*,*,#21544,.F.);
#27255=ORIENTED_EDGE('',*,*,#21545,.F.);
#27256=ORIENTED_EDGE('',*,*,#21546,.T.);
#27257=ORIENTED_EDGE('',*,*,#21547,.F.);
#27258=ORIENTED_EDGE('',*,*,#20958,.F.);
#27259=ORIENTED_EDGE('',*,*,#21548,.T.);
#27260=ORIENTED_EDGE('',*,*,#21549,.F.);
#27261=ORIENTED_EDGE('',*,*,#21550,.T.);
#27262=ORIENTED_EDGE('',*,*,#20946,.T.);
#27263=ORIENTED_EDGE('',*,*,#21551,.F.);
#27264=ORIENTED_EDGE('',*,*,#21552,.T.);
#27265=ORIENTED_EDGE('',*,*,#21553,.T.);
#27266=ORIENTED_EDGE('',*,*,#20942,.T.);
#27267=ORIENTED_EDGE('',*,*,#21554,.F.);
#27268=ORIENTED_EDGE('',*,*,#21555,.T.);
#27269=ORIENTED_EDGE('',*,*,#21556,.F.);
#27270=ORIENTED_EDGE('',*,*,#20938,.F.);
#27271=ORIENTED_EDGE('',*,*,#21557,.T.);
#27272=ORIENTED_EDGE('',*,*,#21558,.F.);
#27273=ORIENTED_EDGE('',*,*,#21559,.F.);
#27274=ORIENTED_EDGE('',*,*,#20930,.F.);
#27275=ORIENTED_EDGE('',*,*,#21560,.T.);
#27276=ORIENTED_EDGE('',*,*,#21561,.F.);
#27277=ORIENTED_EDGE('',*,*,#21562,.T.);
#27278=ORIENTED_EDGE('',*,*,#20922,.T.);
#27279=ORIENTED_EDGE('',*,*,#21563,.F.);
#27280=ORIENTED_EDGE('',*,*,#21564,.T.);
#27281=ORIENTED_EDGE('',*,*,#21565,.T.);
#27282=ORIENTED_EDGE('',*,*,#20918,.T.);
#27283=ORIENTED_EDGE('',*,*,#21566,.F.);
#27284=ORIENTED_EDGE('',*,*,#21567,.T.);
#27285=ORIENTED_EDGE('',*,*,#21568,.T.);
#27286=ORIENTED_EDGE('',*,*,#20914,.T.);
#27287=ORIENTED_EDGE('',*,*,#21569,.F.);
#27288=ORIENTED_EDGE('',*,*,#21570,.T.);
#27289=ORIENTED_EDGE('',*,*,#21571,.T.);
#27290=ORIENTED_EDGE('',*,*,#20910,.T.);
#27291=ORIENTED_EDGE('',*,*,#21572,.F.);
#27292=ORIENTED_EDGE('',*,*,#21573,.T.);
#27293=ORIENTED_EDGE('',*,*,#21574,.T.);
#27294=ORIENTED_EDGE('',*,*,#20906,.T.);
#27295=ORIENTED_EDGE('',*,*,#21575,.F.);
#27296=ORIENTED_EDGE('',*,*,#21576,.T.);
#27297=ORIENTED_EDGE('',*,*,#21577,.T.);
#27298=ORIENTED_EDGE('',*,*,#20902,.T.);
#27299=ORIENTED_EDGE('',*,*,#21578,.F.);
#27300=ORIENTED_EDGE('',*,*,#21579,.T.);
#27301=ORIENTED_EDGE('',*,*,#21580,.T.);
#27302=ORIENTED_EDGE('',*,*,#20898,.T.);
#27303=ORIENTED_EDGE('',*,*,#21581,.F.);
#27304=ORIENTED_EDGE('',*,*,#21582,.T.);
#27305=ORIENTED_EDGE('',*,*,#21583,.F.);
#27306=ORIENTED_EDGE('',*,*,#20894,.F.);
#27307=ORIENTED_EDGE('',*,*,#21584,.T.);
#27308=ORIENTED_EDGE('',*,*,#21585,.F.);
#27309=ORIENTED_EDGE('',*,*,#21586,.F.);
#27310=ORIENTED_EDGE('',*,*,#20886,.F.);
#27311=ORIENTED_EDGE('',*,*,#21587,.T.);
#27312=ORIENTED_EDGE('',*,*,#21588,.F.);
#27313=ORIENTED_EDGE('',*,*,#21589,.F.);
#27314=ORIENTED_EDGE('',*,*,#20878,.F.);
#27315=ORIENTED_EDGE('',*,*,#21590,.T.);
#27316=ORIENTED_EDGE('',*,*,#21591,.F.);
#27317=ORIENTED_EDGE('',*,*,#21592,.T.);
#27318=ORIENTED_EDGE('',*,*,#20874,.T.);
#27319=ORIENTED_EDGE('',*,*,#21593,.F.);
#27320=ORIENTED_EDGE('',*,*,#21594,.T.);
#27321=ORIENTED_EDGE('',*,*,#21595,.F.);
#27322=ORIENTED_EDGE('',*,*,#20882,.F.);
#27323=ORIENTED_EDGE('',*,*,#21596,.T.);
#27324=ORIENTED_EDGE('',*,*,#21597,.F.);
#27325=ORIENTED_EDGE('',*,*,#21598,.F.);
#27326=ORIENTED_EDGE('',*,*,#20890,.F.);
#27327=ORIENTED_EDGE('',*,*,#21599,.T.);
#27328=ORIENTED_EDGE('',*,*,#21600,.F.);
#27329=ORIENTED_EDGE('',*,*,#21601,.F.);
#27330=ORIENTED_EDGE('',*,*,#20926,.F.);
#27331=ORIENTED_EDGE('',*,*,#21602,.T.);
#27332=ORIENTED_EDGE('',*,*,#21603,.F.);
#27333=ORIENTED_EDGE('',*,*,#21604,.F.);
#27334=ORIENTED_EDGE('',*,*,#20934,.F.);
#27335=ORIENTED_EDGE('',*,*,#21605,.T.);
#27336=ORIENTED_EDGE('',*,*,#21606,.F.);
#27337=ORIENTED_EDGE('',*,*,#21607,.F.);
#27338=ORIENTED_EDGE('',*,*,#20950,.F.);
#27339=ORIENTED_EDGE('',*,*,#21608,.T.);
#27340=ORIENTED_EDGE('',*,*,#21609,.F.);
#27341=ORIENTED_EDGE('',*,*,#21610,.T.);
#27342=ORIENTED_EDGE('',*,*,#20954,.T.);
#27343=ORIENTED_EDGE('',*,*,#21611,.F.);
#27344=ORIENTED_EDGE('',*,*,#21612,.T.);
#27345=ORIENTED_EDGE('',*,*,#21613,.F.);
#27346=ORIENTED_EDGE('',*,*,#20962,.F.);
#27347=ORIENTED_EDGE('',*,*,#21614,.T.);
#27348=ORIENTED_EDGE('',*,*,#21615,.F.);
#27349=ORIENTED_EDGE('',*,*,#21616,.T.);
#27350=ORIENTED_EDGE('',*,*,#20966,.T.);
#27351=ORIENTED_EDGE('',*,*,#21617,.F.);
#27352=ORIENTED_EDGE('',*,*,#21618,.T.);
#27353=ORIENTED_EDGE('',*,*,#20994,.F.);
#27354=ORIENTED_EDGE('',*,*,#21619,.F.);
#27355=ORIENTED_EDGE('',*,*,#21620,.F.);
#27356=ORIENTED_EDGE('',*,*,#21621,.T.);
#27357=ORIENTED_EDGE('',*,*,#21002,.F.);
#27358=ORIENTED_EDGE('',*,*,#21622,.F.);
#27359=ORIENTED_EDGE('',*,*,#21623,.F.);
#27360=ORIENTED_EDGE('',*,*,#21624,.T.);
#27361=ORIENTED_EDGE('',*,*,#21010,.F.);
#27362=ORIENTED_EDGE('',*,*,#21625,.F.);
#27363=ORIENTED_EDGE('',*,*,#21626,.F.);
#27364=ORIENTED_EDGE('',*,*,#21627,.T.);
#27365=ORIENTED_EDGE('',*,*,#21018,.F.);
#27366=ORIENTED_EDGE('',*,*,#21628,.F.);
#27367=ORIENTED_EDGE('',*,*,#21629,.F.);
#27368=ORIENTED_EDGE('',*,*,#21630,.T.);
#27369=ORIENTED_EDGE('',*,*,#21022,.T.);
#27370=ORIENTED_EDGE('',*,*,#21631,.T.);
#27371=ORIENTED_EDGE('',*,*,#21632,.T.);
#27372=ORIENTED_EDGE('',*,*,#21633,.F.);
#27373=ORIENTED_EDGE('',*,*,#21026,.T.);
#27374=ORIENTED_EDGE('',*,*,#21634,.T.);
#27375=ORIENTED_EDGE('',*,*,#21635,.T.);
#27376=ORIENTED_EDGE('',*,*,#21636,.F.);
#27377=ORIENTED_EDGE('',*,*,#21030,.T.);
#27378=ORIENTED_EDGE('',*,*,#21637,.T.);
#27379=ORIENTED_EDGE('',*,*,#21638,.T.);
#27380=ORIENTED_EDGE('',*,*,#21639,.F.);
#27381=ORIENTED_EDGE('',*,*,#21034,.T.);
#27382=ORIENTED_EDGE('',*,*,#21640,.T.);
#27383=ORIENTED_EDGE('',*,*,#21641,.T.);
#27384=ORIENTED_EDGE('',*,*,#21642,.F.);
#27385=ORIENTED_EDGE('',*,*,#21042,.F.);
#27386=ORIENTED_EDGE('',*,*,#21643,.F.);
#27387=ORIENTED_EDGE('',*,*,#21644,.F.);
#27388=ORIENTED_EDGE('',*,*,#21645,.T.);
#27389=ORIENTED_EDGE('',*,*,#21046,.T.);
#27390=ORIENTED_EDGE('',*,*,#21646,.T.);
#27391=ORIENTED_EDGE('',*,*,#21647,.T.);
#27392=ORIENTED_EDGE('',*,*,#21648,.F.);
#27393=ORIENTED_EDGE('',*,*,#21062,.F.);
#27394=ORIENTED_EDGE('',*,*,#21649,.F.);
#27395=ORIENTED_EDGE('',*,*,#21650,.F.);
#27396=ORIENTED_EDGE('',*,*,#21651,.T.);
#27397=ORIENTED_EDGE('',*,*,#21652,.F.);
#27398=ORIENTED_EDGE('',*,*,#21111,.T.);
#27399=ORIENTED_EDGE('',*,*,#21653,.F.);
#27400=ORIENTED_EDGE('',*,*,#21654,.T.);
#27401=ORIENTED_EDGE('',*,*,#21655,.F.);
#27402=ORIENTED_EDGE('',*,*,#21656,.T.);
#27403=ORIENTED_EDGE('',*,*,#21657,.F.);
#27404=ORIENTED_EDGE('',*,*,#21095,.T.);
#27405=ORIENTED_EDGE('',*,*,#21658,.F.);
#27406=ORIENTED_EDGE('',*,*,#21659,.T.);
#27407=ORIENTED_EDGE('',*,*,#21660,.F.);
#27408=ORIENTED_EDGE('',*,*,#21661,.T.);
#27409=ORIENTED_EDGE('',*,*,#21662,.F.);
#27410=ORIENTED_EDGE('',*,*,#21109,.T.);
#27411=ORIENTED_EDGE('',*,*,#21663,.F.);
#27412=ORIENTED_EDGE('',*,*,#21664,.T.);
#27413=ORIENTED_EDGE('',*,*,#21665,.F.);
#27414=ORIENTED_EDGE('',*,*,#21666,.T.);
#27415=ORIENTED_EDGE('',*,*,#21667,.F.);
#27416=ORIENTED_EDGE('',*,*,#21668,.T.);
#27417=ORIENTED_EDGE('',*,*,#21669,.F.);
#27418=ORIENTED_EDGE('',*,*,#21105,.T.);
#27419=ORIENTED_EDGE('',*,*,#21670,.F.);
#27420=ORIENTED_EDGE('',*,*,#21671,.T.);
#27421=ORIENTED_EDGE('',*,*,#21672,.F.);
#27422=ORIENTED_EDGE('',*,*,#21099,.T.);
#27423=ORIENTED_EDGE('',*,*,#21673,.F.);
#27424=ORIENTED_EDGE('',*,*,#21674,.T.);
#27425=ORIENTED_EDGE('',*,*,#21675,.F.);
#27426=ORIENTED_EDGE('',*,*,#21676,.T.);
#27427=ORIENTED_EDGE('',*,*,#21677,.F.);
#27428=ORIENTED_EDGE('',*,*,#21678,.T.);
#27429=ORIENTED_EDGE('',*,*,#21679,.F.);
#27430=ORIENTED_EDGE('',*,*,#21680,.T.);
#27431=ORIENTED_EDGE('',*,*,#21681,.F.);
#27432=ORIENTED_EDGE('',*,*,#21682,.T.);
#27433=ORIENTED_EDGE('',*,*,#21683,.F.);
#27434=ORIENTED_EDGE('',*,*,#21684,.T.);
#27435=ORIENTED_EDGE('',*,*,#21685,.F.);
#27436=ORIENTED_EDGE('',*,*,#21093,.T.);
#27437=ORIENTED_EDGE('',*,*,#21686,.F.);
#27438=ORIENTED_EDGE('',*,*,#21687,.T.);
#27439=ORIENTED_EDGE('',*,*,#21688,.F.);
#27440=ORIENTED_EDGE('',*,*,#21689,.T.);
#27441=ORIENTED_EDGE('',*,*,#21690,.F.);
#27442=ORIENTED_EDGE('',*,*,#21691,.T.);
#27443=ORIENTED_EDGE('',*,*,#21692,.F.);
#27444=ORIENTED_EDGE('',*,*,#21693,.T.);
#27445=ORIENTED_EDGE('',*,*,#21694,.F.);
#27446=ORIENTED_EDGE('',*,*,#21123,.T.);
#27447=ORIENTED_EDGE('',*,*,#21695,.F.);
#27448=ORIENTED_EDGE('',*,*,#21696,.T.);
#27449=ORIENTED_EDGE('',*,*,#21697,.F.);
#27450=ORIENTED_EDGE('',*,*,#21698,.T.);
#27451=ORIENTED_EDGE('',*,*,#21699,.F.);
#27452=ORIENTED_EDGE('',*,*,#21119,.T.);
#27453=ORIENTED_EDGE('',*,*,#21700,.F.);
#27454=ORIENTED_EDGE('',*,*,#21701,.T.);
#27455=ORIENTED_EDGE('',*,*,#21702,.F.);
#27456=ORIENTED_EDGE('',*,*,#21703,.T.);
#27457=ORIENTED_EDGE('',*,*,#21704,.F.);
#27458=ORIENTED_EDGE('',*,*,#21137,.T.);
#27459=ORIENTED_EDGE('',*,*,#21705,.F.);
#27460=ORIENTED_EDGE('',*,*,#21706,.T.);
#27461=ORIENTED_EDGE('',*,*,#21707,.F.);
#27462=ORIENTED_EDGE('',*,*,#21708,.T.);
#27463=ORIENTED_EDGE('',*,*,#21709,.F.);
#27464=ORIENTED_EDGE('',*,*,#21710,.T.);
#27465=ORIENTED_EDGE('',*,*,#21711,.F.);
#27466=ORIENTED_EDGE('',*,*,#21133,.T.);
#27467=ORIENTED_EDGE('',*,*,#21712,.F.);
#27468=ORIENTED_EDGE('',*,*,#21713,.T.);
#27469=ORIENTED_EDGE('',*,*,#21714,.F.);
#27470=ORIENTED_EDGE('',*,*,#21127,.T.);
#27471=ORIENTED_EDGE('',*,*,#21715,.F.);
#27472=ORIENTED_EDGE('',*,*,#21716,.T.);
#27473=ORIENTED_EDGE('',*,*,#21717,.F.);
#27474=ORIENTED_EDGE('',*,*,#21718,.T.);
#27475=ORIENTED_EDGE('',*,*,#21719,.F.);
#27476=ORIENTED_EDGE('',*,*,#21720,.T.);
#27477=ORIENTED_EDGE('',*,*,#21721,.F.);
#27478=ORIENTED_EDGE('',*,*,#21722,.T.);
#27479=ORIENTED_EDGE('',*,*,#21723,.F.);
#27480=ORIENTED_EDGE('',*,*,#21724,.T.);
#27481=ORIENTED_EDGE('',*,*,#21725,.F.);
#27482=ORIENTED_EDGE('',*,*,#21726,.T.);
#27483=ORIENTED_EDGE('',*,*,#21727,.F.);
#27484=ORIENTED_EDGE('',*,*,#21117,.T.);
#27485=ORIENTED_EDGE('',*,*,#21728,.F.);
#27486=ORIENTED_EDGE('',*,*,#21729,.T.);
#27487=ORIENTED_EDGE('',*,*,#21730,.F.);
#27488=ORIENTED_EDGE('',*,*,#21731,.T.);
#27489=ORIENTED_EDGE('',*,*,#21732,.F.);
#27490=ORIENTED_EDGE('',*,*,#21733,.T.);
#27491=ORIENTED_EDGE('',*,*,#21734,.F.);
#27492=ORIENTED_EDGE('',*,*,#21735,.T.);
#27493=ORIENTED_EDGE('',*,*,#21736,.T.);
#27494=ORIENTED_EDGE('',*,*,#21737,.T.);
#27495=ORIENTED_EDGE('',*,*,#21738,.F.);
#27496=ORIENTED_EDGE('',*,*,#21739,.T.);
#27497=ORIENTED_EDGE('',*,*,#21172,.F.);
#27498=ORIENTED_EDGE('',*,*,#21154,.F.);
#27499=ORIENTED_EDGE('',*,*,#21740,.T.);
#27500=ORIENTED_EDGE('',*,*,#21679,.T.);
#27501=ORIENTED_EDGE('',*,*,#21741,.T.);
#27502=ORIENTED_EDGE('',*,*,#21742,.T.);
#27503=ORIENTED_EDGE('',*,*,#21142,.T.);
#27504=ORIENTED_EDGE('',*,*,#21743,.T.);
#27505=ORIENTED_EDGE('',*,*,#21653,.T.);
#27506=ORIENTED_EDGE('',*,*,#21110,.T.);
#27507=ORIENTED_EDGE('',*,*,#21744,.F.);
#27508=ORIENTED_EDGE('',*,*,#21146,.F.);
#27509=ORIENTED_EDGE('',*,*,#21745,.T.);
#27510=ORIENTED_EDGE('',*,*,#21746,.T.);
#27511=ORIENTED_EDGE('',*,*,#21747,.T.);
#27512=ORIENTED_EDGE('',*,*,#21748,.T.);
#27513=ORIENTED_EDGE('',*,*,#21138,.T.);
#27514=ORIENTED_EDGE('',*,*,#21749,.T.);
#27515=ORIENTED_EDGE('',*,*,#21750,.T.);
#27516=ORIENTED_EDGE('',*,*,#21086,.T.);
#27517=ORIENTED_EDGE('',*,*,#21751,.F.);
#27518=ORIENTED_EDGE('',*,*,#21752,.T.);
#27519=ORIENTED_EDGE('',*,*,#21753,.T.);
#27520=ORIENTED_EDGE('',*,*,#21754,.T.);
#27521=ORIENTED_EDGE('',*,*,#21066,.T.);
#27522=ORIENTED_EDGE('',*,*,#21755,.T.);
#27523=ORIENTED_EDGE('',*,*,#21756,.T.);
#27524=ORIENTED_EDGE('',*,*,#21757,.F.);
#27525=ORIENTED_EDGE('',*,*,#21758,.T.);
#27526=ORIENTED_EDGE('',*,*,#21759,.T.);
#27527=ORIENTED_EDGE('',*,*,#21070,.T.);
#27528=ORIENTED_EDGE('',*,*,#21760,.T.);
#27529=ORIENTED_EDGE('',*,*,#21761,.T.);
#27530=ORIENTED_EDGE('',*,*,#21762,.T.);
#27531=ORIENTED_EDGE('',*,*,#21763,.T.);
#27532=ORIENTED_EDGE('',*,*,#21764,.F.);
#27533=ORIENTED_EDGE('',*,*,#21765,.T.);
#27534=ORIENTED_EDGE('',*,*,#21766,.T.);
#27535=ORIENTED_EDGE('',*,*,#21767,.T.);
#27536=ORIENTED_EDGE('',*,*,#21768,.T.);
#27537=ORIENTED_EDGE('',*,*,#21769,.T.);
#27538=ORIENTED_EDGE('',*,*,#21770,.T.);
#27539=ORIENTED_EDGE('',*,*,#21771,.T.);
#27540=ORIENTED_EDGE('',*,*,#21772,.F.);
#27541=ORIENTED_EDGE('',*,*,#21082,.T.);
#27542=ORIENTED_EDGE('',*,*,#21773,.T.);
#27543=ORIENTED_EDGE('',*,*,#21774,.T.);
#27544=ORIENTED_EDGE('',*,*,#21775,.T.);
#27545=ORIENTED_EDGE('',*,*,#21776,.T.);
#27546=ORIENTED_EDGE('',*,*,#21777,.T.);
#27547=ORIENTED_EDGE('',*,*,#21778,.T.);
#27548=ORIENTED_EDGE('',*,*,#21779,.F.);
#27549=ORIENTED_EDGE('',*,*,#21078,.T.);
#27550=ORIENTED_EDGE('',*,*,#21780,.T.);
#27551=ORIENTED_EDGE('',*,*,#21781,.T.);
#27552=ORIENTED_EDGE('',*,*,#21782,.T.);
#27553=ORIENTED_EDGE('',*,*,#21783,.T.);
#27554=ORIENTED_EDGE('',*,*,#21784,.T.);
#27555=ORIENTED_EDGE('',*,*,#21074,.T.);
#27556=ORIENTED_EDGE('',*,*,#21785,.F.);
#27557=ORIENTED_EDGE('',*,*,#21786,.T.);
#27558=ORIENTED_EDGE('',*,*,#21686,.T.);
#27559=ORIENTED_EDGE('',*,*,#21787,.T.);
#27560=ORIENTED_EDGE('',*,*,#21788,.T.);
#27561=ORIENTED_EDGE('',*,*,#21090,.T.);
#27562=ORIENTED_EDGE('',*,*,#21685,.T.);
#27563=ORIENTED_EDGE('',*,*,#21789,.T.);
#27564=ORIENTED_EDGE('',*,*,#21790,.F.);
#27565=ORIENTED_EDGE('',*,*,#21791,.T.);
#27566=ORIENTED_EDGE('',*,*,#21655,.T.);
#27567=ORIENTED_EDGE('',*,*,#21094,.T.);
#27568=ORIENTED_EDGE('',*,*,#21792,.T.);
#27569=ORIENTED_EDGE('',*,*,#21793,.T.);
#27570=ORIENTED_EDGE('',*,*,#21690,.T.);
#27571=ORIENTED_EDGE('',*,*,#21794,.T.);
#27572=ORIENTED_EDGE('',*,*,#21795,.F.);
#27573=ORIENTED_EDGE('',*,*,#21796,.T.);
#27574=ORIENTED_EDGE('',*,*,#21662,.T.);
#27575=ORIENTED_EDGE('',*,*,#21797,.T.);
#27576=ORIENTED_EDGE('',*,*,#21798,.T.);
#27577=ORIENTED_EDGE('',*,*,#21799,.T.);
#27578=ORIENTED_EDGE('',*,*,#21660,.T.);
#27579=ORIENTED_EDGE('',*,*,#21800,.T.);
#27580=ORIENTED_EDGE('',*,*,#21801,.F.);
#27581=ORIENTED_EDGE('',*,*,#21106,.T.);
#27582=ORIENTED_EDGE('',*,*,#21669,.T.);
#27583=ORIENTED_EDGE('',*,*,#21802,.T.);
#27584=ORIENTED_EDGE('',*,*,#21803,.T.);
#27585=ORIENTED_EDGE('',*,*,#21804,.T.);
#27586=ORIENTED_EDGE('',*,*,#21667,.T.);
#27587=ORIENTED_EDGE('',*,*,#21805,.T.);
#27588=ORIENTED_EDGE('',*,*,#21806,.F.);
#27589=ORIENTED_EDGE('',*,*,#21102,.T.);
#27590=ORIENTED_EDGE('',*,*,#21675,.T.);
#27591=ORIENTED_EDGE('',*,*,#21807,.T.);
#27592=ORIENTED_EDGE('',*,*,#21808,.T.);
#27593=ORIENTED_EDGE('',*,*,#21809,.T.);
#27594=ORIENTED_EDGE('',*,*,#21673,.T.);
#27595=ORIENTED_EDGE('',*,*,#21098,.T.);
#27596=ORIENTED_EDGE('',*,*,#21810,.F.);
#27597=ORIENTED_EDGE('',*,*,#21811,.T.);
#27598=ORIENTED_EDGE('',*,*,#21728,.T.);
#27599=ORIENTED_EDGE('',*,*,#21812,.T.);
#27600=ORIENTED_EDGE('',*,*,#21813,.T.);
#27601=ORIENTED_EDGE('',*,*,#21114,.T.);
#27602=ORIENTED_EDGE('',*,*,#21727,.T.);
#27603=ORIENTED_EDGE('',*,*,#21814,.T.);
#27604=ORIENTED_EDGE('',*,*,#21736,.F.);
#27605=ORIENTED_EDGE('',*,*,#21815,.T.);
#27606=ORIENTED_EDGE('',*,*,#21697,.T.);
#27607=ORIENTED_EDGE('',*,*,#21118,.T.);
#27608=ORIENTED_EDGE('',*,*,#21816,.T.);
#27609=ORIENTED_EDGE('',*,*,#21817,.T.);
#27610=ORIENTED_EDGE('',*,*,#21732,.T.);
#27611=ORIENTED_EDGE('',*,*,#21818,.T.);
#27612=ORIENTED_EDGE('',*,*,#21819,.F.);
#27613=ORIENTED_EDGE('',*,*,#21820,.T.);
#27614=ORIENTED_EDGE('',*,*,#21704,.T.);
#27615=ORIENTED_EDGE('',*,*,#21821,.T.);
#27616=ORIENTED_EDGE('',*,*,#21822,.T.);
#27617=ORIENTED_EDGE('',*,*,#21823,.T.);
#27618=ORIENTED_EDGE('',*,*,#21702,.T.);
#27619=ORIENTED_EDGE('',*,*,#21824,.T.);
#27620=ORIENTED_EDGE('',*,*,#21825,.F.);
#27621=ORIENTED_EDGE('',*,*,#21134,.T.);
#27622=ORIENTED_EDGE('',*,*,#21711,.T.);
#27623=ORIENTED_EDGE('',*,*,#21826,.T.);
#27624=ORIENTED_EDGE('',*,*,#21827,.T.);
#27625=ORIENTED_EDGE('',*,*,#21828,.T.);
#27626=ORIENTED_EDGE('',*,*,#21709,.T.);
#27627=ORIENTED_EDGE('',*,*,#21829,.T.);
#27628=ORIENTED_EDGE('',*,*,#21830,.F.);
#27629=ORIENTED_EDGE('',*,*,#21130,.T.);
#27630=ORIENTED_EDGE('',*,*,#21717,.T.);
#27631=ORIENTED_EDGE('',*,*,#21831,.T.);
#27632=ORIENTED_EDGE('',*,*,#21832,.T.);
#27633=ORIENTED_EDGE('',*,*,#21833,.T.);
#27634=ORIENTED_EDGE('',*,*,#21715,.T.);
#27635=ORIENTED_EDGE('',*,*,#21126,.T.);
#27636=ORIENTED_EDGE('',*,*,#21834,.F.);
#27637=ORIENTED_EDGE('',*,*,#21835,.T.);
#27638=ORIENTED_EDGE('',*,*,#21192,.F.);
#27639=ORIENTED_EDGE('',*,*,#21836,.T.);
#27640=ORIENTED_EDGE('',*,*,#21721,.T.);
#27641=ORIENTED_EDGE('',*,*,#21837,.T.);
#27642=ORIENTED_EDGE('',*,*,#21838,.T.);
#27643=ORIENTED_EDGE('',*,*,#21150,.T.);
#27644=ORIENTED_EDGE('',*,*,#21839,.T.);
#27645=ORIENTED_EDGE('',*,*,#21695,.T.);
#27646=ORIENTED_EDGE('',*,*,#21122,.T.);
#27647=ORIENTED_EDGE('',*,*,#21840,.F.);
#27648=ORIENTED_EDGE('',*,*,#21193,.F.);
#27649=ORIENTED_EDGE('',*,*,#21840,.T.);
#27650=ORIENTED_EDGE('',*,*,#21125,.T.);
#27651=ORIENTED_EDGE('',*,*,#21841,.F.);
#27652=ORIENTED_EDGE('',*,*,#21842,.F.);
#27653=ORIENTED_EDGE('',*,*,#21087,.T.);
#27654=ORIENTED_EDGE('',*,*,#21750,.F.);
#27655=ORIENTED_EDGE('',*,*,#21843,.T.);
#27656=ORIENTED_EDGE('',*,*,#21834,.T.);
#27657=ORIENTED_EDGE('',*,*,#21129,.T.);
#27658=ORIENTED_EDGE('',*,*,#21844,.F.);
#27659=ORIENTED_EDGE('',*,*,#21845,.T.);
#27660=ORIENTED_EDGE('',*,*,#21830,.T.);
#27661=ORIENTED_EDGE('',*,*,#21846,.T.);
#27662=ORIENTED_EDGE('',*,*,#21847,.F.);
#27663=ORIENTED_EDGE('',*,*,#21131,.T.);
#27664=ORIENTED_EDGE('',*,*,#21825,.T.);
#27665=ORIENTED_EDGE('',*,*,#21848,.T.);
#27666=ORIENTED_EDGE('',*,*,#21849,.F.);
#27667=ORIENTED_EDGE('',*,*,#21135,.T.);
#27668=ORIENTED_EDGE('',*,*,#21850,.T.);
#27669=ORIENTED_EDGE('',*,*,#21851,.T.);
#27670=ORIENTED_EDGE('',*,*,#21852,.F.);
#27671=ORIENTED_EDGE('',*,*,#21853,.F.);
#27672=ORIENTED_EDGE('',*,*,#21854,.F.);
#27673=ORIENTED_EDGE('',*,*,#21855,.F.);
#27674=ORIENTED_EDGE('',*,*,#21856,.F.);
#27675=ORIENTED_EDGE('',*,*,#21857,.F.);
#27676=ORIENTED_EDGE('',*,*,#21858,.T.);
#27677=ORIENTED_EDGE('',*,*,#21859,.T.);
#27678=ORIENTED_EDGE('',*,*,#21163,.F.);
#27679=ORIENTED_EDGE('',*,*,#21160,.T.);
#27680=ORIENTED_EDGE('',*,*,#20858,.F.);
#27681=ORIENTED_EDGE('',*,*,#20861,.F.);
#27682=ORIENTED_EDGE('',*,*,#20864,.F.);
#27683=ORIENTED_EDGE('',*,*,#20867,.F.);
#27684=ORIENTED_EDGE('',*,*,#21860,.F.);
#27685=ORIENTED_EDGE('',*,*,#21861,.F.);
#27686=ORIENTED_EDGE('',*,*,#21862,.F.);
#27687=ORIENTED_EDGE('',*,*,#21863,.F.);
#27688=ORIENTED_EDGE('',*,*,#21864,.F.);
#27689=ORIENTED_EDGE('',*,*,#21865,.F.);
#27690=ORIENTED_EDGE('',*,*,#21866,.F.);
#27691=ORIENTED_EDGE('',*,*,#21867,.F.);
#27692=ORIENTED_EDGE('',*,*,#21868,.F.);
#27693=ORIENTED_EDGE('',*,*,#21869,.F.);
#27694=ORIENTED_EDGE('',*,*,#21870,.F.);
#27695=ORIENTED_EDGE('',*,*,#21871,.F.);
#27696=ORIENTED_EDGE('',*,*,#21872,.F.);
#27697=ORIENTED_EDGE('',*,*,#21873,.F.);
#27698=ORIENTED_EDGE('',*,*,#21874,.F.);
#27699=ORIENTED_EDGE('',*,*,#21875,.F.);
#27700=ORIENTED_EDGE('',*,*,#21166,.T.);
#27701=ORIENTED_EDGE('',*,*,#21169,.F.);
#27702=ORIENTED_EDGE('',*,*,#21175,.F.);
#27703=ORIENTED_EDGE('',*,*,#21876,.T.);
#27704=ORIENTED_EDGE('',*,*,#21877,.T.);
#27705=ORIENTED_EDGE('',*,*,#21878,.F.);
#27706=ORIENTED_EDGE('',*,*,#21879,.T.);
#27707=ORIENTED_EDGE('',*,*,#21880,.F.);
#27708=ORIENTED_EDGE('',*,*,#21881,.F.);
#27709=ORIENTED_EDGE('',*,*,#21882,.T.);
#27710=ORIENTED_EDGE('',*,*,#21883,.T.);
#27711=ORIENTED_EDGE('',*,*,#21884,.F.);
#27712=ORIENTED_EDGE('',*,*,#21885,.F.);
#27713=ORIENTED_EDGE('',*,*,#21164,.F.);
#27714=ORIENTED_EDGE('',*,*,#21158,.F.);
#27715=ORIENTED_EDGE('',*,*,#20856,.T.);
#27716=ORIENTED_EDGE('',*,*,#20859,.T.);
#27717=ORIENTED_EDGE('',*,*,#20862,.T.);
#27718=ORIENTED_EDGE('',*,*,#20865,.T.);
#27719=ORIENTED_EDGE('',*,*,#21886,.T.);
#27720=ORIENTED_EDGE('',*,*,#21887,.T.);
#27721=ORIENTED_EDGE('',*,*,#21888,.T.);
#27722=ORIENTED_EDGE('',*,*,#21889,.T.);
#27723=ORIENTED_EDGE('',*,*,#21890,.T.);
#27724=ORIENTED_EDGE('',*,*,#21891,.T.);
#27725=ORIENTED_EDGE('',*,*,#21892,.T.);
#27726=ORIENTED_EDGE('',*,*,#21893,.T.);
#27727=ORIENTED_EDGE('',*,*,#21894,.T.);
#27728=ORIENTED_EDGE('',*,*,#21895,.T.);
#27729=ORIENTED_EDGE('',*,*,#21896,.T.);
#27730=ORIENTED_EDGE('',*,*,#21897,.T.);
#27731=ORIENTED_EDGE('',*,*,#21898,.T.);
#27732=ORIENTED_EDGE('',*,*,#21899,.T.);
#27733=ORIENTED_EDGE('',*,*,#21900,.T.);
#27734=ORIENTED_EDGE('',*,*,#21901,.T.);
#27735=ORIENTED_EDGE('',*,*,#21161,.T.);
#27736=ORIENTED_EDGE('',*,*,#21167,.T.);
#27737=ORIENTED_EDGE('',*,*,#21178,.F.);
#27738=ORIENTED_EDGE('',*,*,#21902,.F.);
#27739=ORIENTED_EDGE('',*,*,#21213,.T.);
#27740=ORIENTED_EDGE('',*,*,#21903,.F.);
#27741=ORIENTED_EDGE('',*,*,#21268,.T.);
#27742=ORIENTED_EDGE('',*,*,#21904,.F.);
#27743=ORIENTED_EDGE('',*,*,#21341,.T.);
#27744=ORIENTED_EDGE('',*,*,#21269,.T.);
#27745=ORIENTED_EDGE('',*,*,#21903,.T.);
#27746=ORIENTED_EDGE('',*,*,#21212,.T.);
#27747=ORIENTED_EDGE('',*,*,#21905,.F.);
#27748=ORIENTED_EDGE('',*,*,#21266,.T.);
#27749=ORIENTED_EDGE('',*,*,#21906,.T.);
#27750=ORIENTED_EDGE('',*,*,#21215,.T.);
#27751=ORIENTED_EDGE('',*,*,#21907,.F.);
#27752=ORIENTED_EDGE('',*,*,#21303,.T.);
#27753=ORIENTED_EDGE('',*,*,#21216,.T.);
#27754=ORIENTED_EDGE('',*,*,#21906,.F.);
#27755=ORIENTED_EDGE('',*,*,#21265,.T.);
#27756=ORIENTED_EDGE('',*,*,#21908,.F.);
#27757=ORIENTED_EDGE('',*,*,#21199,.T.);
#27758=ORIENTED_EDGE('',*,*,#21909,.F.);
#27759=ORIENTED_EDGE('',*,*,#21282,.T.);
#27760=ORIENTED_EDGE('',*,*,#21910,.F.);
#27761=ORIENTED_EDGE('',*,*,#21301,.T.);
#27762=ORIENTED_EDGE('',*,*,#21283,.T.);
#27763=ORIENTED_EDGE('',*,*,#21909,.T.);
#27764=ORIENTED_EDGE('',*,*,#21198,.T.);
#27765=ORIENTED_EDGE('',*,*,#21911,.F.);
#27766=ORIENTED_EDGE('',*,*,#21280,.T.);
#27767=ORIENTED_EDGE('',*,*,#21912,.T.);
#27768=ORIENTED_EDGE('',*,*,#21201,.T.);
#27769=ORIENTED_EDGE('',*,*,#21913,.F.);
#27770=ORIENTED_EDGE('',*,*,#21343,.T.);
#27771=ORIENTED_EDGE('',*,*,#21202,.T.);
#27772=ORIENTED_EDGE('',*,*,#21912,.F.);
#27773=ORIENTED_EDGE('',*,*,#21279,.T.);
#27774=ORIENTED_EDGE('',*,*,#21911,.T.);
#27775=ORIENTED_EDGE('',*,*,#21913,.T.);
#27776=ORIENTED_EDGE('',*,*,#21914,.T.);
#27777=ORIENTED_EDGE('',*,*,#21915,.T.);
#27778=ORIENTED_EDGE('',*,*,#21916,.T.);
#27779=ORIENTED_EDGE('',*,*,#21917,.F.);
#27780=ORIENTED_EDGE('',*,*,#21918,.T.);
#27781=ORIENTED_EDGE('',*,*,#21919,.T.);
#27782=ORIENTED_EDGE('',*,*,#21920,.T.);
#27783=ORIENTED_EDGE('',*,*,#21908,.T.);
#27784=ORIENTED_EDGE('',*,*,#21910,.T.);
#27785=ORIENTED_EDGE('',*,*,#21921,.F.);
#27786=ORIENTED_EDGE('',*,*,#21921,.T.);
#27787=ORIENTED_EDGE('',*,*,#21281,.F.);
#27788=ORIENTED_EDGE('',*,*,#21917,.T.);
#27789=ORIENTED_EDGE('',*,*,#21855,.T.);
#27790=ORIENTED_EDGE('',*,*,#21920,.F.);
#27791=ORIENTED_EDGE('',*,*,#21883,.F.);
#27792=ORIENTED_EDGE('',*,*,#21914,.F.);
#27793=ORIENTED_EDGE('',*,*,#21200,.T.);
#27794=ORIENTED_EDGE('',*,*,#21853,.T.);
#27795=ORIENTED_EDGE('',*,*,#21922,.T.);
#27796=ORIENTED_EDGE('',*,*,#21885,.T.);
#27797=ORIENTED_EDGE('',*,*,#21923,.F.);
#27798=ORIENTED_EDGE('',*,*,#21852,.T.);
#27799=ORIENTED_EDGE('',*,*,#21924,.T.);
#27800=ORIENTED_EDGE('',*,*,#21876,.F.);
#27801=ORIENTED_EDGE('',*,*,#21922,.F.);
#27802=ORIENTED_EDGE('',*,*,#21878,.T.);
#27803=ORIENTED_EDGE('',*,*,#21925,.T.);
#27804=ORIENTED_EDGE('',*,*,#21850,.F.);
#27805=ORIENTED_EDGE('',*,*,#21926,.T.);
#27806=ORIENTED_EDGE('',*,*,#21880,.T.);
#27807=ORIENTED_EDGE('',*,*,#21927,.T.);
#27808=ORIENTED_EDGE('',*,*,#21858,.F.);
#27809=ORIENTED_EDGE('',*,*,#21928,.F.);
#27810=ORIENTED_EDGE('',*,*,#21857,.T.);
#27811=ORIENTED_EDGE('',*,*,#21929,.T.);
#27812=ORIENTED_EDGE('',*,*,#21881,.T.);
#27813=ORIENTED_EDGE('',*,*,#21928,.T.);
#27814=ORIENTED_EDGE('',*,*,#21915,.F.);
#27815=ORIENTED_EDGE('',*,*,#21882,.F.);
#27816=ORIENTED_EDGE('',*,*,#21929,.F.);
#27817=ORIENTED_EDGE('',*,*,#21856,.T.);
#27818=ORIENTED_EDGE('',*,*,#21916,.F.);
#27819=ORIENTED_EDGE('',*,*,#21918,.F.);
#27820=ORIENTED_EDGE('',*,*,#21854,.T.);
#27821=ORIENTED_EDGE('',*,*,#21923,.T.);
#27822=ORIENTED_EDGE('',*,*,#21884,.T.);
#27823=ORIENTED_EDGE('',*,*,#21919,.F.);
#27824=ORIENTED_EDGE('',*,*,#21930,.T.);
#27825=ORIENTED_EDGE('',*,*,#21931,.T.);
#27826=ORIENTED_EDGE('',*,*,#21932,.T.);
#27827=ORIENTED_EDGE('',*,*,#21902,.T.);
#27828=ORIENTED_EDGE('',*,*,#21904,.T.);
#27829=ORIENTED_EDGE('',*,*,#21933,.F.);
#27830=ORIENTED_EDGE('',*,*,#21905,.T.);
#27831=ORIENTED_EDGE('',*,*,#21907,.T.);
#27832=ORIENTED_EDGE('',*,*,#21934,.T.);
#27833=ORIENTED_EDGE('',*,*,#21935,.T.);
#27834=ORIENTED_EDGE('',*,*,#21936,.T.);
#27835=ORIENTED_EDGE('',*,*,#21937,.F.);
#27836=ORIENTED_EDGE('',*,*,#21937,.T.);
#27837=ORIENTED_EDGE('',*,*,#21351,.F.);
#27838=ORIENTED_EDGE('',*,*,#21933,.T.);
#27839=ORIENTED_EDGE('',*,*,#21267,.T.);
#27840=ORIENTED_EDGE('',*,*,#21934,.F.);
#27841=ORIENTED_EDGE('',*,*,#21214,.F.);
#27842=ORIENTED_EDGE('',*,*,#21932,.F.);
#27843=ORIENTED_EDGE('',*,*,#21503,.T.);
#27844=ORIENTED_EDGE('',*,*,#21349,.T.);
#27845=ORIENTED_EDGE('',*,*,#21938,.F.);
#27846=ORIENTED_EDGE('',*,*,#21505,.T.);
#27847=ORIENTED_EDGE('',*,*,#21939,.F.);
#27848=ORIENTED_EDGE('',*,*,#21348,.F.);
#27849=ORIENTED_EDGE('',*,*,#21940,.T.);
#27850=ORIENTED_EDGE('',*,*,#21506,.T.);
#27851=ORIENTED_EDGE('',*,*,#21938,.T.);
#27852=ORIENTED_EDGE('',*,*,#21346,.T.);
#27853=ORIENTED_EDGE('',*,*,#21941,.T.);
#27854=ORIENTED_EDGE('',*,*,#21498,.F.);
#27855=ORIENTED_EDGE('',*,*,#21942,.T.);
#27856=ORIENTED_EDGE('',*,*,#21500,.F.);
#27857=ORIENTED_EDGE('',*,*,#21943,.T.);
#27858=ORIENTED_EDGE('',*,*,#21344,.T.);
#27859=ORIENTED_EDGE('',*,*,#21944,.F.);
#27860=ORIENTED_EDGE('',*,*,#21353,.T.);
#27861=ORIENTED_EDGE('',*,*,#21945,.T.);
#27862=ORIENTED_EDGE('',*,*,#21501,.T.);
#27863=ORIENTED_EDGE('',*,*,#21944,.T.);
#27864=ORIENTED_EDGE('',*,*,#21935,.F.);
#27865=ORIENTED_EDGE('',*,*,#21502,.F.);
#27866=ORIENTED_EDGE('',*,*,#21945,.F.);
#27867=ORIENTED_EDGE('',*,*,#21352,.T.);
#27868=ORIENTED_EDGE('',*,*,#21936,.F.);
#27869=ORIENTED_EDGE('',*,*,#21930,.F.);
#27870=ORIENTED_EDGE('',*,*,#21350,.T.);
#27871=ORIENTED_EDGE('',*,*,#21939,.T.);
#27872=ORIENTED_EDGE('',*,*,#21504,.T.);
#27873=ORIENTED_EDGE('',*,*,#21931,.F.);
#27874=ORIENTED_EDGE('',*,*,#21237,.T.);
#27875=ORIENTED_EDGE('',*,*,#21946,.F.);
#27876=ORIENTED_EDGE('',*,*,#21284,.T.);
#27877=ORIENTED_EDGE('',*,*,#21947,.F.);
#27878=ORIENTED_EDGE('',*,*,#21948,.F.);
#27879=ORIENTED_EDGE('',*,*,#21286,.F.);
#27880=ORIENTED_EDGE('',*,*,#21949,.F.);
#27881=ORIENTED_EDGE('',*,*,#21233,.F.);
#27882=ORIENTED_EDGE('',*,*,#21946,.T.);
#27883=ORIENTED_EDGE('',*,*,#21950,.T.);
#27884=ORIENTED_EDGE('',*,*,#21951,.T.);
#27885=ORIENTED_EDGE('',*,*,#21952,.T.);
#27886=ORIENTED_EDGE('',*,*,#21949,.T.);
#27887=ORIENTED_EDGE('',*,*,#21285,.T.);
#27888=ORIENTED_EDGE('',*,*,#21948,.T.);
#27889=ORIENTED_EDGE('',*,*,#21953,.T.);
#27890=ORIENTED_EDGE('',*,*,#21954,.T.);
#27891=ORIENTED_EDGE('',*,*,#21955,.T.);
#27892=ORIENTED_EDGE('',*,*,#21947,.T.);
#27893=ORIENTED_EDGE('',*,*,#21287,.T.);
#27894=ORIENTED_EDGE('',*,*,#21956,.T.);
#27895=ORIENTED_EDGE('',*,*,#21234,.T.);
#27896=ORIENTED_EDGE('',*,*,#21952,.F.);
#27897=ORIENTED_EDGE('',*,*,#21957,.F.);
#27898=ORIENTED_EDGE('',*,*,#21958,.F.);
#27899=ORIENTED_EDGE('',*,*,#21959,.F.);
#27900=ORIENTED_EDGE('',*,*,#21960,.F.);
#27901=ORIENTED_EDGE('',*,*,#21961,.F.);
#27902=ORIENTED_EDGE('',*,*,#21953,.F.);
#27903=ORIENTED_EDGE('',*,*,#21232,.T.);
#27904=ORIENTED_EDGE('',*,*,#21962,.T.);
#27905=ORIENTED_EDGE('',*,*,#21963,.T.);
#27906=ORIENTED_EDGE('',*,*,#21964,.T.);
#27907=ORIENTED_EDGE('',*,*,#21965,.T.);
#27908=ORIENTED_EDGE('',*,*,#21966,.T.);
#27909=ORIENTED_EDGE('',*,*,#21967,.T.);
#27910=ORIENTED_EDGE('',*,*,#21968,.T.);
#27911=ORIENTED_EDGE('',*,*,#21238,.T.);
#27912=ORIENTED_EDGE('',*,*,#21955,.F.);
#27913=ORIENTED_EDGE('',*,*,#21969,.T.);
#27914=ORIENTED_EDGE('',*,*,#21970,.F.);
#27915=ORIENTED_EDGE('',*,*,#21971,.T.);
#27916=ORIENTED_EDGE('',*,*,#21972,.F.);
#27917=ORIENTED_EDGE('',*,*,#21973,.T.);
#27918=ORIENTED_EDGE('',*,*,#21950,.F.);
#27919=ORIENTED_EDGE('',*,*,#21236,.T.);
#27920=ORIENTED_EDGE('',*,*,#21974,.T.);
#27921=ORIENTED_EDGE('',*,*,#21975,.F.);
#27922=ORIENTED_EDGE('',*,*,#21976,.T.);
#27923=ORIENTED_EDGE('',*,*,#21977,.F.);
#27924=ORIENTED_EDGE('',*,*,#21978,.T.);
#27925=ORIENTED_EDGE('',*,*,#21979,.F.);
#27926=ORIENTED_EDGE('',*,*,#21972,.T.);
#27927=ORIENTED_EDGE('',*,*,#21980,.T.);
#27928=ORIENTED_EDGE('',*,*,#21958,.T.);
#27929=ORIENTED_EDGE('',*,*,#21981,.T.);
#27930=ORIENTED_EDGE('',*,*,#21970,.T.);
#27931=ORIENTED_EDGE('',*,*,#21982,.T.);
#27932=ORIENTED_EDGE('',*,*,#21960,.T.);
#27933=ORIENTED_EDGE('',*,*,#21983,.T.);
#27934=ORIENTED_EDGE('',*,*,#21957,.T.);
#27935=ORIENTED_EDGE('',*,*,#21951,.F.);
#27936=ORIENTED_EDGE('',*,*,#21973,.F.);
#27937=ORIENTED_EDGE('',*,*,#21981,.F.);
#27938=ORIENTED_EDGE('',*,*,#21969,.F.);
#27939=ORIENTED_EDGE('',*,*,#21954,.F.);
#27940=ORIENTED_EDGE('',*,*,#21961,.T.);
#27941=ORIENTED_EDGE('',*,*,#21982,.F.);
#27942=ORIENTED_EDGE('',*,*,#21959,.T.);
#27943=ORIENTED_EDGE('',*,*,#21980,.F.);
#27944=ORIENTED_EDGE('',*,*,#21971,.F.);
#27945=ORIENTED_EDGE('',*,*,#21983,.F.);
#27946=ORIENTED_EDGE('',*,*,#21189,.F.);
#27947=ORIENTED_EDGE('',*,*,#21976,.F.);
#27948=ORIENTED_EDGE('',*,*,#21984,.F.);
#27949=ORIENTED_EDGE('',*,*,#21966,.F.);
#27950=ORIENTED_EDGE('',*,*,#21985,.F.);
#27951=ORIENTED_EDGE('',*,*,#21978,.F.);
#27952=ORIENTED_EDGE('',*,*,#21986,.F.);
#27953=ORIENTED_EDGE('',*,*,#21964,.F.);
#27954=ORIENTED_EDGE('',*,*,#21987,.F.);
#27955=ORIENTED_EDGE('',*,*,#21968,.F.);
#27956=ORIENTED_EDGE('',*,*,#21988,.F.);
#27957=ORIENTED_EDGE('',*,*,#21962,.F.);
#27958=ORIENTED_EDGE('',*,*,#21239,.F.);
#27959=ORIENTED_EDGE('',*,*,#21974,.F.);
#27960=ORIENTED_EDGE('',*,*,#21235,.F.);
#27961=ORIENTED_EDGE('',*,*,#21956,.F.);
#27962=ORIENTED_EDGE('',*,*,#21989,.F.);
#27963=ORIENTED_EDGE('',*,*,#21967,.F.);
#27964=ORIENTED_EDGE('',*,*,#21984,.T.);
#27965=ORIENTED_EDGE('',*,*,#21975,.T.);
#27966=ORIENTED_EDGE('',*,*,#21989,.T.);
#27967=ORIENTED_EDGE('',*,*,#21979,.T.);
#27968=ORIENTED_EDGE('',*,*,#21987,.T.);
#27969=ORIENTED_EDGE('',*,*,#21963,.F.);
#27970=ORIENTED_EDGE('',*,*,#21988,.T.);
#27971=ORIENTED_EDGE('',*,*,#21965,.F.);
#27972=ORIENTED_EDGE('',*,*,#21986,.T.);
#27973=ORIENTED_EDGE('',*,*,#21977,.T.);
#27974=ORIENTED_EDGE('',*,*,#21985,.T.);
#27975=ORIENTED_EDGE('',*,*,#21191,.T.);
#27976=ORIENTED_EDGE('',*,*,#21245,.T.);
#27977=ORIENTED_EDGE('',*,*,#21990,.F.);
#27978=ORIENTED_EDGE('',*,*,#21288,.T.);
#27979=ORIENTED_EDGE('',*,*,#21991,.F.);
#27980=ORIENTED_EDGE('',*,*,#21992,.F.);
#27981=ORIENTED_EDGE('',*,*,#21290,.F.);
#27982=ORIENTED_EDGE('',*,*,#21993,.F.);
#27983=ORIENTED_EDGE('',*,*,#21241,.F.);
#27984=ORIENTED_EDGE('',*,*,#21990,.T.);
#27985=ORIENTED_EDGE('',*,*,#21994,.T.);
#27986=ORIENTED_EDGE('',*,*,#21995,.T.);
#27987=ORIENTED_EDGE('',*,*,#21996,.T.);
#27988=ORIENTED_EDGE('',*,*,#21993,.T.);
#27989=ORIENTED_EDGE('',*,*,#21289,.T.);
#27990=ORIENTED_EDGE('',*,*,#21992,.T.);
#27991=ORIENTED_EDGE('',*,*,#21997,.T.);
#27992=ORIENTED_EDGE('',*,*,#21998,.T.);
#27993=ORIENTED_EDGE('',*,*,#21999,.T.);
#27994=ORIENTED_EDGE('',*,*,#21991,.T.);
#27995=ORIENTED_EDGE('',*,*,#21291,.T.);
#27996=ORIENTED_EDGE('',*,*,#22000,.T.);
#27997=ORIENTED_EDGE('',*,*,#21242,.T.);
#27998=ORIENTED_EDGE('',*,*,#21996,.F.);
#27999=ORIENTED_EDGE('',*,*,#22001,.F.);
#28000=ORIENTED_EDGE('',*,*,#22002,.F.);
#28001=ORIENTED_EDGE('',*,*,#22003,.F.);
#28002=ORIENTED_EDGE('',*,*,#22004,.F.);
#28003=ORIENTED_EDGE('',*,*,#22005,.F.);
#28004=ORIENTED_EDGE('',*,*,#21997,.F.);
#28005=ORIENTED_EDGE('',*,*,#21240,.T.);
#28006=ORIENTED_EDGE('',*,*,#22006,.T.);
#28007=ORIENTED_EDGE('',*,*,#22007,.T.);
#28008=ORIENTED_EDGE('',*,*,#22008,.T.);
#28009=ORIENTED_EDGE('',*,*,#22009,.T.);
#28010=ORIENTED_EDGE('',*,*,#22010,.T.);
#28011=ORIENTED_EDGE('',*,*,#22011,.T.);
#28012=ORIENTED_EDGE('',*,*,#22012,.T.);
#28013=ORIENTED_EDGE('',*,*,#21246,.T.);
#28014=ORIENTED_EDGE('',*,*,#21999,.F.);
#28015=ORIENTED_EDGE('',*,*,#22013,.T.);
#28016=ORIENTED_EDGE('',*,*,#22014,.F.);
#28017=ORIENTED_EDGE('',*,*,#22015,.T.);
#28018=ORIENTED_EDGE('',*,*,#22016,.F.);
#28019=ORIENTED_EDGE('',*,*,#22017,.T.);
#28020=ORIENTED_EDGE('',*,*,#21994,.F.);
#28021=ORIENTED_EDGE('',*,*,#21244,.T.);
#28022=ORIENTED_EDGE('',*,*,#22018,.T.);
#28023=ORIENTED_EDGE('',*,*,#22019,.F.);
#28024=ORIENTED_EDGE('',*,*,#22020,.T.);
#28025=ORIENTED_EDGE('',*,*,#22021,.F.);
#28026=ORIENTED_EDGE('',*,*,#22022,.T.);
#28027=ORIENTED_EDGE('',*,*,#22023,.F.);
#28028=ORIENTED_EDGE('',*,*,#22016,.T.);
#28029=ORIENTED_EDGE('',*,*,#22024,.T.);
#28030=ORIENTED_EDGE('',*,*,#22002,.T.);
#28031=ORIENTED_EDGE('',*,*,#22025,.T.);
#28032=ORIENTED_EDGE('',*,*,#22014,.T.);
#28033=ORIENTED_EDGE('',*,*,#22026,.T.);
#28034=ORIENTED_EDGE('',*,*,#22004,.T.);
#28035=ORIENTED_EDGE('',*,*,#22027,.T.);
#28036=ORIENTED_EDGE('',*,*,#22001,.T.);
#28037=ORIENTED_EDGE('',*,*,#21995,.F.);
#28038=ORIENTED_EDGE('',*,*,#22017,.F.);
#28039=ORIENTED_EDGE('',*,*,#22025,.F.);
#28040=ORIENTED_EDGE('',*,*,#22013,.F.);
#28041=ORIENTED_EDGE('',*,*,#21998,.F.);
#28042=ORIENTED_EDGE('',*,*,#22005,.T.);
#28043=ORIENTED_EDGE('',*,*,#22026,.F.);
#28044=ORIENTED_EDGE('',*,*,#22003,.T.);
#28045=ORIENTED_EDGE('',*,*,#22024,.F.);
#28046=ORIENTED_EDGE('',*,*,#22015,.F.);
#28047=ORIENTED_EDGE('',*,*,#22027,.F.);
#28048=ORIENTED_EDGE('',*,*,#21186,.F.);
#28049=ORIENTED_EDGE('',*,*,#22020,.F.);
#28050=ORIENTED_EDGE('',*,*,#22028,.F.);
#28051=ORIENTED_EDGE('',*,*,#22010,.F.);
#28052=ORIENTED_EDGE('',*,*,#22029,.F.);
#28053=ORIENTED_EDGE('',*,*,#22022,.F.);
#28054=ORIENTED_EDGE('',*,*,#22030,.F.);
#28055=ORIENTED_EDGE('',*,*,#22008,.F.);
#28056=ORIENTED_EDGE('',*,*,#22031,.F.);
#28057=ORIENTED_EDGE('',*,*,#22012,.F.);
#28058=ORIENTED_EDGE('',*,*,#22032,.F.);
#28059=ORIENTED_EDGE('',*,*,#22006,.F.);
#28060=ORIENTED_EDGE('',*,*,#21247,.F.);
#28061=ORIENTED_EDGE('',*,*,#22018,.F.);
#28062=ORIENTED_EDGE('',*,*,#21243,.F.);
#28063=ORIENTED_EDGE('',*,*,#22000,.F.);
#28064=ORIENTED_EDGE('',*,*,#22033,.F.);
#28065=ORIENTED_EDGE('',*,*,#22011,.F.);
#28066=ORIENTED_EDGE('',*,*,#22028,.T.);
#28067=ORIENTED_EDGE('',*,*,#22019,.T.);
#28068=ORIENTED_EDGE('',*,*,#22033,.T.);
#28069=ORIENTED_EDGE('',*,*,#22023,.T.);
#28070=ORIENTED_EDGE('',*,*,#22031,.T.);
#28071=ORIENTED_EDGE('',*,*,#22007,.F.);
#28072=ORIENTED_EDGE('',*,*,#22032,.T.);
#28073=ORIENTED_EDGE('',*,*,#22009,.F.);
#28074=ORIENTED_EDGE('',*,*,#22030,.T.);
#28075=ORIENTED_EDGE('',*,*,#22021,.T.);
#28076=ORIENTED_EDGE('',*,*,#22029,.T.);
#28077=ORIENTED_EDGE('',*,*,#21188,.T.);
#28078=ORIENTED_EDGE('',*,*,#21229,.T.);
#28079=ORIENTED_EDGE('',*,*,#22034,.F.);
#28080=ORIENTED_EDGE('',*,*,#21292,.T.);
#28081=ORIENTED_EDGE('',*,*,#22035,.F.);
#28082=ORIENTED_EDGE('',*,*,#22036,.F.);
#28083=ORIENTED_EDGE('',*,*,#21294,.F.);
#28084=ORIENTED_EDGE('',*,*,#22037,.F.);
#28085=ORIENTED_EDGE('',*,*,#21225,.F.);
#28086=ORIENTED_EDGE('',*,*,#22034,.T.);
#28087=ORIENTED_EDGE('',*,*,#22038,.T.);
#28088=ORIENTED_EDGE('',*,*,#22039,.T.);
#28089=ORIENTED_EDGE('',*,*,#22040,.T.);
#28090=ORIENTED_EDGE('',*,*,#22037,.T.);
#28091=ORIENTED_EDGE('',*,*,#21293,.T.);
#28092=ORIENTED_EDGE('',*,*,#22036,.T.);
#28093=ORIENTED_EDGE('',*,*,#22041,.T.);
#28094=ORIENTED_EDGE('',*,*,#22042,.T.);
#28095=ORIENTED_EDGE('',*,*,#22043,.T.);
#28096=ORIENTED_EDGE('',*,*,#22035,.T.);
#28097=ORIENTED_EDGE('',*,*,#21295,.T.);
#28098=ORIENTED_EDGE('',*,*,#22044,.T.);
#28099=ORIENTED_EDGE('',*,*,#21226,.T.);
#28100=ORIENTED_EDGE('',*,*,#22040,.F.);
#28101=ORIENTED_EDGE('',*,*,#22045,.F.);
#28102=ORIENTED_EDGE('',*,*,#22046,.F.);
#28103=ORIENTED_EDGE('',*,*,#22047,.F.);
#28104=ORIENTED_EDGE('',*,*,#22048,.F.);
#28105=ORIENTED_EDGE('',*,*,#22049,.F.);
#28106=ORIENTED_EDGE('',*,*,#22041,.F.);
#28107=ORIENTED_EDGE('',*,*,#21224,.T.);
#28108=ORIENTED_EDGE('',*,*,#22050,.T.);
#28109=ORIENTED_EDGE('',*,*,#22051,.T.);
#28110=ORIENTED_EDGE('',*,*,#22052,.T.);
#28111=ORIENTED_EDGE('',*,*,#22053,.T.);
#28112=ORIENTED_EDGE('',*,*,#22054,.T.);
#28113=ORIENTED_EDGE('',*,*,#22055,.T.);
#28114=ORIENTED_EDGE('',*,*,#22056,.T.);
#28115=ORIENTED_EDGE('',*,*,#21230,.T.);
#28116=ORIENTED_EDGE('',*,*,#22043,.F.);
#28117=ORIENTED_EDGE('',*,*,#22057,.T.);
#28118=ORIENTED_EDGE('',*,*,#22058,.F.);
#28119=ORIENTED_EDGE('',*,*,#22059,.T.);
#28120=ORIENTED_EDGE('',*,*,#22060,.F.);
#28121=ORIENTED_EDGE('',*,*,#22061,.T.);
#28122=ORIENTED_EDGE('',*,*,#22038,.F.);
#28123=ORIENTED_EDGE('',*,*,#21228,.T.);
#28124=ORIENTED_EDGE('',*,*,#22062,.T.);
#28125=ORIENTED_EDGE('',*,*,#22063,.F.);
#28126=ORIENTED_EDGE('',*,*,#22064,.T.);
#28127=ORIENTED_EDGE('',*,*,#22065,.F.);
#28128=ORIENTED_EDGE('',*,*,#22066,.T.);
#28129=ORIENTED_EDGE('',*,*,#22067,.F.);
#28130=ORIENTED_EDGE('',*,*,#22060,.T.);
#28131=ORIENTED_EDGE('',*,*,#22068,.T.);
#28132=ORIENTED_EDGE('',*,*,#22046,.T.);
#28133=ORIENTED_EDGE('',*,*,#22069,.T.);
#28134=ORIENTED_EDGE('',*,*,#22058,.T.);
#28135=ORIENTED_EDGE('',*,*,#22070,.T.);
#28136=ORIENTED_EDGE('',*,*,#22048,.T.);
#28137=ORIENTED_EDGE('',*,*,#22071,.T.);
#28138=ORIENTED_EDGE('',*,*,#22045,.T.);
#28139=ORIENTED_EDGE('',*,*,#22039,.F.);
#28140=ORIENTED_EDGE('',*,*,#22061,.F.);
#28141=ORIENTED_EDGE('',*,*,#22069,.F.);
#28142=ORIENTED_EDGE('',*,*,#22057,.F.);
#28143=ORIENTED_EDGE('',*,*,#22042,.F.);
#28144=ORIENTED_EDGE('',*,*,#22049,.T.);
#28145=ORIENTED_EDGE('',*,*,#22070,.F.);
#28146=ORIENTED_EDGE('',*,*,#22047,.T.);
#28147=ORIENTED_EDGE('',*,*,#22068,.F.);
#28148=ORIENTED_EDGE('',*,*,#22059,.F.);
#28149=ORIENTED_EDGE('',*,*,#22071,.F.);
#28150=ORIENTED_EDGE('',*,*,#21183,.F.);
#28151=ORIENTED_EDGE('',*,*,#22064,.F.);
#28152=ORIENTED_EDGE('',*,*,#22072,.F.);
#28153=ORIENTED_EDGE('',*,*,#22054,.F.);
#28154=ORIENTED_EDGE('',*,*,#22073,.F.);
#28155=ORIENTED_EDGE('',*,*,#22066,.F.);
#28156=ORIENTED_EDGE('',*,*,#22074,.F.);
#28157=ORIENTED_EDGE('',*,*,#22052,.F.);
#28158=ORIENTED_EDGE('',*,*,#22075,.F.);
#28159=ORIENTED_EDGE('',*,*,#22056,.F.);
#28160=ORIENTED_EDGE('',*,*,#22076,.F.);
#28161=ORIENTED_EDGE('',*,*,#22050,.F.);
#28162=ORIENTED_EDGE('',*,*,#21231,.F.);
#28163=ORIENTED_EDGE('',*,*,#22062,.F.);
#28164=ORIENTED_EDGE('',*,*,#21227,.F.);
#28165=ORIENTED_EDGE('',*,*,#22044,.F.);
#28166=ORIENTED_EDGE('',*,*,#22077,.F.);
#28167=ORIENTED_EDGE('',*,*,#22055,.F.);
#28168=ORIENTED_EDGE('',*,*,#22072,.T.);
#28169=ORIENTED_EDGE('',*,*,#22063,.T.);
#28170=ORIENTED_EDGE('',*,*,#22077,.T.);
#28171=ORIENTED_EDGE('',*,*,#22067,.T.);
#28172=ORIENTED_EDGE('',*,*,#22075,.T.);
#28173=ORIENTED_EDGE('',*,*,#22051,.F.);
#28174=ORIENTED_EDGE('',*,*,#22076,.T.);
#28175=ORIENTED_EDGE('',*,*,#22053,.F.);
#28176=ORIENTED_EDGE('',*,*,#22074,.T.);
#28177=ORIENTED_EDGE('',*,*,#22065,.T.);
#28178=ORIENTED_EDGE('',*,*,#22073,.T.);
#28179=ORIENTED_EDGE('',*,*,#21185,.T.);
#28180=ORIENTED_EDGE('',*,*,#21253,.T.);
#28181=ORIENTED_EDGE('',*,*,#22078,.F.);
#28182=ORIENTED_EDGE('',*,*,#21296,.T.);
#28183=ORIENTED_EDGE('',*,*,#22079,.F.);
#28184=ORIENTED_EDGE('',*,*,#22080,.F.);
#28185=ORIENTED_EDGE('',*,*,#21298,.F.);
#28186=ORIENTED_EDGE('',*,*,#22081,.F.);
#28187=ORIENTED_EDGE('',*,*,#21249,.F.);
#28188=ORIENTED_EDGE('',*,*,#22078,.T.);
#28189=ORIENTED_EDGE('',*,*,#22082,.T.);
#28190=ORIENTED_EDGE('',*,*,#22083,.T.);
#28191=ORIENTED_EDGE('',*,*,#22084,.T.);
#28192=ORIENTED_EDGE('',*,*,#22081,.T.);
#28193=ORIENTED_EDGE('',*,*,#21297,.T.);
#28194=ORIENTED_EDGE('',*,*,#22080,.T.);
#28195=ORIENTED_EDGE('',*,*,#22085,.T.);
#28196=ORIENTED_EDGE('',*,*,#22086,.T.);
#28197=ORIENTED_EDGE('',*,*,#22087,.T.);
#28198=ORIENTED_EDGE('',*,*,#22079,.T.);
#28199=ORIENTED_EDGE('',*,*,#21299,.T.);
#28200=ORIENTED_EDGE('',*,*,#22088,.T.);
#28201=ORIENTED_EDGE('',*,*,#21250,.T.);
#28202=ORIENTED_EDGE('',*,*,#22084,.F.);
#28203=ORIENTED_EDGE('',*,*,#22089,.F.);
#28204=ORIENTED_EDGE('',*,*,#22090,.F.);
#28205=ORIENTED_EDGE('',*,*,#22091,.F.);
#28206=ORIENTED_EDGE('',*,*,#22092,.F.);
#28207=ORIENTED_EDGE('',*,*,#22093,.F.);
#28208=ORIENTED_EDGE('',*,*,#22085,.F.);
#28209=ORIENTED_EDGE('',*,*,#21248,.T.);
#28210=ORIENTED_EDGE('',*,*,#22094,.T.);
#28211=ORIENTED_EDGE('',*,*,#22095,.T.);
#28212=ORIENTED_EDGE('',*,*,#22096,.T.);
#28213=ORIENTED_EDGE('',*,*,#22097,.T.);
#28214=ORIENTED_EDGE('',*,*,#22098,.T.);
#28215=ORIENTED_EDGE('',*,*,#22099,.T.);
#28216=ORIENTED_EDGE('',*,*,#22100,.T.);
#28217=ORIENTED_EDGE('',*,*,#21254,.T.);
#28218=ORIENTED_EDGE('',*,*,#22087,.F.);
#28219=ORIENTED_EDGE('',*,*,#22101,.T.);
#28220=ORIENTED_EDGE('',*,*,#22102,.F.);
#28221=ORIENTED_EDGE('',*,*,#22103,.T.);
#28222=ORIENTED_EDGE('',*,*,#22104,.F.);
#28223=ORIENTED_EDGE('',*,*,#22105,.T.);
#28224=ORIENTED_EDGE('',*,*,#22082,.F.);
#28225=ORIENTED_EDGE('',*,*,#21252,.T.);
#28226=ORIENTED_EDGE('',*,*,#22106,.T.);
#28227=ORIENTED_EDGE('',*,*,#22107,.F.);
#28228=ORIENTED_EDGE('',*,*,#22108,.T.);
#28229=ORIENTED_EDGE('',*,*,#22109,.F.);
#28230=ORIENTED_EDGE('',*,*,#22110,.T.);
#28231=ORIENTED_EDGE('',*,*,#22111,.F.);
#28232=ORIENTED_EDGE('',*,*,#22104,.T.);
#28233=ORIENTED_EDGE('',*,*,#22112,.T.);
#28234=ORIENTED_EDGE('',*,*,#22090,.T.);
#28235=ORIENTED_EDGE('',*,*,#22113,.T.);
#28236=ORIENTED_EDGE('',*,*,#22102,.T.);
#28237=ORIENTED_EDGE('',*,*,#22114,.T.);
#28238=ORIENTED_EDGE('',*,*,#22092,.T.);
#28239=ORIENTED_EDGE('',*,*,#22115,.T.);
#28240=ORIENTED_EDGE('',*,*,#22089,.T.);
#28241=ORIENTED_EDGE('',*,*,#22083,.F.);
#28242=ORIENTED_EDGE('',*,*,#22105,.F.);
#28243=ORIENTED_EDGE('',*,*,#22113,.F.);
#28244=ORIENTED_EDGE('',*,*,#22101,.F.);
#28245=ORIENTED_EDGE('',*,*,#22086,.F.);
#28246=ORIENTED_EDGE('',*,*,#22093,.T.);
#28247=ORIENTED_EDGE('',*,*,#22114,.F.);
#28248=ORIENTED_EDGE('',*,*,#22091,.T.);
#28249=ORIENTED_EDGE('',*,*,#22112,.F.);
#28250=ORIENTED_EDGE('',*,*,#22103,.F.);
#28251=ORIENTED_EDGE('',*,*,#22115,.F.);
#28252=ORIENTED_EDGE('',*,*,#21180,.F.);
#28253=ORIENTED_EDGE('',*,*,#22108,.F.);
#28254=ORIENTED_EDGE('',*,*,#22116,.F.);
#28255=ORIENTED_EDGE('',*,*,#22098,.F.);
#28256=ORIENTED_EDGE('',*,*,#22117,.F.);
#28257=ORIENTED_EDGE('',*,*,#22110,.F.);
#28258=ORIENTED_EDGE('',*,*,#22118,.F.);
#28259=ORIENTED_EDGE('',*,*,#22096,.F.);
#28260=ORIENTED_EDGE('',*,*,#22119,.F.);
#28261=ORIENTED_EDGE('',*,*,#22100,.F.);
#28262=ORIENTED_EDGE('',*,*,#22120,.F.);
#28263=ORIENTED_EDGE('',*,*,#22094,.F.);
#28264=ORIENTED_EDGE('',*,*,#21255,.F.);
#28265=ORIENTED_EDGE('',*,*,#22106,.F.);
#28266=ORIENTED_EDGE('',*,*,#21251,.F.);
#28267=ORIENTED_EDGE('',*,*,#22088,.F.);
#28268=ORIENTED_EDGE('',*,*,#22121,.F.);
#28269=ORIENTED_EDGE('',*,*,#22099,.F.);
#28270=ORIENTED_EDGE('',*,*,#22116,.T.);
#28271=ORIENTED_EDGE('',*,*,#22107,.T.);
#28272=ORIENTED_EDGE('',*,*,#22121,.T.);
#28273=ORIENTED_EDGE('',*,*,#22111,.T.);
#28274=ORIENTED_EDGE('',*,*,#22119,.T.);
#28275=ORIENTED_EDGE('',*,*,#22095,.F.);
#28276=ORIENTED_EDGE('',*,*,#22120,.T.);
#28277=ORIENTED_EDGE('',*,*,#22097,.F.);
#28278=ORIENTED_EDGE('',*,*,#22118,.T.);
#28279=ORIENTED_EDGE('',*,*,#22109,.T.);
#28280=ORIENTED_EDGE('',*,*,#22117,.T.);
#28281=ORIENTED_EDGE('',*,*,#21182,.T.);
#28282=ORIENTED_EDGE('',*,*,#21176,.T.);
#28283=ORIENTED_EDGE('',*,*,#21148,.T.);
#28284=ORIENTED_EDGE('',*,*,#22122,.T.);
#28285=ORIENTED_EDGE('',*,*,#21088,.T.);
#28286=ORIENTED_EDGE('',*,*,#21842,.T.);
#28287=ORIENTED_EDGE('',*,*,#22123,.T.);
#28288=ORIENTED_EDGE('',*,*,#21140,.T.);
#28289=ORIENTED_EDGE('',*,*,#22124,.T.);
#28290=ORIENTED_EDGE('',*,*,#22125,.T.);
#28291=ORIENTED_EDGE('',*,*,#22126,.T.);
#28292=ORIENTED_EDGE('',*,*,#22127,.T.);
#28293=ORIENTED_EDGE('',*,*,#22128,.T.);
#28294=ORIENTED_EDGE('',*,*,#22129,.T.);
#28295=ORIENTED_EDGE('',*,*,#22130,.T.);
#28296=ORIENTED_EDGE('',*,*,#21068,.T.);
#28297=ORIENTED_EDGE('',*,*,#22131,.T.);
#28298=ORIENTED_EDGE('',*,*,#22132,.T.);
#28299=ORIENTED_EDGE('',*,*,#22133,.T.);
#28300=ORIENTED_EDGE('',*,*,#22134,.T.);
#28301=ORIENTED_EDGE('',*,*,#22135,.T.);
#28302=ORIENTED_EDGE('',*,*,#22136,.T.);
#28303=ORIENTED_EDGE('',*,*,#22137,.T.);
#28304=ORIENTED_EDGE('',*,*,#22138,.T.);
#28305=ORIENTED_EDGE('',*,*,#22139,.T.);
#28306=ORIENTED_EDGE('',*,*,#21072,.T.);
#28307=ORIENTED_EDGE('',*,*,#22140,.T.);
#28308=ORIENTED_EDGE('',*,*,#22141,.T.);
#28309=ORIENTED_EDGE('',*,*,#22142,.T.);
#28310=ORIENTED_EDGE('',*,*,#22143,.T.);
#28311=ORIENTED_EDGE('',*,*,#22144,.T.);
#28312=ORIENTED_EDGE('',*,*,#22145,.T.);
#28313=ORIENTED_EDGE('',*,*,#22146,.T.);
#28314=ORIENTED_EDGE('',*,*,#22147,.T.);
#28315=ORIENTED_EDGE('',*,*,#22148,.T.);
#28316=ORIENTED_EDGE('',*,*,#21084,.T.);
#28317=ORIENTED_EDGE('',*,*,#22149,.T.);
#28318=ORIENTED_EDGE('',*,*,#22150,.T.);
#28319=ORIENTED_EDGE('',*,*,#22151,.T.);
#28320=ORIENTED_EDGE('',*,*,#22152,.T.);
#28321=ORIENTED_EDGE('',*,*,#22153,.T.);
#28322=ORIENTED_EDGE('',*,*,#22154,.T.);
#28323=ORIENTED_EDGE('',*,*,#22155,.T.);
#28324=ORIENTED_EDGE('',*,*,#21080,.T.);
#28325=ORIENTED_EDGE('',*,*,#22156,.T.);
#28326=ORIENTED_EDGE('',*,*,#21076,.T.);
#28327=ORIENTED_EDGE('',*,*,#22157,.T.);
#28328=ORIENTED_EDGE('',*,*,#22158,.T.);
#28329=ORIENTED_EDGE('',*,*,#22159,.T.);
#28330=ORIENTED_EDGE('',*,*,#22160,.T.);
#28331=ORIENTED_EDGE('',*,*,#22161,.T.);
#28332=ORIENTED_EDGE('',*,*,#22162,.T.);
#28333=ORIENTED_EDGE('',*,*,#21156,.T.);
#28334=ORIENTED_EDGE('',*,*,#22163,.T.);
#28335=ORIENTED_EDGE('',*,*,#21112,.T.);
#28336=ORIENTED_EDGE('',*,*,#21652,.T.);
#28337=ORIENTED_EDGE('',*,*,#22164,.T.);
#28338=ORIENTED_EDGE('',*,*,#21144,.T.);
#28339=ORIENTED_EDGE('',*,*,#22165,.T.);
#28340=ORIENTED_EDGE('',*,*,#22166,.T.);
#28341=ORIENTED_EDGE('',*,*,#21681,.T.);
#28342=ORIENTED_EDGE('',*,*,#22167,.T.);
#28343=ORIENTED_EDGE('',*,*,#22168,.T.);
#28344=ORIENTED_EDGE('',*,*,#22169,.T.);
#28345=ORIENTED_EDGE('',*,*,#21683,.T.);
#28346=ORIENTED_EDGE('',*,*,#21092,.T.);
#28347=ORIENTED_EDGE('',*,*,#22170,.T.);
#28348=ORIENTED_EDGE('',*,*,#22171,.T.);
#28349=ORIENTED_EDGE('',*,*,#21688,.T.);
#28350=ORIENTED_EDGE('',*,*,#22172,.T.);
#28351=ORIENTED_EDGE('',*,*,#22173,.T.);
#28352=ORIENTED_EDGE('',*,*,#22174,.T.);
#28353=ORIENTED_EDGE('',*,*,#21692,.T.);
#28354=ORIENTED_EDGE('',*,*,#22175,.T.);
#28355=ORIENTED_EDGE('',*,*,#22176,.T.);
#28356=ORIENTED_EDGE('',*,*,#21096,.T.);
#28357=ORIENTED_EDGE('',*,*,#21657,.T.);
#28358=ORIENTED_EDGE('',*,*,#22177,.T.);
#28359=ORIENTED_EDGE('',*,*,#22178,.T.);
#28360=ORIENTED_EDGE('',*,*,#22179,.T.);
#28361=ORIENTED_EDGE('',*,*,#21658,.T.);
#28362=ORIENTED_EDGE('',*,*,#22180,.T.);
#28363=ORIENTED_EDGE('',*,*,#22181,.T.);
#28364=ORIENTED_EDGE('',*,*,#22182,.T.);
#28365=ORIENTED_EDGE('',*,*,#21663,.T.);
#28366=ORIENTED_EDGE('',*,*,#21108,.T.);
#28367=ORIENTED_EDGE('',*,*,#22183,.T.);
#28368=ORIENTED_EDGE('',*,*,#22184,.T.);
#28369=ORIENTED_EDGE('',*,*,#21665,.T.);
#28370=ORIENTED_EDGE('',*,*,#22185,.T.);
#28371=ORIENTED_EDGE('',*,*,#22186,.T.);
#28372=ORIENTED_EDGE('',*,*,#22187,.T.);
#28373=ORIENTED_EDGE('',*,*,#21670,.T.);
#28374=ORIENTED_EDGE('',*,*,#21104,.T.);
#28375=ORIENTED_EDGE('',*,*,#22188,.T.);
#28376=ORIENTED_EDGE('',*,*,#21100,.T.);
#28377=ORIENTED_EDGE('',*,*,#21672,.T.);
#28378=ORIENTED_EDGE('',*,*,#22189,.T.);
#28379=ORIENTED_EDGE('',*,*,#22190,.T.);
#28380=ORIENTED_EDGE('',*,*,#22191,.T.);
#28381=ORIENTED_EDGE('',*,*,#21677,.T.);
#28382=ORIENTED_EDGE('',*,*,#22192,.T.);
#28383=ORIENTED_EDGE('',*,*,#21194,.T.);
#28384=ORIENTED_EDGE('',*,*,#21841,.T.);
#28385=ORIENTED_EDGE('',*,*,#21124,.T.);
#28386=ORIENTED_EDGE('',*,*,#21694,.T.);
#28387=ORIENTED_EDGE('',*,*,#22193,.T.);
#28388=ORIENTED_EDGE('',*,*,#21152,.T.);
#28389=ORIENTED_EDGE('',*,*,#22194,.T.);
#28390=ORIENTED_EDGE('',*,*,#22195,.T.);
#28391=ORIENTED_EDGE('',*,*,#21723,.T.);
#28392=ORIENTED_EDGE('',*,*,#22196,.T.);
#28393=ORIENTED_EDGE('',*,*,#21738,.T.);
#28394=ORIENTED_EDGE('',*,*,#22197,.T.);
#28395=ORIENTED_EDGE('',*,*,#21725,.T.);
#28396=ORIENTED_EDGE('',*,*,#21116,.T.);
#28397=ORIENTED_EDGE('',*,*,#22198,.T.);
#28398=ORIENTED_EDGE('',*,*,#22199,.T.);
#28399=ORIENTED_EDGE('',*,*,#21730,.T.);
#28400=ORIENTED_EDGE('',*,*,#22200,.T.);
#28401=ORIENTED_EDGE('',*,*,#22201,.T.);
#28402=ORIENTED_EDGE('',*,*,#22202,.T.);
#28403=ORIENTED_EDGE('',*,*,#21734,.T.);
#28404=ORIENTED_EDGE('',*,*,#22203,.T.);
#28405=ORIENTED_EDGE('',*,*,#22204,.T.);
#28406=ORIENTED_EDGE('',*,*,#21120,.T.);
#28407=ORIENTED_EDGE('',*,*,#21699,.T.);
#28408=ORIENTED_EDGE('',*,*,#22205,.T.);
#28409=ORIENTED_EDGE('',*,*,#21849,.T.);
#28410=ORIENTED_EDGE('',*,*,#22206,.T.);
#28411=ORIENTED_EDGE('',*,*,#21700,.T.);
#28412=ORIENTED_EDGE('',*,*,#22207,.T.);
#28413=ORIENTED_EDGE('',*,*,#22208,.T.);
#28414=ORIENTED_EDGE('',*,*,#22209,.T.);
#28415=ORIENTED_EDGE('',*,*,#21705,.T.);
#28416=ORIENTED_EDGE('',*,*,#21136,.T.);
#28417=ORIENTED_EDGE('',*,*,#21847,.T.);
#28418=ORIENTED_EDGE('',*,*,#22210,.T.);
#28419=ORIENTED_EDGE('',*,*,#21707,.T.);
#28420=ORIENTED_EDGE('',*,*,#22211,.T.);
#28421=ORIENTED_EDGE('',*,*,#22212,.T.);
#28422=ORIENTED_EDGE('',*,*,#22213,.T.);
#28423=ORIENTED_EDGE('',*,*,#21712,.T.);
#28424=ORIENTED_EDGE('',*,*,#21132,.T.);
#28425=ORIENTED_EDGE('',*,*,#21844,.T.);
#28426=ORIENTED_EDGE('',*,*,#21128,.T.);
#28427=ORIENTED_EDGE('',*,*,#21714,.T.);
#28428=ORIENTED_EDGE('',*,*,#22214,.T.);
#28429=ORIENTED_EDGE('',*,*,#22215,.T.);
#28430=ORIENTED_EDGE('',*,*,#22216,.T.);
#28431=ORIENTED_EDGE('',*,*,#21719,.T.);
#28432=ORIENTED_EDGE('',*,*,#22217,.T.);
#28433=ORIENTED_EDGE('',*,*,#22201,.F.);
#28434=ORIENTED_EDGE('',*,*,#22218,.T.);
#28435=ORIENTED_EDGE('',*,*,#21819,.T.);
#28436=ORIENTED_EDGE('',*,*,#22219,.T.);
#28437=ORIENTED_EDGE('',*,*,#21759,.F.);
#28438=ORIENTED_EDGE('',*,*,#22220,.T.);
#28439=ORIENTED_EDGE('',*,*,#22140,.F.);
#28440=ORIENTED_EDGE('',*,*,#21071,.T.);
#28441=ORIENTED_EDGE('',*,*,#22144,.F.);
#28442=ORIENTED_EDGE('',*,*,#22221,.T.);
#28443=ORIENTED_EDGE('',*,*,#21770,.F.);
#28444=ORIENTED_EDGE('',*,*,#22222,.T.);
#28445=ORIENTED_EDGE('',*,*,#21766,.F.);
#28446=ORIENTED_EDGE('',*,*,#21085,.T.);
#28447=ORIENTED_EDGE('',*,*,#22148,.F.);
#28448=ORIENTED_EDGE('',*,*,#22223,.T.);
#28449=ORIENTED_EDGE('',*,*,#22151,.F.);
#28450=ORIENTED_EDGE('',*,*,#22224,.T.);
#28451=ORIENTED_EDGE('',*,*,#21777,.F.);
#28452=ORIENTED_EDGE('',*,*,#22225,.T.);
#28453=ORIENTED_EDGE('',*,*,#21773,.F.);
#28454=ORIENTED_EDGE('',*,*,#21081,.T.);
#28455=ORIENTED_EDGE('',*,*,#22155,.F.);
#28456=ORIENTED_EDGE('',*,*,#22226,.T.);
#28457=ORIENTED_EDGE('',*,*,#22157,.F.);
#28458=ORIENTED_EDGE('',*,*,#21075,.T.);
#28459=ORIENTED_EDGE('',*,*,#21784,.F.);
#28460=ORIENTED_EDGE('',*,*,#22227,.T.);
#28461=ORIENTED_EDGE('',*,*,#21780,.F.);
#28462=ORIENTED_EDGE('',*,*,#22228,.T.);
#28463=ORIENTED_EDGE('',*,*,#22161,.F.);
#28464=ORIENTED_EDGE('',*,*,#22229,.T.);
#28465=ORIENTED_EDGE('',*,*,#21746,.F.);
#28466=ORIENTED_EDGE('',*,*,#22230,.T.);
#28467=ORIENTED_EDGE('',*,*,#22126,.F.);
#28468=ORIENTED_EDGE('',*,*,#22231,.T.);
#28469=ORIENTED_EDGE('',*,*,#22130,.F.);
#28470=ORIENTED_EDGE('',*,*,#22232,.T.);
#28471=ORIENTED_EDGE('',*,*,#21755,.F.);
#28472=ORIENTED_EDGE('',*,*,#21069,.T.);
#28473=ORIENTED_EDGE('',*,*,#21752,.F.);
#28474=ORIENTED_EDGE('',*,*,#22233,.T.);
#28475=ORIENTED_EDGE('',*,*,#22133,.F.);
#28476=ORIENTED_EDGE('',*,*,#22234,.T.);
#28477=ORIENTED_EDGE('',*,*,#21762,.F.);
#28478=ORIENTED_EDGE('',*,*,#22235,.T.);
#28479=ORIENTED_EDGE('',*,*,#22137,.F.);
#28480=ORIENTED_EDGE('',*,*,#22236,.T.);
#28481=ORIENTED_EDGE('',*,*,#21795,.T.);
#28482=ORIENTED_EDGE('',*,*,#22237,.T.);
#28483=ORIENTED_EDGE('',*,*,#22173,.F.);
#28484=ORIENTED_EDGE('',*,*,#22238,.T.);
#28485=ORIENTED_EDGE('',*,*,#22204,.F.);
#28486=ORIENTED_EDGE('',*,*,#22239,.T.);
#28487=ORIENTED_EDGE('',*,*,#21816,.F.);
#28488=ORIENTED_EDGE('',*,*,#21121,.T.);
#28489=ORIENTED_EDGE('',*,*,#21790,.T.);
#28490=ORIENTED_EDGE('',*,*,#22240,.T.);
#28491=ORIENTED_EDGE('',*,*,#22168,.F.);
#28492=ORIENTED_EDGE('',*,*,#22241,.T.);
#28493=ORIENTED_EDGE('',*,*,#22198,.F.);
#28494=ORIENTED_EDGE('',*,*,#21115,.T.);
#28495=ORIENTED_EDGE('',*,*,#21813,.F.);
#28496=ORIENTED_EDGE('',*,*,#22242,.T.);
#28497=ORIENTED_EDGE('',*,*,#21155,.F.);
#28498=ORIENTED_EDGE('',*,*,#21744,.T.);
#28499=ORIENTED_EDGE('',*,*,#21113,.T.);
#28500=ORIENTED_EDGE('',*,*,#22163,.F.);
#28501=ORIENTED_EDGE('',*,*,#21151,.F.);
#28502=ORIENTED_EDGE('',*,*,#21838,.F.);
#28503=ORIENTED_EDGE('',*,*,#22243,.T.);
#28504=ORIENTED_EDGE('',*,*,#22194,.F.);
#28505=ORIENTED_EDGE('',*,*,#21810,.T.);
#28506=ORIENTED_EDGE('',*,*,#21101,.T.);
#28507=ORIENTED_EDGE('',*,*,#22188,.F.);
#28508=ORIENTED_EDGE('',*,*,#22244,.T.);
#28509=ORIENTED_EDGE('',*,*,#22215,.F.);
#28510=ORIENTED_EDGE('',*,*,#22245,.T.);
#28511=ORIENTED_EDGE('',*,*,#21832,.F.);
#28512=ORIENTED_EDGE('',*,*,#22246,.T.);
#28513=ORIENTED_EDGE('',*,*,#21806,.T.);
#28514=ORIENTED_EDGE('',*,*,#22247,.T.);
#28515=ORIENTED_EDGE('',*,*,#22183,.F.);
#28516=ORIENTED_EDGE('',*,*,#21103,.T.);
#28517=ORIENTED_EDGE('',*,*,#22212,.F.);
#28518=ORIENTED_EDGE('',*,*,#22248,.T.);
#28519=ORIENTED_EDGE('',*,*,#21827,.F.);
#28520=ORIENTED_EDGE('',*,*,#22249,.T.);
#28521=ORIENTED_EDGE('',*,*,#22208,.F.);
#28522=ORIENTED_EDGE('',*,*,#22250,.T.);
#28523=ORIENTED_EDGE('',*,*,#21822,.F.);
#28524=ORIENTED_EDGE('',*,*,#22251,.T.);
#28525=ORIENTED_EDGE('',*,*,#21801,.T.);
#28526=ORIENTED_EDGE('',*,*,#22252,.T.);
#28527=ORIENTED_EDGE('',*,*,#22178,.F.);
#28528=ORIENTED_EDGE('',*,*,#21107,.T.);
#28529=ORIENTED_EDGE('',*,*,#21764,.T.);
#28530=ORIENTED_EDGE('',*,*,#22253,.T.);
#28531=ORIENTED_EDGE('',*,*,#22135,.F.);
#28532=ORIENTED_EDGE('',*,*,#22254,.T.);
#28533=ORIENTED_EDGE('',*,*,#22176,.F.);
#28534=ORIENTED_EDGE('',*,*,#22255,.T.);
#28535=ORIENTED_EDGE('',*,*,#21792,.F.);
#28536=ORIENTED_EDGE('',*,*,#21097,.T.);
#28537=ORIENTED_EDGE('',*,*,#21757,.T.);
#28538=ORIENTED_EDGE('',*,*,#22256,.T.);
#28539=ORIENTED_EDGE('',*,*,#22128,.F.);
#28540=ORIENTED_EDGE('',*,*,#22257,.T.);
#28541=ORIENTED_EDGE('',*,*,#22170,.F.);
#28542=ORIENTED_EDGE('',*,*,#21091,.T.);
#28543=ORIENTED_EDGE('',*,*,#21788,.F.);
#28544=ORIENTED_EDGE('',*,*,#22258,.T.);
#28545=ORIENTED_EDGE('',*,*,#21147,.F.);
#28546=ORIENTED_EDGE('',*,*,#21751,.T.);
#28547=ORIENTED_EDGE('',*,*,#21089,.T.);
#28548=ORIENTED_EDGE('',*,*,#22122,.F.);
#28549=ORIENTED_EDGE('',*,*,#21143,.F.);
#28550=ORIENTED_EDGE('',*,*,#21742,.F.);
#28551=ORIENTED_EDGE('',*,*,#22259,.T.);
#28552=ORIENTED_EDGE('',*,*,#22165,.F.);
#28553=ORIENTED_EDGE('',*,*,#21785,.T.);
#28554=ORIENTED_EDGE('',*,*,#21077,.T.);
#28555=ORIENTED_EDGE('',*,*,#22156,.F.);
#28556=ORIENTED_EDGE('',*,*,#22260,.T.);
#28557=ORIENTED_EDGE('',*,*,#22190,.F.);
#28558=ORIENTED_EDGE('',*,*,#22261,.T.);
#28559=ORIENTED_EDGE('',*,*,#21808,.F.);
#28560=ORIENTED_EDGE('',*,*,#22262,.T.);
#28561=ORIENTED_EDGE('',*,*,#21779,.T.);
#28562=ORIENTED_EDGE('',*,*,#22263,.T.);
#28563=ORIENTED_EDGE('',*,*,#22149,.F.);
#28564=ORIENTED_EDGE('',*,*,#21079,.T.);
#28565=ORIENTED_EDGE('',*,*,#22186,.F.);
#28566=ORIENTED_EDGE('',*,*,#22264,.T.);
#28567=ORIENTED_EDGE('',*,*,#21803,.F.);
#28568=ORIENTED_EDGE('',*,*,#22265,.T.);
#28569=ORIENTED_EDGE('',*,*,#22181,.F.);
#28570=ORIENTED_EDGE('',*,*,#22266,.T.);
#28571=ORIENTED_EDGE('',*,*,#21798,.F.);
#28572=ORIENTED_EDGE('',*,*,#22267,.T.);
#28573=ORIENTED_EDGE('',*,*,#21772,.T.);
#28574=ORIENTED_EDGE('',*,*,#22268,.T.);
#28575=ORIENTED_EDGE('',*,*,#22142,.F.);
#28576=ORIENTED_EDGE('',*,*,#21083,.T.);
#28577=ORIENTED_EDGE('',*,*,#22139,.F.);
#28578=ORIENTED_EDGE('',*,*,#22269,.T.);
#28579=ORIENTED_EDGE('',*,*,#21760,.F.);
#28580=ORIENTED_EDGE('',*,*,#21073,.T.);
#28581=ORIENTED_EDGE('',*,*,#22131,.F.);
#28582=ORIENTED_EDGE('',*,*,#21067,.T.);
#28583=ORIENTED_EDGE('',*,*,#21754,.F.);
#28584=ORIENTED_EDGE('',*,*,#22270,.T.);
#28585=ORIENTED_EDGE('',*,*,#21139,.F.);
#28586=ORIENTED_EDGE('',*,*,#21748,.F.);
#28587=ORIENTED_EDGE('',*,*,#22271,.T.);
#28588=ORIENTED_EDGE('',*,*,#22124,.F.);
#28589=ORIENTED_EDGE('',*,*,#22159,.F.);
#28590=ORIENTED_EDGE('',*,*,#22272,.T.);
#28591=ORIENTED_EDGE('',*,*,#21782,.F.);
#28592=ORIENTED_EDGE('',*,*,#22273,.T.);
#28593=ORIENTED_EDGE('',*,*,#22153,.F.);
#28594=ORIENTED_EDGE('',*,*,#22274,.T.);
#28595=ORIENTED_EDGE('',*,*,#21775,.F.);
#28596=ORIENTED_EDGE('',*,*,#22275,.T.);
#28597=ORIENTED_EDGE('',*,*,#22146,.F.);
#28598=ORIENTED_EDGE('',*,*,#22276,.T.);
#28599=ORIENTED_EDGE('',*,*,#21768,.F.);
#28600=ORIENTED_EDGE('',*,*,#22277,.T.);
#28601=ORIENTED_EDGE('',*,*,#22138,.F.);
#28602=ORIENTED_EDGE('',*,*,#22235,.F.);
#28603=ORIENTED_EDGE('',*,*,#21761,.F.);
#28604=ORIENTED_EDGE('',*,*,#22269,.F.);
#28605=ORIENTED_EDGE('',*,*,#22175,.F.);
#28606=ORIENTED_EDGE('',*,*,#21691,.F.);
#28607=ORIENTED_EDGE('',*,*,#21793,.F.);
#28608=ORIENTED_EDGE('',*,*,#22255,.F.);
#28609=ORIENTED_EDGE('',*,*,#21763,.F.);
#28610=ORIENTED_EDGE('',*,*,#22236,.F.);
#28611=ORIENTED_EDGE('',*,*,#22136,.F.);
#28612=ORIENTED_EDGE('',*,*,#22253,.F.);
#28613=ORIENTED_EDGE('',*,*,#22203,.F.);
#28614=ORIENTED_EDGE('',*,*,#21733,.F.);
#28615=ORIENTED_EDGE('',*,*,#21817,.F.);
#28616=ORIENTED_EDGE('',*,*,#22239,.F.);
#28617=ORIENTED_EDGE('',*,*,#21794,.F.);
#28618=ORIENTED_EDGE('',*,*,#21693,.F.);
#28619=ORIENTED_EDGE('',*,*,#22174,.F.);
#28620=ORIENTED_EDGE('',*,*,#22237,.F.);
#28621=ORIENTED_EDGE('',*,*,#21820,.F.);
#28622=ORIENTED_EDGE('',*,*,#22218,.F.);
#28623=ORIENTED_EDGE('',*,*,#22205,.F.);
#28624=ORIENTED_EDGE('',*,*,#21698,.F.);
#28625=ORIENTED_EDGE('',*,*,#21824,.F.);
#28626=ORIENTED_EDGE('',*,*,#21701,.F.);
#28627=ORIENTED_EDGE('',*,*,#22206,.F.);
#28628=ORIENTED_EDGE('',*,*,#21848,.F.);
#28629=ORIENTED_EDGE('',*,*,#21829,.F.);
#28630=ORIENTED_EDGE('',*,*,#21708,.F.);
#28631=ORIENTED_EDGE('',*,*,#22210,.F.);
#28632=ORIENTED_EDGE('',*,*,#21846,.F.);
#28633=ORIENTED_EDGE('',*,*,#21835,.F.);
#28634=ORIENTED_EDGE('',*,*,#21845,.F.);
#28635=ORIENTED_EDGE('',*,*,#22217,.F.);
#28636=ORIENTED_EDGE('',*,*,#21718,.F.);
#28637=ORIENTED_EDGE('',*,*,#21836,.F.);
#28638=ORIENTED_EDGE('',*,*,#21195,.F.);
#28639=ORIENTED_EDGE('',*,*,#22196,.F.);
#28640=ORIENTED_EDGE('',*,*,#21722,.F.);
#28641=ORIENTED_EDGE('',*,*,#21814,.F.);
#28642=ORIENTED_EDGE('',*,*,#21726,.F.);
#28643=ORIENTED_EDGE('',*,*,#22197,.F.);
#28644=ORIENTED_EDGE('',*,*,#21737,.F.);
#28645=ORIENTED_EDGE('',*,*,#21815,.F.);
#28646=ORIENTED_EDGE('',*,*,#21739,.F.);
#28647=ORIENTED_EDGE('',*,*,#22200,.F.);
#28648=ORIENTED_EDGE('',*,*,#21729,.F.);
#28649=ORIENTED_EDGE('',*,*,#21818,.F.);
#28650=ORIENTED_EDGE('',*,*,#21735,.F.);
#28651=ORIENTED_EDGE('',*,*,#22202,.F.);
#28652=ORIENTED_EDGE('',*,*,#22219,.F.);
#28653=ORIENTED_EDGE('',*,*,#22193,.F.);
#28654=ORIENTED_EDGE('',*,*,#21696,.F.);
#28655=ORIENTED_EDGE('',*,*,#21839,.F.);
#28656=ORIENTED_EDGE('',*,*,#21153,.F.);
#28657=ORIENTED_EDGE('',*,*,#22207,.F.);
#28658=ORIENTED_EDGE('',*,*,#21703,.F.);
#28659=ORIENTED_EDGE('',*,*,#21823,.F.);
#28660=ORIENTED_EDGE('',*,*,#22250,.F.);
#28661=ORIENTED_EDGE('',*,*,#21821,.F.);
#28662=ORIENTED_EDGE('',*,*,#21706,.F.);
#28663=ORIENTED_EDGE('',*,*,#22209,.F.);
#28664=ORIENTED_EDGE('',*,*,#22251,.F.);
#28665=ORIENTED_EDGE('',*,*,#22211,.F.);
#28666=ORIENTED_EDGE('',*,*,#21710,.F.);
#28667=ORIENTED_EDGE('',*,*,#21828,.F.);
#28668=ORIENTED_EDGE('',*,*,#22248,.F.);
#28669=ORIENTED_EDGE('',*,*,#21826,.F.);
#28670=ORIENTED_EDGE('',*,*,#21713,.F.);
#28671=ORIENTED_EDGE('',*,*,#22213,.F.);
#28672=ORIENTED_EDGE('',*,*,#22249,.F.);
#28673=ORIENTED_EDGE('',*,*,#22214,.F.);
#28674=ORIENTED_EDGE('',*,*,#21716,.F.);
#28675=ORIENTED_EDGE('',*,*,#21833,.F.);
#28676=ORIENTED_EDGE('',*,*,#22245,.F.);
#28677=ORIENTED_EDGE('',*,*,#21831,.F.);
#28678=ORIENTED_EDGE('',*,*,#21720,.F.);
#28679=ORIENTED_EDGE('',*,*,#22216,.F.);
#28680=ORIENTED_EDGE('',*,*,#22246,.F.);
#28681=ORIENTED_EDGE('',*,*,#21837,.F.);
#28682=ORIENTED_EDGE('',*,*,#21724,.F.);
#28683=ORIENTED_EDGE('',*,*,#22195,.F.);
#28684=ORIENTED_EDGE('',*,*,#22243,.F.);
#28685=ORIENTED_EDGE('',*,*,#21812,.F.);
#28686=ORIENTED_EDGE('',*,*,#21731,.F.);
#28687=ORIENTED_EDGE('',*,*,#22199,.F.);
#28688=ORIENTED_EDGE('',*,*,#22242,.F.);
#28689=ORIENTED_EDGE('',*,*,#22177,.F.);
#28690=ORIENTED_EDGE('',*,*,#21656,.F.);
#28691=ORIENTED_EDGE('',*,*,#21796,.F.);
#28692=ORIENTED_EDGE('',*,*,#22238,.F.);
#28693=ORIENTED_EDGE('',*,*,#21800,.F.);
#28694=ORIENTED_EDGE('',*,*,#21659,.F.);
#28695=ORIENTED_EDGE('',*,*,#22179,.F.);
#28696=ORIENTED_EDGE('',*,*,#22252,.F.);
#28697=ORIENTED_EDGE('',*,*,#21805,.F.);
#28698=ORIENTED_EDGE('',*,*,#21666,.F.);
#28699=ORIENTED_EDGE('',*,*,#22184,.F.);
#28700=ORIENTED_EDGE('',*,*,#22247,.F.);
#28701=ORIENTED_EDGE('',*,*,#22192,.F.);
#28702=ORIENTED_EDGE('',*,*,#21676,.F.);
#28703=ORIENTED_EDGE('',*,*,#21811,.F.);
#28704=ORIENTED_EDGE('',*,*,#22244,.F.);
#28705=ORIENTED_EDGE('',*,*,#22167,.F.);
#28706=ORIENTED_EDGE('',*,*,#21680,.F.);
#28707=ORIENTED_EDGE('',*,*,#21740,.F.);
#28708=ORIENTED_EDGE('',*,*,#21157,.F.);
#28709=ORIENTED_EDGE('',*,*,#21789,.F.);
#28710=ORIENTED_EDGE('',*,*,#21684,.F.);
#28711=ORIENTED_EDGE('',*,*,#22169,.F.);
#28712=ORIENTED_EDGE('',*,*,#22240,.F.);
#28713=ORIENTED_EDGE('',*,*,#22172,.F.);
#28714=ORIENTED_EDGE('',*,*,#21687,.F.);
#28715=ORIENTED_EDGE('',*,*,#21791,.F.);
#28716=ORIENTED_EDGE('',*,*,#22241,.F.);
#28717=ORIENTED_EDGE('',*,*,#22164,.F.);
#28718=ORIENTED_EDGE('',*,*,#21654,.F.);
#28719=ORIENTED_EDGE('',*,*,#21743,.F.);
#28720=ORIENTED_EDGE('',*,*,#21145,.F.);
#28721=ORIENTED_EDGE('',*,*,#22180,.F.);
#28722=ORIENTED_EDGE('',*,*,#21661,.F.);
#28723=ORIENTED_EDGE('',*,*,#21799,.F.);
#28724=ORIENTED_EDGE('',*,*,#22266,.F.);
#28725=ORIENTED_EDGE('',*,*,#21797,.F.);
#28726=ORIENTED_EDGE('',*,*,#21664,.F.);
#28727=ORIENTED_EDGE('',*,*,#22182,.F.);
#28728=ORIENTED_EDGE('',*,*,#22267,.F.);
#28729=ORIENTED_EDGE('',*,*,#22185,.F.);
#28730=ORIENTED_EDGE('',*,*,#21668,.F.);
#28731=ORIENTED_EDGE('',*,*,#21804,.F.);
#28732=ORIENTED_EDGE('',*,*,#22264,.F.);
#28733=ORIENTED_EDGE('',*,*,#21802,.F.);
#28734=ORIENTED_EDGE('',*,*,#21671,.F.);
#28735=ORIENTED_EDGE('',*,*,#22187,.F.);
#28736=ORIENTED_EDGE('',*,*,#22265,.F.);
#28737=ORIENTED_EDGE('',*,*,#22189,.F.);
#28738=ORIENTED_EDGE('',*,*,#21674,.F.);
#28739=ORIENTED_EDGE('',*,*,#21809,.F.);
#28740=ORIENTED_EDGE('',*,*,#22261,.F.);
#28741=ORIENTED_EDGE('',*,*,#21807,.F.);
#28742=ORIENTED_EDGE('',*,*,#21678,.F.);
#28743=ORIENTED_EDGE('',*,*,#22191,.F.);
#28744=ORIENTED_EDGE('',*,*,#22262,.F.);
#28745=ORIENTED_EDGE('',*,*,#21741,.F.);
#28746=ORIENTED_EDGE('',*,*,#21682,.F.);
#28747=ORIENTED_EDGE('',*,*,#22166,.F.);
#28748=ORIENTED_EDGE('',*,*,#22259,.F.);
#28749=ORIENTED_EDGE('',*,*,#21787,.F.);
#28750=ORIENTED_EDGE('',*,*,#21689,.F.);
#28751=ORIENTED_EDGE('',*,*,#22171,.F.);
#28752=ORIENTED_EDGE('',*,*,#22258,.F.);
#28753=ORIENTED_EDGE('',*,*,#22141,.F.);
#28754=ORIENTED_EDGE('',*,*,#22220,.F.);
#28755=ORIENTED_EDGE('',*,*,#21765,.F.);
#28756=ORIENTED_EDGE('',*,*,#22254,.F.);
#28757=ORIENTED_EDGE('',*,*,#21771,.F.);
#28758=ORIENTED_EDGE('',*,*,#22221,.F.);
#28759=ORIENTED_EDGE('',*,*,#22143,.F.);
#28760=ORIENTED_EDGE('',*,*,#22268,.F.);
#28761=ORIENTED_EDGE('',*,*,#21778,.F.);
#28762=ORIENTED_EDGE('',*,*,#22224,.F.);
#28763=ORIENTED_EDGE('',*,*,#22150,.F.);
#28764=ORIENTED_EDGE('',*,*,#22263,.F.);
#28765=ORIENTED_EDGE('',*,*,#22162,.F.);
#28766=ORIENTED_EDGE('',*,*,#22228,.F.);
#28767=ORIENTED_EDGE('',*,*,#21786,.F.);
#28768=ORIENTED_EDGE('',*,*,#22260,.F.);
#28769=ORIENTED_EDGE('',*,*,#22127,.F.);
#28770=ORIENTED_EDGE('',*,*,#22230,.F.);
#28771=ORIENTED_EDGE('',*,*,#21745,.F.);
#28772=ORIENTED_EDGE('',*,*,#21149,.F.);
#28773=ORIENTED_EDGE('',*,*,#21756,.F.);
#28774=ORIENTED_EDGE('',*,*,#22232,.F.);
#28775=ORIENTED_EDGE('',*,*,#22129,.F.);
#28776=ORIENTED_EDGE('',*,*,#22256,.F.);
#28777=ORIENTED_EDGE('',*,*,#22134,.F.);
#28778=ORIENTED_EDGE('',*,*,#22233,.F.);
#28779=ORIENTED_EDGE('',*,*,#21758,.F.);
#28780=ORIENTED_EDGE('',*,*,#22257,.F.);
#28781=ORIENTED_EDGE('',*,*,#22123,.F.);
#28782=ORIENTED_EDGE('',*,*,#21843,.F.);
#28783=ORIENTED_EDGE('',*,*,#21749,.F.);
#28784=ORIENTED_EDGE('',*,*,#21141,.F.);
#28785=ORIENTED_EDGE('',*,*,#22145,.F.);
#28786=ORIENTED_EDGE('',*,*,#22222,.F.);
#28787=ORIENTED_EDGE('',*,*,#21769,.F.);
#28788=ORIENTED_EDGE('',*,*,#22276,.F.);
#28789=ORIENTED_EDGE('',*,*,#21767,.F.);
#28790=ORIENTED_EDGE('',*,*,#22223,.F.);
#28791=ORIENTED_EDGE('',*,*,#22147,.F.);
#28792=ORIENTED_EDGE('',*,*,#22277,.F.);
#28793=ORIENTED_EDGE('',*,*,#22152,.F.);
#28794=ORIENTED_EDGE('',*,*,#22225,.F.);
#28795=ORIENTED_EDGE('',*,*,#21776,.F.);
#28796=ORIENTED_EDGE('',*,*,#22274,.F.);
#28797=ORIENTED_EDGE('',*,*,#21774,.F.);
#28798=ORIENTED_EDGE('',*,*,#22226,.F.);
#28799=ORIENTED_EDGE('',*,*,#22154,.F.);
#28800=ORIENTED_EDGE('',*,*,#22275,.F.);
#28801=ORIENTED_EDGE('',*,*,#22158,.F.);
#28802=ORIENTED_EDGE('',*,*,#22227,.F.);
#28803=ORIENTED_EDGE('',*,*,#21783,.F.);
#28804=ORIENTED_EDGE('',*,*,#22272,.F.);
#28805=ORIENTED_EDGE('',*,*,#21781,.F.);
#28806=ORIENTED_EDGE('',*,*,#22229,.F.);
#28807=ORIENTED_EDGE('',*,*,#22160,.F.);
#28808=ORIENTED_EDGE('',*,*,#22273,.F.);
#28809=ORIENTED_EDGE('',*,*,#21747,.F.);
#28810=ORIENTED_EDGE('',*,*,#22231,.F.);
#28811=ORIENTED_EDGE('',*,*,#22125,.F.);
#28812=ORIENTED_EDGE('',*,*,#22271,.F.);
#28813=ORIENTED_EDGE('',*,*,#21753,.F.);
#28814=ORIENTED_EDGE('',*,*,#22234,.F.);
#28815=ORIENTED_EDGE('',*,*,#22132,.F.);
#28816=ORIENTED_EDGE('',*,*,#22270,.F.);
#28817=ORIENTED_EDGE('',*,*,#22278,.T.);
#28818=ORIENTED_EDGE('',*,*,#21864,.T.);
#28819=ORIENTED_EDGE('',*,*,#22279,.F.);
#28820=ORIENTED_EDGE('',*,*,#21891,.F.);
#28821=ORIENTED_EDGE('',*,*,#22280,.T.);
#28822=ORIENTED_EDGE('',*,*,#21865,.T.);
#28823=ORIENTED_EDGE('',*,*,#22278,.F.);
#28824=ORIENTED_EDGE('',*,*,#21890,.F.);
#28825=ORIENTED_EDGE('',*,*,#22281,.T.);
#28826=ORIENTED_EDGE('',*,*,#21866,.T.);
#28827=ORIENTED_EDGE('',*,*,#22280,.F.);
#28828=ORIENTED_EDGE('',*,*,#21901,.F.);
#28829=ORIENTED_EDGE('',*,*,#22282,.T.);
#28830=ORIENTED_EDGE('',*,*,#21867,.T.);
#28831=ORIENTED_EDGE('',*,*,#22281,.F.);
#28832=ORIENTED_EDGE('',*,*,#21900,.F.);
#28833=ORIENTED_EDGE('',*,*,#22283,.T.);
#28834=ORIENTED_EDGE('',*,*,#21868,.T.);
#28835=ORIENTED_EDGE('',*,*,#22282,.F.);
#28836=ORIENTED_EDGE('',*,*,#21899,.F.);
#28837=ORIENTED_EDGE('',*,*,#22284,.T.);
#28838=ORIENTED_EDGE('',*,*,#21869,.T.);
#28839=ORIENTED_EDGE('',*,*,#22283,.F.);
#28840=ORIENTED_EDGE('',*,*,#21898,.F.);
#28841=ORIENTED_EDGE('',*,*,#22285,.T.);
#28842=ORIENTED_EDGE('',*,*,#21870,.T.);
#28843=ORIENTED_EDGE('',*,*,#22284,.F.);
#28844=ORIENTED_EDGE('',*,*,#21897,.F.);
#28845=ORIENTED_EDGE('',*,*,#22286,.T.);
#28846=ORIENTED_EDGE('',*,*,#21871,.T.);
#28847=ORIENTED_EDGE('',*,*,#22285,.F.);
#28848=ORIENTED_EDGE('',*,*,#21896,.F.);
#28849=ORIENTED_EDGE('',*,*,#22287,.T.);
#28850=ORIENTED_EDGE('',*,*,#21872,.T.);
#28851=ORIENTED_EDGE('',*,*,#22286,.F.);
#28852=ORIENTED_EDGE('',*,*,#21895,.F.);
#28853=ORIENTED_EDGE('',*,*,#22288,.T.);
#28854=ORIENTED_EDGE('',*,*,#21873,.T.);
#28855=ORIENTED_EDGE('',*,*,#22287,.F.);
#28856=ORIENTED_EDGE('',*,*,#21894,.F.);
#28857=ORIENTED_EDGE('',*,*,#22289,.T.);
#28858=ORIENTED_EDGE('',*,*,#21874,.T.);
#28859=ORIENTED_EDGE('',*,*,#22288,.F.);
#28860=ORIENTED_EDGE('',*,*,#21893,.F.);
#28861=ORIENTED_EDGE('',*,*,#22279,.T.);
#28862=ORIENTED_EDGE('',*,*,#21875,.T.);
#28863=ORIENTED_EDGE('',*,*,#22289,.F.);
#28864=ORIENTED_EDGE('',*,*,#21892,.F.);
#28865=ORIENTED_EDGE('',*,*,#22290,.T.);
#28866=ORIENTED_EDGE('',*,*,#21860,.T.);
#28867=ORIENTED_EDGE('',*,*,#22291,.F.);
#28868=ORIENTED_EDGE('',*,*,#21887,.F.);
#28869=ORIENTED_EDGE('',*,*,#22292,.T.);
#28870=ORIENTED_EDGE('',*,*,#21861,.T.);
#28871=ORIENTED_EDGE('',*,*,#22290,.F.);
#28872=ORIENTED_EDGE('',*,*,#21886,.F.);
#28873=ORIENTED_EDGE('',*,*,#22293,.T.);
#28874=ORIENTED_EDGE('',*,*,#21862,.T.);
#28875=ORIENTED_EDGE('',*,*,#22292,.F.);
#28876=ORIENTED_EDGE('',*,*,#21889,.F.);
#28877=ORIENTED_EDGE('',*,*,#22291,.T.);
#28878=ORIENTED_EDGE('',*,*,#21863,.T.);
#28879=ORIENTED_EDGE('',*,*,#22293,.F.);
#28880=ORIENTED_EDGE('',*,*,#21888,.F.);
#28881=ORIENTED_EDGE('',*,*,#21859,.F.);
#28882=ORIENTED_EDGE('',*,*,#21927,.F.);
#28883=ORIENTED_EDGE('',*,*,#21879,.F.);
#28884=ORIENTED_EDGE('',*,*,#21926,.F.);
#28885=ORIENTED_EDGE('',*,*,#21507,.F.);
#28886=ORIENTED_EDGE('',*,*,#21940,.F.);
#28887=ORIENTED_EDGE('',*,*,#21347,.F.);
#28888=ORIENTED_EDGE('',*,*,#21942,.F.);
#28889=ORIENTED_EDGE('',*,*,#21499,.F.);
#28890=ORIENTED_EDGE('',*,*,#21941,.F.);
#28891=ORIENTED_EDGE('',*,*,#21345,.F.);
#28892=ORIENTED_EDGE('',*,*,#21943,.F.);
#28893=ORIENTED_EDGE('',*,*,#21851,.F.);
#28894=ORIENTED_EDGE('',*,*,#21925,.F.);
#28895=ORIENTED_EDGE('',*,*,#21877,.F.);
#28896=ORIENTED_EDGE('',*,*,#21924,.F.);
#28897=ORIENTED_EDGE('',*,*,#22294,.T.);
#28898=ORIENTED_EDGE('',*,*,#21355,.T.);
#28899=ORIENTED_EDGE('',*,*,#21063,.F.);
#28900=ORIENTED_EDGE('',*,*,#21651,.F.);
#28901=ORIENTED_EDGE('',*,*,#21650,.T.);
#28902=ORIENTED_EDGE('',*,*,#22295,.T.);
#28903=ORIENTED_EDGE('',*,*,#21356,.F.);
#28904=ORIENTED_EDGE('',*,*,#22294,.F.);
#28905=ORIENTED_EDGE('',*,*,#21649,.T.);
#28906=ORIENTED_EDGE('',*,*,#21065,.T.);
#28907=ORIENTED_EDGE('',*,*,#21354,.F.);
#28908=ORIENTED_EDGE('',*,*,#22295,.F.);
#28909=ORIENTED_EDGE('',*,*,#21061,.T.);
#28910=ORIENTED_EDGE('',*,*,#21495,.T.);
#28911=ORIENTED_EDGE('',*,*,#22296,.F.);
#28912=ORIENTED_EDGE('',*,*,#21508,.F.);
#28913=ORIENTED_EDGE('',*,*,#21510,.T.);
#28914=ORIENTED_EDGE('',*,*,#22297,.T.);
#28915=ORIENTED_EDGE('',*,*,#21496,.F.);
#28916=ORIENTED_EDGE('',*,*,#21059,.F.);
#28917=ORIENTED_EDGE('',*,*,#22296,.T.);
#28918=ORIENTED_EDGE('',*,*,#21497,.T.);
#28919=ORIENTED_EDGE('',*,*,#22297,.F.);
#28920=ORIENTED_EDGE('',*,*,#21509,.F.);
#28921=ORIENTED_EDGE('',*,*,#21057,.T.);
#28922=ORIENTED_EDGE('',*,*,#21492,.T.);
#28923=ORIENTED_EDGE('',*,*,#22298,.F.);
#28924=ORIENTED_EDGE('',*,*,#21511,.F.);
#28925=ORIENTED_EDGE('',*,*,#21513,.T.);
#28926=ORIENTED_EDGE('',*,*,#22299,.T.);
#28927=ORIENTED_EDGE('',*,*,#21493,.F.);
#28928=ORIENTED_EDGE('',*,*,#21055,.F.);
#28929=ORIENTED_EDGE('',*,*,#22298,.T.);
#28930=ORIENTED_EDGE('',*,*,#21494,.T.);
#28931=ORIENTED_EDGE('',*,*,#22299,.F.);
#28932=ORIENTED_EDGE('',*,*,#21512,.F.);
#28933=ORIENTED_EDGE('',*,*,#22300,.T.);
#28934=ORIENTED_EDGE('',*,*,#21358,.T.);
#28935=ORIENTED_EDGE('',*,*,#21051,.F.);
#28936=ORIENTED_EDGE('',*,*,#21516,.F.);
#28937=ORIENTED_EDGE('',*,*,#21515,.T.);
#28938=ORIENTED_EDGE('',*,*,#22301,.T.);
#28939=ORIENTED_EDGE('',*,*,#21359,.F.);
#28940=ORIENTED_EDGE('',*,*,#22300,.F.);
#28941=ORIENTED_EDGE('',*,*,#21514,.T.);
#28942=ORIENTED_EDGE('',*,*,#21053,.T.);
#28943=ORIENTED_EDGE('',*,*,#21357,.F.);
#28944=ORIENTED_EDGE('',*,*,#22301,.F.);
#28945=ORIENTED_EDGE('',*,*,#21049,.T.);
#28946=ORIENTED_EDGE('',*,*,#21489,.T.);
#28947=ORIENTED_EDGE('',*,*,#22302,.F.);
#28948=ORIENTED_EDGE('',*,*,#21646,.F.);
#28949=ORIENTED_EDGE('',*,*,#21648,.T.);
#28950=ORIENTED_EDGE('',*,*,#22303,.T.);
#28951=ORIENTED_EDGE('',*,*,#21490,.F.);
#28952=ORIENTED_EDGE('',*,*,#21047,.F.);
#28953=ORIENTED_EDGE('',*,*,#22302,.T.);
#28954=ORIENTED_EDGE('',*,*,#21491,.T.);
#28955=ORIENTED_EDGE('',*,*,#22303,.F.);
#28956=ORIENTED_EDGE('',*,*,#21647,.F.);
#28957=ORIENTED_EDGE('',*,*,#22304,.T.);
#28958=ORIENTED_EDGE('',*,*,#21361,.T.);
#28959=ORIENTED_EDGE('',*,*,#21043,.F.);
#28960=ORIENTED_EDGE('',*,*,#21645,.F.);
#28961=ORIENTED_EDGE('',*,*,#21644,.T.);
#28962=ORIENTED_EDGE('',*,*,#22305,.T.);
#28963=ORIENTED_EDGE('',*,*,#21362,.F.);
#28964=ORIENTED_EDGE('',*,*,#22304,.F.);
#28965=ORIENTED_EDGE('',*,*,#21643,.T.);
#28966=ORIENTED_EDGE('',*,*,#21045,.T.);
#28967=ORIENTED_EDGE('',*,*,#21360,.F.);
#28968=ORIENTED_EDGE('',*,*,#22305,.F.);
#28969=ORIENTED_EDGE('',*,*,#22306,.T.);
#28970=ORIENTED_EDGE('',*,*,#21364,.T.);
#28971=ORIENTED_EDGE('',*,*,#21039,.F.);
#28972=ORIENTED_EDGE('',*,*,#21519,.F.);
#28973=ORIENTED_EDGE('',*,*,#21518,.T.);
#28974=ORIENTED_EDGE('',*,*,#22307,.T.);
#28975=ORIENTED_EDGE('',*,*,#21365,.F.);
#28976=ORIENTED_EDGE('',*,*,#22306,.F.);
#28977=ORIENTED_EDGE('',*,*,#21517,.T.);
#28978=ORIENTED_EDGE('',*,*,#21041,.T.);
#28979=ORIENTED_EDGE('',*,*,#21363,.F.);
#28980=ORIENTED_EDGE('',*,*,#22307,.F.);
#28981=ORIENTED_EDGE('',*,*,#21037,.T.);
#28982=ORIENTED_EDGE('',*,*,#21486,.T.);
#28983=ORIENTED_EDGE('',*,*,#22308,.F.);
#28984=ORIENTED_EDGE('',*,*,#21640,.F.);
#28985=ORIENTED_EDGE('',*,*,#21642,.T.);
#28986=ORIENTED_EDGE('',*,*,#22309,.T.);
#28987=ORIENTED_EDGE('',*,*,#21487,.F.);
#28988=ORIENTED_EDGE('',*,*,#21035,.F.);
#28989=ORIENTED_EDGE('',*,*,#22308,.T.);
#28990=ORIENTED_EDGE('',*,*,#21488,.T.);
#28991=ORIENTED_EDGE('',*,*,#22309,.F.);
#28992=ORIENTED_EDGE('',*,*,#21641,.F.);
#28993=ORIENTED_EDGE('',*,*,#21033,.T.);
#28994=ORIENTED_EDGE('',*,*,#21483,.T.);
#28995=ORIENTED_EDGE('',*,*,#22310,.F.);
#28996=ORIENTED_EDGE('',*,*,#21637,.F.);
#28997=ORIENTED_EDGE('',*,*,#21639,.T.);
#28998=ORIENTED_EDGE('',*,*,#22311,.T.);
#28999=ORIENTED_EDGE('',*,*,#21484,.F.);
#29000=ORIENTED_EDGE('',*,*,#21031,.F.);
#29001=ORIENTED_EDGE('',*,*,#22310,.T.);
#29002=ORIENTED_EDGE('',*,*,#21485,.T.);
#29003=ORIENTED_EDGE('',*,*,#22311,.F.);
#29004=ORIENTED_EDGE('',*,*,#21638,.F.);
#29005=ORIENTED_EDGE('',*,*,#21029,.T.);
#29006=ORIENTED_EDGE('',*,*,#21480,.T.);
#29007=ORIENTED_EDGE('',*,*,#22312,.F.);
#29008=ORIENTED_EDGE('',*,*,#21634,.F.);
#29009=ORIENTED_EDGE('',*,*,#21636,.T.);
#29010=ORIENTED_EDGE('',*,*,#22313,.T.);
#29011=ORIENTED_EDGE('',*,*,#21481,.F.);
#29012=ORIENTED_EDGE('',*,*,#21027,.F.);
#29013=ORIENTED_EDGE('',*,*,#22312,.T.);
#29014=ORIENTED_EDGE('',*,*,#21482,.T.);
#29015=ORIENTED_EDGE('',*,*,#22313,.F.);
#29016=ORIENTED_EDGE('',*,*,#21635,.F.);
#29017=ORIENTED_EDGE('',*,*,#21025,.T.);
#29018=ORIENTED_EDGE('',*,*,#21477,.T.);
#29019=ORIENTED_EDGE('',*,*,#22314,.F.);
#29020=ORIENTED_EDGE('',*,*,#21631,.F.);
#29021=ORIENTED_EDGE('',*,*,#21633,.T.);
#29022=ORIENTED_EDGE('',*,*,#22315,.T.);
#29023=ORIENTED_EDGE('',*,*,#21478,.F.);
#29024=ORIENTED_EDGE('',*,*,#21023,.F.);
#29025=ORIENTED_EDGE('',*,*,#22314,.T.);
#29026=ORIENTED_EDGE('',*,*,#21479,.T.);
#29027=ORIENTED_EDGE('',*,*,#22315,.F.);
#29028=ORIENTED_EDGE('',*,*,#21632,.F.);
#29029=ORIENTED_EDGE('',*,*,#22316,.T.);
#29030=ORIENTED_EDGE('',*,*,#21367,.T.);
#29031=ORIENTED_EDGE('',*,*,#21019,.F.);
#29032=ORIENTED_EDGE('',*,*,#21630,.F.);
#29033=ORIENTED_EDGE('',*,*,#21629,.T.);
#29034=ORIENTED_EDGE('',*,*,#22317,.T.);
#29035=ORIENTED_EDGE('',*,*,#21368,.F.);
#29036=ORIENTED_EDGE('',*,*,#22316,.F.);
#29037=ORIENTED_EDGE('',*,*,#21628,.T.);
#29038=ORIENTED_EDGE('',*,*,#21021,.T.);
#29039=ORIENTED_EDGE('',*,*,#21366,.F.);
#29040=ORIENTED_EDGE('',*,*,#22317,.F.);
#29041=ORIENTED_EDGE('',*,*,#22318,.T.);
#29042=ORIENTED_EDGE('',*,*,#21370,.T.);
#29043=ORIENTED_EDGE('',*,*,#21015,.F.);
#29044=ORIENTED_EDGE('',*,*,#21522,.F.);
#29045=ORIENTED_EDGE('',*,*,#21521,.T.);
#29046=ORIENTED_EDGE('',*,*,#22319,.T.);
#29047=ORIENTED_EDGE('',*,*,#21371,.F.);
#29048=ORIENTED_EDGE('',*,*,#22318,.F.);
#29049=ORIENTED_EDGE('',*,*,#21520,.T.);
#29050=ORIENTED_EDGE('',*,*,#21017,.T.);
#29051=ORIENTED_EDGE('',*,*,#21369,.F.);
#29052=ORIENTED_EDGE('',*,*,#22319,.F.);
#29053=ORIENTED_EDGE('',*,*,#22320,.T.);
#29054=ORIENTED_EDGE('',*,*,#21373,.T.);
#29055=ORIENTED_EDGE('',*,*,#21011,.F.);
#29056=ORIENTED_EDGE('',*,*,#21627,.F.);
#29057=ORIENTED_EDGE('',*,*,#21626,.T.);
#29058=ORIENTED_EDGE('',*,*,#22321,.T.);
#29059=ORIENTED_EDGE('',*,*,#21374,.F.);
#29060=ORIENTED_EDGE('',*,*,#22320,.F.);
#29061=ORIENTED_EDGE('',*,*,#21625,.T.);
#29062=ORIENTED_EDGE('',*,*,#21013,.T.);
#29063=ORIENTED_EDGE('',*,*,#21372,.F.);
#29064=ORIENTED_EDGE('',*,*,#22321,.F.);
#29065=ORIENTED_EDGE('',*,*,#22322,.T.);
#29066=ORIENTED_EDGE('',*,*,#21376,.T.);
#29067=ORIENTED_EDGE('',*,*,#21007,.F.);
#29068=ORIENTED_EDGE('',*,*,#21525,.F.);
#29069=ORIENTED_EDGE('',*,*,#21524,.T.);
#29070=ORIENTED_EDGE('',*,*,#22323,.T.);
#29071=ORIENTED_EDGE('',*,*,#21377,.F.);
#29072=ORIENTED_EDGE('',*,*,#22322,.F.);
#29073=ORIENTED_EDGE('',*,*,#21523,.T.);
#29074=ORIENTED_EDGE('',*,*,#21009,.T.);
#29075=ORIENTED_EDGE('',*,*,#21375,.F.);
#29076=ORIENTED_EDGE('',*,*,#22323,.F.);
#29077=ORIENTED_EDGE('',*,*,#22324,.T.);
#29078=ORIENTED_EDGE('',*,*,#21379,.T.);
#29079=ORIENTED_EDGE('',*,*,#21003,.F.);
#29080=ORIENTED_EDGE('',*,*,#21624,.F.);
#29081=ORIENTED_EDGE('',*,*,#21623,.T.);
#29082=ORIENTED_EDGE('',*,*,#22325,.T.);
#29083=ORIENTED_EDGE('',*,*,#21380,.F.);
#29084=ORIENTED_EDGE('',*,*,#22324,.F.);
#29085=ORIENTED_EDGE('',*,*,#21622,.T.);
#29086=ORIENTED_EDGE('',*,*,#21005,.T.);
#29087=ORIENTED_EDGE('',*,*,#21378,.F.);
#29088=ORIENTED_EDGE('',*,*,#22325,.F.);
#29089=ORIENTED_EDGE('',*,*,#22326,.T.);
#29090=ORIENTED_EDGE('',*,*,#21382,.T.);
#29091=ORIENTED_EDGE('',*,*,#20999,.F.);
#29092=ORIENTED_EDGE('',*,*,#21528,.F.);
#29093=ORIENTED_EDGE('',*,*,#21527,.T.);
#29094=ORIENTED_EDGE('',*,*,#22327,.T.);
#29095=ORIENTED_EDGE('',*,*,#21383,.F.);
#29096=ORIENTED_EDGE('',*,*,#22326,.F.);
#29097=ORIENTED_EDGE('',*,*,#21526,.T.);
#29098=ORIENTED_EDGE('',*,*,#21001,.T.);
#29099=ORIENTED_EDGE('',*,*,#21381,.F.);
#29100=ORIENTED_EDGE('',*,*,#22327,.F.);
#29101=ORIENTED_EDGE('',*,*,#22328,.T.);
#29102=ORIENTED_EDGE('',*,*,#21385,.T.);
#29103=ORIENTED_EDGE('',*,*,#20995,.F.);
#29104=ORIENTED_EDGE('',*,*,#21621,.F.);
#29105=ORIENTED_EDGE('',*,*,#21620,.T.);
#29106=ORIENTED_EDGE('',*,*,#22329,.T.);
#29107=ORIENTED_EDGE('',*,*,#21386,.F.);
#29108=ORIENTED_EDGE('',*,*,#22328,.F.);
#29109=ORIENTED_EDGE('',*,*,#21619,.T.);
#29110=ORIENTED_EDGE('',*,*,#20997,.T.);
#29111=ORIENTED_EDGE('',*,*,#21384,.F.);
#29112=ORIENTED_EDGE('',*,*,#22329,.F.);
#29113=ORIENTED_EDGE('',*,*,#20993,.T.);
#29114=ORIENTED_EDGE('',*,*,#21474,.T.);
#29115=ORIENTED_EDGE('',*,*,#22330,.F.);
#29116=ORIENTED_EDGE('',*,*,#21529,.F.);
#29117=ORIENTED_EDGE('',*,*,#21531,.T.);
#29118=ORIENTED_EDGE('',*,*,#22331,.T.);
#29119=ORIENTED_EDGE('',*,*,#21475,.F.);
#29120=ORIENTED_EDGE('',*,*,#20991,.F.);
#29121=ORIENTED_EDGE('',*,*,#22330,.T.);
#29122=ORIENTED_EDGE('',*,*,#21476,.T.);
#29123=ORIENTED_EDGE('',*,*,#22331,.F.);
#29124=ORIENTED_EDGE('',*,*,#21530,.F.);
#29125=ORIENTED_EDGE('',*,*,#20989,.T.);
#29126=ORIENTED_EDGE('',*,*,#21471,.T.);
#29127=ORIENTED_EDGE('',*,*,#22332,.F.);
#29128=ORIENTED_EDGE('',*,*,#21532,.F.);
#29129=ORIENTED_EDGE('',*,*,#21534,.T.);
#29130=ORIENTED_EDGE('',*,*,#22333,.T.);
#29131=ORIENTED_EDGE('',*,*,#21472,.F.);
#29132=ORIENTED_EDGE('',*,*,#20987,.F.);
#29133=ORIENTED_EDGE('',*,*,#22332,.T.);
#29134=ORIENTED_EDGE('',*,*,#21473,.T.);
#29135=ORIENTED_EDGE('',*,*,#22333,.F.);
#29136=ORIENTED_EDGE('',*,*,#21533,.F.);
#29137=ORIENTED_EDGE('',*,*,#20985,.T.);
#29138=ORIENTED_EDGE('',*,*,#21468,.T.);
#29139=ORIENTED_EDGE('',*,*,#22334,.F.);
#29140=ORIENTED_EDGE('',*,*,#21535,.F.);
#29141=ORIENTED_EDGE('',*,*,#21537,.T.);
#29142=ORIENTED_EDGE('',*,*,#22335,.T.);
#29143=ORIENTED_EDGE('',*,*,#21469,.F.);
#29144=ORIENTED_EDGE('',*,*,#20983,.F.);
#29145=ORIENTED_EDGE('',*,*,#22334,.T.);
#29146=ORIENTED_EDGE('',*,*,#21470,.T.);
#29147=ORIENTED_EDGE('',*,*,#22335,.F.);
#29148=ORIENTED_EDGE('',*,*,#21536,.F.);
#29149=ORIENTED_EDGE('',*,*,#20981,.T.);
#29150=ORIENTED_EDGE('',*,*,#21465,.T.);
#29151=ORIENTED_EDGE('',*,*,#22336,.F.);
#29152=ORIENTED_EDGE('',*,*,#21538,.F.);
#29153=ORIENTED_EDGE('',*,*,#21540,.T.);
#29154=ORIENTED_EDGE('',*,*,#22337,.T.);
#29155=ORIENTED_EDGE('',*,*,#21466,.F.);
#29156=ORIENTED_EDGE('',*,*,#20979,.F.);
#29157=ORIENTED_EDGE('',*,*,#22336,.T.);
#29158=ORIENTED_EDGE('',*,*,#21467,.T.);
#29159=ORIENTED_EDGE('',*,*,#22337,.F.);
#29160=ORIENTED_EDGE('',*,*,#21539,.F.);
#29161=ORIENTED_EDGE('',*,*,#20977,.T.);
#29162=ORIENTED_EDGE('',*,*,#21462,.T.);
#29163=ORIENTED_EDGE('',*,*,#22338,.F.);
#29164=ORIENTED_EDGE('',*,*,#21541,.F.);
#29165=ORIENTED_EDGE('',*,*,#21543,.T.);
#29166=ORIENTED_EDGE('',*,*,#22339,.T.);
#29167=ORIENTED_EDGE('',*,*,#21463,.F.);
#29168=ORIENTED_EDGE('',*,*,#20975,.F.);
#29169=ORIENTED_EDGE('',*,*,#22338,.T.);
#29170=ORIENTED_EDGE('',*,*,#21464,.T.);
#29171=ORIENTED_EDGE('',*,*,#22339,.F.);
#29172=ORIENTED_EDGE('',*,*,#21542,.F.);
#29173=ORIENTED_EDGE('',*,*,#22340,.T.);
#29174=ORIENTED_EDGE('',*,*,#21388,.T.);
#29175=ORIENTED_EDGE('',*,*,#20971,.F.);
#29176=ORIENTED_EDGE('',*,*,#21546,.F.);
#29177=ORIENTED_EDGE('',*,*,#21545,.T.);
#29178=ORIENTED_EDGE('',*,*,#22341,.T.);
#29179=ORIENTED_EDGE('',*,*,#21389,.F.);
#29180=ORIENTED_EDGE('',*,*,#22340,.F.);
#29181=ORIENTED_EDGE('',*,*,#21544,.T.);
#29182=ORIENTED_EDGE('',*,*,#20973,.T.);
#29183=ORIENTED_EDGE('',*,*,#21387,.F.);
#29184=ORIENTED_EDGE('',*,*,#22341,.F.);
#29185=ORIENTED_EDGE('',*,*,#22342,.T.);
#29186=ORIENTED_EDGE('',*,*,#21459,.T.);
#29187=ORIENTED_EDGE('',*,*,#20967,.F.);
#29188=ORIENTED_EDGE('',*,*,#21616,.F.);
#29189=ORIENTED_EDGE('',*,*,#22343,.T.);
#29190=ORIENTED_EDGE('',*,*,#21460,.T.);
#29191=ORIENTED_EDGE('',*,*,#22342,.F.);
#29192=ORIENTED_EDGE('',*,*,#21618,.F.);
#29193=ORIENTED_EDGE('',*,*,#21617,.T.);
#29194=ORIENTED_EDGE('',*,*,#20969,.T.);
#29195=ORIENTED_EDGE('',*,*,#21461,.F.);
#29196=ORIENTED_EDGE('',*,*,#22343,.F.);
#29197=ORIENTED_EDGE('',*,*,#21613,.T.);
#29198=ORIENTED_EDGE('',*,*,#22344,.T.);
#29199=ORIENTED_EDGE('',*,*,#21390,.F.);
#29200=ORIENTED_EDGE('',*,*,#20963,.F.);
#29201=ORIENTED_EDGE('',*,*,#21615,.T.);
#29202=ORIENTED_EDGE('',*,*,#22345,.T.);
#29203=ORIENTED_EDGE('',*,*,#21391,.F.);
#29204=ORIENTED_EDGE('',*,*,#22344,.F.);
#29205=ORIENTED_EDGE('',*,*,#20965,.T.);
#29206=ORIENTED_EDGE('',*,*,#21392,.T.);
#29207=ORIENTED_EDGE('',*,*,#22345,.F.);
#29208=ORIENTED_EDGE('',*,*,#21614,.F.);
#29209=ORIENTED_EDGE('',*,*,#21547,.T.);
#29210=ORIENTED_EDGE('',*,*,#22346,.T.);
#29211=ORIENTED_EDGE('',*,*,#21393,.F.);
#29212=ORIENTED_EDGE('',*,*,#20959,.F.);
#29213=ORIENTED_EDGE('',*,*,#21549,.T.);
#29214=ORIENTED_EDGE('',*,*,#22347,.T.);
#29215=ORIENTED_EDGE('',*,*,#21394,.F.);
#29216=ORIENTED_EDGE('',*,*,#22346,.F.);
#29217=ORIENTED_EDGE('',*,*,#20961,.T.);
#29218=ORIENTED_EDGE('',*,*,#21395,.T.);
#29219=ORIENTED_EDGE('',*,*,#22347,.F.);
#29220=ORIENTED_EDGE('',*,*,#21548,.F.);
#29221=ORIENTED_EDGE('',*,*,#22348,.T.);
#29222=ORIENTED_EDGE('',*,*,#21456,.T.);
#29223=ORIENTED_EDGE('',*,*,#20955,.F.);
#29224=ORIENTED_EDGE('',*,*,#21610,.F.);
#29225=ORIENTED_EDGE('',*,*,#22349,.T.);
#29226=ORIENTED_EDGE('',*,*,#21457,.T.);
#29227=ORIENTED_EDGE('',*,*,#22348,.F.);
#29228=ORIENTED_EDGE('',*,*,#21612,.F.);
#29229=ORIENTED_EDGE('',*,*,#21611,.T.);
#29230=ORIENTED_EDGE('',*,*,#20957,.T.);
#29231=ORIENTED_EDGE('',*,*,#21458,.F.);
#29232=ORIENTED_EDGE('',*,*,#22349,.F.);
#29233=ORIENTED_EDGE('',*,*,#21607,.T.);
#29234=ORIENTED_EDGE('',*,*,#22350,.T.);
#29235=ORIENTED_EDGE('',*,*,#21396,.F.);
#29236=ORIENTED_EDGE('',*,*,#20951,.F.);
#29237=ORIENTED_EDGE('',*,*,#21609,.T.);
#29238=ORIENTED_EDGE('',*,*,#22351,.T.);
#29239=ORIENTED_EDGE('',*,*,#21397,.F.);
#29240=ORIENTED_EDGE('',*,*,#22350,.F.);
#29241=ORIENTED_EDGE('',*,*,#20953,.T.);
#29242=ORIENTED_EDGE('',*,*,#21398,.T.);
#29243=ORIENTED_EDGE('',*,*,#22351,.F.);
#29244=ORIENTED_EDGE('',*,*,#21608,.F.);
#29245=ORIENTED_EDGE('',*,*,#22352,.T.);
#29246=ORIENTED_EDGE('',*,*,#21453,.T.);
#29247=ORIENTED_EDGE('',*,*,#20947,.F.);
#29248=ORIENTED_EDGE('',*,*,#21550,.F.);
#29249=ORIENTED_EDGE('',*,*,#22353,.T.);
#29250=ORIENTED_EDGE('',*,*,#21454,.T.);
#29251=ORIENTED_EDGE('',*,*,#22352,.F.);
#29252=ORIENTED_EDGE('',*,*,#21552,.F.);
#29253=ORIENTED_EDGE('',*,*,#21551,.T.);
#29254=ORIENTED_EDGE('',*,*,#20949,.T.);
#29255=ORIENTED_EDGE('',*,*,#21455,.F.);
#29256=ORIENTED_EDGE('',*,*,#22353,.F.);
#29257=ORIENTED_EDGE('',*,*,#22354,.T.);
#29258=ORIENTED_EDGE('',*,*,#21450,.T.);
#29259=ORIENTED_EDGE('',*,*,#20943,.F.);
#29260=ORIENTED_EDGE('',*,*,#21553,.F.);
#29261=ORIENTED_EDGE('',*,*,#22355,.T.);
#29262=ORIENTED_EDGE('',*,*,#21451,.T.);
#29263=ORIENTED_EDGE('',*,*,#22354,.F.);
#29264=ORIENTED_EDGE('',*,*,#21555,.F.);
#29265=ORIENTED_EDGE('',*,*,#21554,.T.);
#29266=ORIENTED_EDGE('',*,*,#20945,.T.);
#29267=ORIENTED_EDGE('',*,*,#21452,.F.);
#29268=ORIENTED_EDGE('',*,*,#22355,.F.);
#29269=ORIENTED_EDGE('',*,*,#21556,.T.);
#29270=ORIENTED_EDGE('',*,*,#22356,.T.);
#29271=ORIENTED_EDGE('',*,*,#21399,.F.);
#29272=ORIENTED_EDGE('',*,*,#20939,.F.);
#29273=ORIENTED_EDGE('',*,*,#21558,.T.);
#29274=ORIENTED_EDGE('',*,*,#22357,.T.);
#29275=ORIENTED_EDGE('',*,*,#21400,.F.);
#29276=ORIENTED_EDGE('',*,*,#22356,.F.);
#29277=ORIENTED_EDGE('',*,*,#20941,.T.);
#29278=ORIENTED_EDGE('',*,*,#21401,.T.);
#29279=ORIENTED_EDGE('',*,*,#22357,.F.);
#29280=ORIENTED_EDGE('',*,*,#21557,.F.);
#29281=ORIENTED_EDGE('',*,*,#21604,.T.);
#29282=ORIENTED_EDGE('',*,*,#22358,.T.);
#29283=ORIENTED_EDGE('',*,*,#21402,.F.);
#29284=ORIENTED_EDGE('',*,*,#20935,.F.);
#29285=ORIENTED_EDGE('',*,*,#21606,.T.);
#29286=ORIENTED_EDGE('',*,*,#22359,.T.);
#29287=ORIENTED_EDGE('',*,*,#21403,.F.);
#29288=ORIENTED_EDGE('',*,*,#22358,.F.);
#29289=ORIENTED_EDGE('',*,*,#20937,.T.);
#29290=ORIENTED_EDGE('',*,*,#21404,.T.);
#29291=ORIENTED_EDGE('',*,*,#22359,.F.);
#29292=ORIENTED_EDGE('',*,*,#21605,.F.);
#29293=ORIENTED_EDGE('',*,*,#21559,.T.);
#29294=ORIENTED_EDGE('',*,*,#22360,.T.);
#29295=ORIENTED_EDGE('',*,*,#21405,.F.);
#29296=ORIENTED_EDGE('',*,*,#20931,.F.);
#29297=ORIENTED_EDGE('',*,*,#21561,.T.);
#29298=ORIENTED_EDGE('',*,*,#22361,.T.);
#29299=ORIENTED_EDGE('',*,*,#21406,.F.);
#29300=ORIENTED_EDGE('',*,*,#22360,.F.);
#29301=ORIENTED_EDGE('',*,*,#20933,.T.);
#29302=ORIENTED_EDGE('',*,*,#21407,.T.);
#29303=ORIENTED_EDGE('',*,*,#22361,.F.);
#29304=ORIENTED_EDGE('',*,*,#21560,.F.);
#29305=ORIENTED_EDGE('',*,*,#21601,.T.);
#29306=ORIENTED_EDGE('',*,*,#22362,.T.);
#29307=ORIENTED_EDGE('',*,*,#21408,.F.);
#29308=ORIENTED_EDGE('',*,*,#20927,.F.);
#29309=ORIENTED_EDGE('',*,*,#21603,.T.);
#29310=ORIENTED_EDGE('',*,*,#22363,.T.);
#29311=ORIENTED_EDGE('',*,*,#21409,.F.);
#29312=ORIENTED_EDGE('',*,*,#22362,.F.);
#29313=ORIENTED_EDGE('',*,*,#20929,.T.);
#29314=ORIENTED_EDGE('',*,*,#21410,.T.);
#29315=ORIENTED_EDGE('',*,*,#22363,.F.);
#29316=ORIENTED_EDGE('',*,*,#21602,.F.);
#29317=ORIENTED_EDGE('',*,*,#22364,.T.);
#29318=ORIENTED_EDGE('',*,*,#21447,.T.);
#29319=ORIENTED_EDGE('',*,*,#20923,.F.);
#29320=ORIENTED_EDGE('',*,*,#21562,.F.);
#29321=ORIENTED_EDGE('',*,*,#22365,.T.);
#29322=ORIENTED_EDGE('',*,*,#21448,.T.);
#29323=ORIENTED_EDGE('',*,*,#22364,.F.);
#29324=ORIENTED_EDGE('',*,*,#21564,.F.);
#29325=ORIENTED_EDGE('',*,*,#21563,.T.);
#29326=ORIENTED_EDGE('',*,*,#20925,.T.);
#29327=ORIENTED_EDGE('',*,*,#21449,.F.);
#29328=ORIENTED_EDGE('',*,*,#22365,.F.);
#29329=ORIENTED_EDGE('',*,*,#22366,.T.);
#29330=ORIENTED_EDGE('',*,*,#21444,.T.);
#29331=ORIENTED_EDGE('',*,*,#20919,.F.);
#29332=ORIENTED_EDGE('',*,*,#21565,.F.);
#29333=ORIENTED_EDGE('',*,*,#22367,.T.);
#29334=ORIENTED_EDGE('',*,*,#21445,.T.);
#29335=ORIENTED_EDGE('',*,*,#22366,.F.);
#29336=ORIENTED_EDGE('',*,*,#21567,.F.);
#29337=ORIENTED_EDGE('',*,*,#21566,.T.);
#29338=ORIENTED_EDGE('',*,*,#20921,.T.);
#29339=ORIENTED_EDGE('',*,*,#21446,.F.);
#29340=ORIENTED_EDGE('',*,*,#22367,.F.);
#29341=ORIENTED_EDGE('',*,*,#22368,.T.);
#29342=ORIENTED_EDGE('',*,*,#21441,.T.);
#29343=ORIENTED_EDGE('',*,*,#20915,.F.);
#29344=ORIENTED_EDGE('',*,*,#21568,.F.);
#29345=ORIENTED_EDGE('',*,*,#22369,.T.);
#29346=ORIENTED_EDGE('',*,*,#21442,.T.);
#29347=ORIENTED_EDGE('',*,*,#22368,.F.);
#29348=ORIENTED_EDGE('',*,*,#21570,.F.);
#29349=ORIENTED_EDGE('',*,*,#21569,.T.);
#29350=ORIENTED_EDGE('',*,*,#20917,.T.);
#29351=ORIENTED_EDGE('',*,*,#21443,.F.);
#29352=ORIENTED_EDGE('',*,*,#22369,.F.);
#29353=ORIENTED_EDGE('',*,*,#22370,.T.);
#29354=ORIENTED_EDGE('',*,*,#21438,.T.);
#29355=ORIENTED_EDGE('',*,*,#20911,.F.);
#29356=ORIENTED_EDGE('',*,*,#21571,.F.);
#29357=ORIENTED_EDGE('',*,*,#22371,.T.);
#29358=ORIENTED_EDGE('',*,*,#21439,.T.);
#29359=ORIENTED_EDGE('',*,*,#22370,.F.);
#29360=ORIENTED_EDGE('',*,*,#21573,.F.);
#29361=ORIENTED_EDGE('',*,*,#21572,.T.);
#29362=ORIENTED_EDGE('',*,*,#20913,.T.);
#29363=ORIENTED_EDGE('',*,*,#21440,.F.);
#29364=ORIENTED_EDGE('',*,*,#22371,.F.);
#29365=ORIENTED_EDGE('',*,*,#22372,.T.);
#29366=ORIENTED_EDGE('',*,*,#21435,.T.);
#29367=ORIENTED_EDGE('',*,*,#20907,.F.);
#29368=ORIENTED_EDGE('',*,*,#21574,.F.);
#29369=ORIENTED_EDGE('',*,*,#22373,.T.);
#29370=ORIENTED_EDGE('',*,*,#21436,.T.);
#29371=ORIENTED_EDGE('',*,*,#22372,.F.);
#29372=ORIENTED_EDGE('',*,*,#21576,.F.);
#29373=ORIENTED_EDGE('',*,*,#21575,.T.);
#29374=ORIENTED_EDGE('',*,*,#20909,.T.);
#29375=ORIENTED_EDGE('',*,*,#21437,.F.);
#29376=ORIENTED_EDGE('',*,*,#22373,.F.);
#29377=ORIENTED_EDGE('',*,*,#22374,.T.);
#29378=ORIENTED_EDGE('',*,*,#21432,.T.);
#29379=ORIENTED_EDGE('',*,*,#20903,.F.);
#29380=ORIENTED_EDGE('',*,*,#21577,.F.);
#29381=ORIENTED_EDGE('',*,*,#22375,.T.);
#29382=ORIENTED_EDGE('',*,*,#21433,.T.);
#29383=ORIENTED_EDGE('',*,*,#22374,.F.);
#29384=ORIENTED_EDGE('',*,*,#21579,.F.);
#29385=ORIENTED_EDGE('',*,*,#21578,.T.);
#29386=ORIENTED_EDGE('',*,*,#20905,.T.);
#29387=ORIENTED_EDGE('',*,*,#21434,.F.);
#29388=ORIENTED_EDGE('',*,*,#22375,.F.);
#29389=ORIENTED_EDGE('',*,*,#22376,.T.);
#29390=ORIENTED_EDGE('',*,*,#21429,.T.);
#29391=ORIENTED_EDGE('',*,*,#20899,.F.);
#29392=ORIENTED_EDGE('',*,*,#21580,.F.);
#29393=ORIENTED_EDGE('',*,*,#22377,.T.);
#29394=ORIENTED_EDGE('',*,*,#21430,.T.);
#29395=ORIENTED_EDGE('',*,*,#22376,.F.);
#29396=ORIENTED_EDGE('',*,*,#21582,.F.);
#29397=ORIENTED_EDGE('',*,*,#21581,.T.);
#29398=ORIENTED_EDGE('',*,*,#20901,.T.);
#29399=ORIENTED_EDGE('',*,*,#21431,.F.);
#29400=ORIENTED_EDGE('',*,*,#22377,.F.);
#29401=ORIENTED_EDGE('',*,*,#21583,.T.);
#29402=ORIENTED_EDGE('',*,*,#22378,.T.);
#29403=ORIENTED_EDGE('',*,*,#21411,.F.);
#29404=ORIENTED_EDGE('',*,*,#20895,.F.);
#29405=ORIENTED_EDGE('',*,*,#21585,.T.);
#29406=ORIENTED_EDGE('',*,*,#22379,.T.);
#29407=ORIENTED_EDGE('',*,*,#21412,.F.);
#29408=ORIENTED_EDGE('',*,*,#22378,.F.);
#29409=ORIENTED_EDGE('',*,*,#20897,.T.);
#29410=ORIENTED_EDGE('',*,*,#21413,.T.);
#29411=ORIENTED_EDGE('',*,*,#22379,.F.);
#29412=ORIENTED_EDGE('',*,*,#21584,.F.);
#29413=ORIENTED_EDGE('',*,*,#21598,.T.);
#29414=ORIENTED_EDGE('',*,*,#22380,.T.);
#29415=ORIENTED_EDGE('',*,*,#21414,.F.);
#29416=ORIENTED_EDGE('',*,*,#20891,.F.);
#29417=ORIENTED_EDGE('',*,*,#21600,.T.);
#29418=ORIENTED_EDGE('',*,*,#22381,.T.);
#29419=ORIENTED_EDGE('',*,*,#21415,.F.);
#29420=ORIENTED_EDGE('',*,*,#22380,.F.);
#29421=ORIENTED_EDGE('',*,*,#20893,.T.);
#29422=ORIENTED_EDGE('',*,*,#21416,.T.);
#29423=ORIENTED_EDGE('',*,*,#22381,.F.);
#29424=ORIENTED_EDGE('',*,*,#21599,.F.);
#29425=ORIENTED_EDGE('',*,*,#21586,.T.);
#29426=ORIENTED_EDGE('',*,*,#22382,.T.);
#29427=ORIENTED_EDGE('',*,*,#21417,.F.);
#29428=ORIENTED_EDGE('',*,*,#20887,.F.);
#29429=ORIENTED_EDGE('',*,*,#21588,.T.);
#29430=ORIENTED_EDGE('',*,*,#22383,.T.);
#29431=ORIENTED_EDGE('',*,*,#21418,.F.);
#29432=ORIENTED_EDGE('',*,*,#22382,.F.);
#29433=ORIENTED_EDGE('',*,*,#20889,.T.);
#29434=ORIENTED_EDGE('',*,*,#21419,.T.);
#29435=ORIENTED_EDGE('',*,*,#22383,.F.);
#29436=ORIENTED_EDGE('',*,*,#21587,.F.);
#29437=ORIENTED_EDGE('',*,*,#21595,.T.);
#29438=ORIENTED_EDGE('',*,*,#22384,.T.);
#29439=ORIENTED_EDGE('',*,*,#21420,.F.);
#29440=ORIENTED_EDGE('',*,*,#20883,.F.);
#29441=ORIENTED_EDGE('',*,*,#21597,.T.);
#29442=ORIENTED_EDGE('',*,*,#22385,.T.);
#29443=ORIENTED_EDGE('',*,*,#21421,.F.);
#29444=ORIENTED_EDGE('',*,*,#22384,.F.);
#29445=ORIENTED_EDGE('',*,*,#20885,.T.);
#29446=ORIENTED_EDGE('',*,*,#21422,.T.);
#29447=ORIENTED_EDGE('',*,*,#22385,.F.);
#29448=ORIENTED_EDGE('',*,*,#21596,.F.);
#29449=ORIENTED_EDGE('',*,*,#21589,.T.);
#29450=ORIENTED_EDGE('',*,*,#22386,.T.);
#29451=ORIENTED_EDGE('',*,*,#21423,.F.);
#29452=ORIENTED_EDGE('',*,*,#20879,.F.);
#29453=ORIENTED_EDGE('',*,*,#21591,.T.);
#29454=ORIENTED_EDGE('',*,*,#22387,.T.);
#29455=ORIENTED_EDGE('',*,*,#21424,.F.);
#29456=ORIENTED_EDGE('',*,*,#22386,.F.);
#29457=ORIENTED_EDGE('',*,*,#20881,.T.);
#29458=ORIENTED_EDGE('',*,*,#21425,.T.);
#29459=ORIENTED_EDGE('',*,*,#22387,.F.);
#29460=ORIENTED_EDGE('',*,*,#21590,.F.);
#29461=ORIENTED_EDGE('',*,*,#22388,.T.);
#29462=ORIENTED_EDGE('',*,*,#21426,.T.);
#29463=ORIENTED_EDGE('',*,*,#20875,.F.);
#29464=ORIENTED_EDGE('',*,*,#21592,.F.);
#29465=ORIENTED_EDGE('',*,*,#22389,.T.);
#29466=ORIENTED_EDGE('',*,*,#21427,.T.);
#29467=ORIENTED_EDGE('',*,*,#22388,.F.);
#29468=ORIENTED_EDGE('',*,*,#21594,.F.);
#29469=ORIENTED_EDGE('',*,*,#21593,.T.);
#29470=ORIENTED_EDGE('',*,*,#20877,.T.);
#29471=ORIENTED_EDGE('',*,*,#21428,.F.);
#29472=ORIENTED_EDGE('',*,*,#22389,.F.);
#29473=ORIENTED_EDGE('',*,*,#21271,.F.);
#29474=ORIENTED_EDGE('',*,*,#21340,.F.);
#29475=ORIENTED_EDGE('',*,*,#21210,.T.);
#29476=ORIENTED_EDGE('',*,*,#22390,.T.);
#29477=ORIENTED_EDGE('',*,*,#21272,.F.);
#29478=ORIENTED_EDGE('',*,*,#22390,.F.);
#29479=ORIENTED_EDGE('',*,*,#21209,.T.);
#29480=ORIENTED_EDGE('',*,*,#22391,.T.);
#29481=ORIENTED_EDGE('',*,*,#21273,.F.);
#29482=ORIENTED_EDGE('',*,*,#22391,.F.);
#29483=ORIENTED_EDGE('',*,*,#21208,.T.);
#29484=ORIENTED_EDGE('',*,*,#22392,.T.);
#29485=ORIENTED_EDGE('',*,*,#21275,.F.);
#29486=ORIENTED_EDGE('',*,*,#22393,.F.);
#29487=ORIENTED_EDGE('',*,*,#21206,.T.);
#29488=ORIENTED_EDGE('',*,*,#22394,.T.);
#29489=ORIENTED_EDGE('',*,*,#21276,.F.);
#29490=ORIENTED_EDGE('',*,*,#22394,.F.);
#29491=ORIENTED_EDGE('',*,*,#21205,.T.);
#29492=ORIENTED_EDGE('',*,*,#22395,.T.);
#29493=ORIENTED_EDGE('',*,*,#21277,.F.);
#29494=ORIENTED_EDGE('',*,*,#22395,.F.);
#29495=ORIENTED_EDGE('',*,*,#21204,.T.);
#29496=ORIENTED_EDGE('',*,*,#21342,.T.);
#29497=ORIENTED_EDGE('',*,*,#22396,.F.);
#29498=ORIENTED_EDGE('',*,*,#22397,.F.);
#29499=ORIENTED_EDGE('',*,*,#22393,.T.);
#29500=ORIENTED_EDGE('',*,*,#22398,.T.);
#29501=ORIENTED_EDGE('',*,*,#22399,.F.);
#29502=ORIENTED_EDGE('',*,*,#22400,.T.);
#29503=ORIENTED_EDGE('',*,*,#22401,.T.);
#29504=ORIENTED_EDGE('',*,*,#22392,.F.);
#29505=ORIENTED_EDGE('',*,*,#21274,.F.);
#29506=ORIENTED_EDGE('',*,*,#22401,.F.);
#29507=ORIENTED_EDGE('',*,*,#21326,.T.);
#29508=ORIENTED_EDGE('',*,*,#22398,.F.);
#29509=ORIENTED_EDGE('',*,*,#21207,.T.);
#29510=ORIENTED_EDGE('',*,*,#22397,.T.);
#29511=ORIENTED_EDGE('',*,*,#21305,.T.);
#29512=ORIENTED_EDGE('',*,*,#22399,.T.);
#29513=ORIENTED_EDGE('',*,*,#22400,.F.);
#29514=ORIENTED_EDGE('',*,*,#21304,.T.);
#29515=ORIENTED_EDGE('',*,*,#22402,.F.);
#29516=ORIENTED_EDGE('',*,*,#21327,.F.);
#29517=ORIENTED_EDGE('',*,*,#22396,.T.);
#29518=ORIENTED_EDGE('',*,*,#21331,.F.);
#29519=ORIENTED_EDGE('',*,*,#22403,.T.);
#29520=ORIENTED_EDGE('',*,*,#21306,.T.);
#29521=ORIENTED_EDGE('',*,*,#21309,.T.);
#29522=ORIENTED_EDGE('',*,*,#22404,.F.);
#29523=ORIENTED_EDGE('',*,*,#21328,.F.);
#29524=ORIENTED_EDGE('',*,*,#22402,.T.);
#29525=ORIENTED_EDGE('',*,*,#21308,.T.);
#29526=ORIENTED_EDGE('',*,*,#22405,.F.);
#29527=ORIENTED_EDGE('',*,*,#21329,.F.);
#29528=ORIENTED_EDGE('',*,*,#22404,.T.);
#29529=ORIENTED_EDGE('',*,*,#21307,.T.);
#29530=ORIENTED_EDGE('',*,*,#22403,.F.);
#29531=ORIENTED_EDGE('',*,*,#21330,.F.);
#29532=ORIENTED_EDGE('',*,*,#22405,.T.);
#29533=ORIENTED_EDGE('',*,*,#22406,.F.);
#29534=ORIENTED_EDGE('',*,*,#21332,.T.);
#29535=ORIENTED_EDGE('',*,*,#22407,.F.);
#29536=ORIENTED_EDGE('',*,*,#21316,.F.);
#29537=ORIENTED_EDGE('',*,*,#21312,.T.);
#29538=ORIENTED_EDGE('',*,*,#22408,.F.);
#29539=ORIENTED_EDGE('',*,*,#21334,.F.);
#29540=ORIENTED_EDGE('',*,*,#22409,.F.);
#29541=ORIENTED_EDGE('',*,*,#22409,.T.);
#29542=ORIENTED_EDGE('',*,*,#21333,.T.);
#29543=ORIENTED_EDGE('',*,*,#22406,.T.);
#29544=ORIENTED_EDGE('',*,*,#22410,.T.);
#29545=ORIENTED_EDGE('',*,*,#22411,.T.);
#29546=ORIENTED_EDGE('',*,*,#22412,.T.);
#29547=ORIENTED_EDGE('',*,*,#22407,.T.);
#29548=ORIENTED_EDGE('',*,*,#21335,.T.);
#29549=ORIENTED_EDGE('',*,*,#22408,.T.);
#29550=ORIENTED_EDGE('',*,*,#22413,.T.);
#29551=ORIENTED_EDGE('',*,*,#22414,.T.);
#29552=ORIENTED_EDGE('',*,*,#22415,.T.);
#29553=ORIENTED_EDGE('',*,*,#21311,.F.);
#29554=ORIENTED_EDGE('',*,*,#22416,.T.);
#29555=ORIENTED_EDGE('',*,*,#22417,.T.);
#29556=ORIENTED_EDGE('',*,*,#22418,.T.);
#29557=ORIENTED_EDGE('',*,*,#22419,.T.);
#29558=ORIENTED_EDGE('',*,*,#22420,.T.);
#29559=ORIENTED_EDGE('',*,*,#22421,.T.);
#29560=ORIENTED_EDGE('',*,*,#22422,.T.);
#29561=ORIENTED_EDGE('',*,*,#21313,.F.);
#29562=ORIENTED_EDGE('',*,*,#22412,.F.);
#29563=ORIENTED_EDGE('',*,*,#22423,.F.);
#29564=ORIENTED_EDGE('',*,*,#22424,.F.);
#29565=ORIENTED_EDGE('',*,*,#22425,.F.);
#29566=ORIENTED_EDGE('',*,*,#22426,.F.);
#29567=ORIENTED_EDGE('',*,*,#22427,.F.);
#29568=ORIENTED_EDGE('',*,*,#22413,.F.);
#29569=ORIENTED_EDGE('',*,*,#21315,.F.);
#29570=ORIENTED_EDGE('',*,*,#22428,.T.);
#29571=ORIENTED_EDGE('',*,*,#22429,.F.);
#29572=ORIENTED_EDGE('',*,*,#22430,.T.);
#29573=ORIENTED_EDGE('',*,*,#22431,.F.);
#29574=ORIENTED_EDGE('',*,*,#22432,.T.);
#29575=ORIENTED_EDGE('',*,*,#22433,.F.);
#29576=ORIENTED_EDGE('',*,*,#22434,.T.);
#29577=ORIENTED_EDGE('',*,*,#21317,.F.);
#29578=ORIENTED_EDGE('',*,*,#22415,.F.);
#29579=ORIENTED_EDGE('',*,*,#22435,.T.);
#29580=ORIENTED_EDGE('',*,*,#22436,.F.);
#29581=ORIENTED_EDGE('',*,*,#22437,.T.);
#29582=ORIENTED_EDGE('',*,*,#22438,.F.);
#29583=ORIENTED_EDGE('',*,*,#22439,.T.);
#29584=ORIENTED_EDGE('',*,*,#22410,.F.);
#29585=ORIENTED_EDGE('',*,*,#22438,.T.);
#29586=ORIENTED_EDGE('',*,*,#22440,.T.);
#29587=ORIENTED_EDGE('',*,*,#22424,.T.);
#29588=ORIENTED_EDGE('',*,*,#22441,.T.);
#29589=ORIENTED_EDGE('',*,*,#22436,.T.);
#29590=ORIENTED_EDGE('',*,*,#22442,.T.);
#29591=ORIENTED_EDGE('',*,*,#22426,.T.);
#29592=ORIENTED_EDGE('',*,*,#22443,.T.);
#29593=ORIENTED_EDGE('',*,*,#22423,.T.);
#29594=ORIENTED_EDGE('',*,*,#22411,.F.);
#29595=ORIENTED_EDGE('',*,*,#22439,.F.);
#29596=ORIENTED_EDGE('',*,*,#22441,.F.);
#29597=ORIENTED_EDGE('',*,*,#22435,.F.);
#29598=ORIENTED_EDGE('',*,*,#22414,.F.);
#29599=ORIENTED_EDGE('',*,*,#22427,.T.);
#29600=ORIENTED_EDGE('',*,*,#22442,.F.);
#29601=ORIENTED_EDGE('',*,*,#22425,.T.);
#29602=ORIENTED_EDGE('',*,*,#22440,.F.);
#29603=ORIENTED_EDGE('',*,*,#22437,.F.);
#29604=ORIENTED_EDGE('',*,*,#22443,.F.);
#29605=ORIENTED_EDGE('',*,*,#20871,.F.);
#29606=ORIENTED_EDGE('',*,*,#22430,.F.);
#29607=ORIENTED_EDGE('',*,*,#22444,.F.);
#29608=ORIENTED_EDGE('',*,*,#22420,.F.);
#29609=ORIENTED_EDGE('',*,*,#22445,.F.);
#29610=ORIENTED_EDGE('',*,*,#22432,.F.);
#29611=ORIENTED_EDGE('',*,*,#22446,.F.);
#29612=ORIENTED_EDGE('',*,*,#22418,.F.);
#29613=ORIENTED_EDGE('',*,*,#22447,.F.);
#29614=ORIENTED_EDGE('',*,*,#22434,.F.);
#29615=ORIENTED_EDGE('',*,*,#22448,.F.);
#29616=ORIENTED_EDGE('',*,*,#22416,.F.);
#29617=ORIENTED_EDGE('',*,*,#21310,.F.);
#29618=ORIENTED_EDGE('',*,*,#22428,.F.);
#29619=ORIENTED_EDGE('',*,*,#21314,.F.);
#29620=ORIENTED_EDGE('',*,*,#22422,.F.);
#29621=ORIENTED_EDGE('',*,*,#22449,.F.);
#29622=ORIENTED_EDGE('',*,*,#22421,.F.);
#29623=ORIENTED_EDGE('',*,*,#22444,.T.);
#29624=ORIENTED_EDGE('',*,*,#22429,.T.);
#29625=ORIENTED_EDGE('',*,*,#22449,.T.);
#29626=ORIENTED_EDGE('',*,*,#22433,.T.);
#29627=ORIENTED_EDGE('',*,*,#22447,.T.);
#29628=ORIENTED_EDGE('',*,*,#22417,.F.);
#29629=ORIENTED_EDGE('',*,*,#22448,.T.);
#29630=ORIENTED_EDGE('',*,*,#22419,.F.);
#29631=ORIENTED_EDGE('',*,*,#22446,.T.);
#29632=ORIENTED_EDGE('',*,*,#22431,.T.);
#29633=ORIENTED_EDGE('',*,*,#22445,.T.);
#29634=ORIENTED_EDGE('',*,*,#20873,.T.);
#29635=ORIENTED_EDGE('',*,*,#22450,.T.);
#29636=ORIENTED_EDGE('',*,*,#21337,.F.);
#29637=ORIENTED_EDGE('',*,*,#22451,.T.);
#29638=ORIENTED_EDGE('',*,*,#21324,.F.);
#29639=ORIENTED_EDGE('',*,*,#21320,.T.);
#29640=ORIENTED_EDGE('',*,*,#22452,.T.);
#29641=ORIENTED_EDGE('',*,*,#21339,.T.);
#29642=ORIENTED_EDGE('',*,*,#22453,.T.);
#29643=ORIENTED_EDGE('',*,*,#22451,.F.);
#29644=ORIENTED_EDGE('',*,*,#21336,.F.);
#29645=ORIENTED_EDGE('',*,*,#22452,.F.);
#29646=ORIENTED_EDGE('',*,*,#22454,.F.);
#29647=ORIENTED_EDGE('',*,*,#22455,.F.);
#29648=ORIENTED_EDGE('',*,*,#22456,.F.);
#29649=ORIENTED_EDGE('',*,*,#22453,.F.);
#29650=ORIENTED_EDGE('',*,*,#21338,.F.);
#29651=ORIENTED_EDGE('',*,*,#22450,.F.);
#29652=ORIENTED_EDGE('',*,*,#22457,.F.);
#29653=ORIENTED_EDGE('',*,*,#22458,.F.);
#29654=ORIENTED_EDGE('',*,*,#22459,.F.);
#29655=ORIENTED_EDGE('',*,*,#21319,.F.);
#29656=ORIENTED_EDGE('',*,*,#22460,.F.);
#29657=ORIENTED_EDGE('',*,*,#22461,.F.);
#29658=ORIENTED_EDGE('',*,*,#22462,.F.);
#29659=ORIENTED_EDGE('',*,*,#22463,.F.);
#29660=ORIENTED_EDGE('',*,*,#22464,.F.);
#29661=ORIENTED_EDGE('',*,*,#22465,.F.);
#29662=ORIENTED_EDGE('',*,*,#22466,.F.);
#29663=ORIENTED_EDGE('',*,*,#21321,.F.);
#29664=ORIENTED_EDGE('',*,*,#22459,.T.);
#29665=ORIENTED_EDGE('',*,*,#22467,.T.);
#29666=ORIENTED_EDGE('',*,*,#22468,.T.);
#29667=ORIENTED_EDGE('',*,*,#22469,.T.);
#29668=ORIENTED_EDGE('',*,*,#22470,.T.);
#29669=ORIENTED_EDGE('',*,*,#22471,.T.);
#29670=ORIENTED_EDGE('',*,*,#22454,.T.);
#29671=ORIENTED_EDGE('',*,*,#21323,.F.);
#29672=ORIENTED_EDGE('',*,*,#22472,.F.);
#29673=ORIENTED_EDGE('',*,*,#22473,.T.);
#29674=ORIENTED_EDGE('',*,*,#22474,.F.);
#29675=ORIENTED_EDGE('',*,*,#22475,.T.);
#29676=ORIENTED_EDGE('',*,*,#22476,.F.);
#29677=ORIENTED_EDGE('',*,*,#22477,.T.);
#29678=ORIENTED_EDGE('',*,*,#22478,.F.);
#29679=ORIENTED_EDGE('',*,*,#21325,.F.);
#29680=ORIENTED_EDGE('',*,*,#22456,.T.);
#29681=ORIENTED_EDGE('',*,*,#22479,.F.);
#29682=ORIENTED_EDGE('',*,*,#22480,.T.);
#29683=ORIENTED_EDGE('',*,*,#22481,.F.);
#29684=ORIENTED_EDGE('',*,*,#22482,.T.);
#29685=ORIENTED_EDGE('',*,*,#22483,.F.);
#29686=ORIENTED_EDGE('',*,*,#22457,.T.);
#29687=ORIENTED_EDGE('',*,*,#22480,.F.);
#29688=ORIENTED_EDGE('',*,*,#22484,.F.);
#29689=ORIENTED_EDGE('',*,*,#22470,.F.);
#29690=ORIENTED_EDGE('',*,*,#22485,.F.);
#29691=ORIENTED_EDGE('',*,*,#22482,.F.);
#29692=ORIENTED_EDGE('',*,*,#22486,.F.);
#29693=ORIENTED_EDGE('',*,*,#22468,.F.);
#29694=ORIENTED_EDGE('',*,*,#22487,.F.);
#29695=ORIENTED_EDGE('',*,*,#22471,.F.);
#29696=ORIENTED_EDGE('',*,*,#22484,.T.);
#29697=ORIENTED_EDGE('',*,*,#22479,.T.);
#29698=ORIENTED_EDGE('',*,*,#22455,.T.);
#29699=ORIENTED_EDGE('',*,*,#22483,.T.);
#29700=ORIENTED_EDGE('',*,*,#22487,.T.);
#29701=ORIENTED_EDGE('',*,*,#22467,.F.);
#29702=ORIENTED_EDGE('',*,*,#22458,.T.);
#29703=ORIENTED_EDGE('',*,*,#22469,.F.);
#29704=ORIENTED_EDGE('',*,*,#22486,.T.);
#29705=ORIENTED_EDGE('',*,*,#22481,.T.);
#29706=ORIENTED_EDGE('',*,*,#22485,.T.);
#29707=ORIENTED_EDGE('',*,*,#20868,.T.);
#29708=ORIENTED_EDGE('',*,*,#22476,.T.);
#29709=ORIENTED_EDGE('',*,*,#22488,.T.);
#29710=ORIENTED_EDGE('',*,*,#22462,.T.);
#29711=ORIENTED_EDGE('',*,*,#22489,.T.);
#29712=ORIENTED_EDGE('',*,*,#22474,.T.);
#29713=ORIENTED_EDGE('',*,*,#22490,.T.);
#29714=ORIENTED_EDGE('',*,*,#22464,.T.);
#29715=ORIENTED_EDGE('',*,*,#22491,.T.);
#29716=ORIENTED_EDGE('',*,*,#22472,.T.);
#29717=ORIENTED_EDGE('',*,*,#21322,.T.);
#29718=ORIENTED_EDGE('',*,*,#22466,.T.);
#29719=ORIENTED_EDGE('',*,*,#22492,.T.);
#29720=ORIENTED_EDGE('',*,*,#22478,.T.);
#29721=ORIENTED_EDGE('',*,*,#22493,.T.);
#29722=ORIENTED_EDGE('',*,*,#22460,.T.);
#29723=ORIENTED_EDGE('',*,*,#21318,.T.);
#29724=ORIENTED_EDGE('',*,*,#22461,.T.);
#29725=ORIENTED_EDGE('',*,*,#22493,.F.);
#29726=ORIENTED_EDGE('',*,*,#22477,.F.);
#29727=ORIENTED_EDGE('',*,*,#22489,.F.);
#29728=ORIENTED_EDGE('',*,*,#22473,.F.);
#29729=ORIENTED_EDGE('',*,*,#22492,.F.);
#29730=ORIENTED_EDGE('',*,*,#22465,.T.);
#29731=ORIENTED_EDGE('',*,*,#22490,.F.);
#29732=ORIENTED_EDGE('',*,*,#22463,.T.);
#29733=ORIENTED_EDGE('',*,*,#22488,.F.);
#29734=ORIENTED_EDGE('',*,*,#22475,.F.);
#29735=ORIENTED_EDGE('',*,*,#22491,.F.);
#29736=ORIENTED_EDGE('',*,*,#20870,.F.);
#29737=ORIENTED_EDGE('',*,*,#21257,.F.);
#29738=ORIENTED_EDGE('',*,*,#21300,.F.);
#29739=ORIENTED_EDGE('',*,*,#21196,.T.);
#29740=ORIENTED_EDGE('',*,*,#22494,.T.);
#29741=ORIENTED_EDGE('',*,*,#21258,.F.);
#29742=ORIENTED_EDGE('',*,*,#22494,.F.);
#29743=ORIENTED_EDGE('',*,*,#21223,.T.);
#29744=ORIENTED_EDGE('',*,*,#22495,.T.);
#29745=ORIENTED_EDGE('',*,*,#21259,.F.);
#29746=ORIENTED_EDGE('',*,*,#22495,.F.);
#29747=ORIENTED_EDGE('',*,*,#21222,.T.);
#29748=ORIENTED_EDGE('',*,*,#22496,.T.);
#29749=ORIENTED_EDGE('',*,*,#21261,.F.);
#29750=ORIENTED_EDGE('',*,*,#22497,.F.);
#29751=ORIENTED_EDGE('',*,*,#21220,.T.);
#29752=ORIENTED_EDGE('',*,*,#22498,.T.);
#29753=ORIENTED_EDGE('',*,*,#21262,.F.);
#29754=ORIENTED_EDGE('',*,*,#22498,.F.);
#29755=ORIENTED_EDGE('',*,*,#21219,.T.);
#29756=ORIENTED_EDGE('',*,*,#22499,.T.);
#29757=ORIENTED_EDGE('',*,*,#21263,.F.);
#29758=ORIENTED_EDGE('',*,*,#22499,.F.);
#29759=ORIENTED_EDGE('',*,*,#21218,.T.);
#29760=ORIENTED_EDGE('',*,*,#21302,.T.);
#29761=ORIENTED_EDGE('',*,*,#22500,.F.);
#29762=ORIENTED_EDGE('',*,*,#22501,.F.);
#29763=ORIENTED_EDGE('',*,*,#22497,.T.);
#29764=ORIENTED_EDGE('',*,*,#22502,.T.);
#29765=ORIENTED_EDGE('',*,*,#22503,.F.);
#29766=ORIENTED_EDGE('',*,*,#22504,.T.);
#29767=ORIENTED_EDGE('',*,*,#22505,.T.);
#29768=ORIENTED_EDGE('',*,*,#22496,.F.);
#29769=ORIENTED_EDGE('',*,*,#21260,.F.);
#29770=ORIENTED_EDGE('',*,*,#22505,.F.);
#29771=ORIENTED_EDGE('',*,*,#22506,.T.);
#29772=ORIENTED_EDGE('',*,*,#22502,.F.);
#29773=ORIENTED_EDGE('',*,*,#21221,.T.);
#29774=ORIENTED_EDGE('',*,*,#22501,.T.);
#29775=ORIENTED_EDGE('',*,*,#22507,.T.);
#29776=ORIENTED_EDGE('',*,*,#22503,.T.);
#29777=ORIENTED_EDGE('',*,*,#22508,.F.);
#29778=ORIENTED_EDGE('',*,*,#22500,.T.);
#29779=ORIENTED_EDGE('',*,*,#22509,.T.);
#29780=ORIENTED_EDGE('',*,*,#22510,.T.);
#29781=ORIENTED_EDGE('',*,*,#22511,.T.);
#29782=ORIENTED_EDGE('',*,*,#22504,.F.);
#29783=ORIENTED_EDGE('',*,*,#22512,.F.);
#29784=ORIENTED_EDGE('',*,*,#22513,.F.);
#29785=ORIENTED_EDGE('',*,*,#22506,.F.);
#29786=ORIENTED_EDGE('',*,*,#22511,.F.);
#29787=ORIENTED_EDGE('',*,*,#22514,.F.);
#29788=ORIENTED_EDGE('',*,*,#22515,.F.);
#29789=ORIENTED_EDGE('',*,*,#22516,.F.);
#29790=ORIENTED_EDGE('',*,*,#22509,.F.);
#29791=ORIENTED_EDGE('',*,*,#22512,.T.);
#29792=ORIENTED_EDGE('',*,*,#22507,.F.);
#29793=ORIENTED_EDGE('',*,*,#22508,.T.);
#29794=ORIENTED_EDGE('',*,*,#22517,.T.);
#29795=ORIENTED_EDGE('',*,*,#22518,.T.);
#29796=ORIENTED_EDGE('',*,*,#22519,.T.);
#29797=ORIENTED_EDGE('',*,*,#22519,.F.);
#29798=ORIENTED_EDGE('',*,*,#22520,.F.);
#29799=ORIENTED_EDGE('',*,*,#22514,.T.);
#29800=ORIENTED_EDGE('',*,*,#22513,.T.);
#29801=ORIENTED_EDGE('',*,*,#22518,.F.);
#29802=ORIENTED_EDGE('',*,*,#22521,.F.);
#29803=ORIENTED_EDGE('',*,*,#22515,.T.);
#29804=ORIENTED_EDGE('',*,*,#22520,.T.);
#29805=ORIENTED_EDGE('',*,*,#22517,.F.);
#29806=ORIENTED_EDGE('',*,*,#22510,.F.);
#29807=ORIENTED_EDGE('',*,*,#22516,.T.);
#29808=ORIENTED_EDGE('',*,*,#22521,.T.);
#29809=ORIENTED_EDGE('',*,*,#22522,.F.);
#29810=ORIENTED_EDGE('',*,*,#22523,.T.);
#29811=ORIENTED_EDGE('',*,*,#22524,.T.);
#29812=ORIENTED_EDGE('',*,*,#22523,.F.);
#29813=ORIENTED_EDGE('',*,*,#22525,.T.);
#29814=ORIENTED_EDGE('',*,*,#22526,.T.);
#29815=ORIENTED_EDGE('',*,*,#22527,.T.);
#29816=ORIENTED_EDGE('',*,*,#22526,.F.);
#29817=ORIENTED_EDGE('',*,*,#22528,.T.);
#29818=ORIENTED_EDGE('',*,*,#22529,.T.);
#29819=ORIENTED_EDGE('',*,*,#22530,.F.);
#29820=ORIENTED_EDGE('',*,*,#22529,.F.);
#29821=ORIENTED_EDGE('',*,*,#22531,.F.);
#29822=ORIENTED_EDGE('',*,*,#22532,.F.);
#29823=ORIENTED_EDGE('',*,*,#22533,.T.);
#29824=ORIENTED_EDGE('',*,*,#22534,.F.);
#29825=ORIENTED_EDGE('',*,*,#22533,.F.);
#29826=ORIENTED_EDGE('',*,*,#22535,.F.);
#29827=ORIENTED_EDGE('',*,*,#22536,.F.);
#29828=ORIENTED_EDGE('',*,*,#22537,.T.);
#29829=ORIENTED_EDGE('',*,*,#22538,.F.);
#29830=ORIENTED_EDGE('',*,*,#22537,.F.);
#29831=ORIENTED_EDGE('',*,*,#22531,.T.);
#29832=ORIENTED_EDGE('',*,*,#22532,.T.);
#29833=ORIENTED_EDGE('',*,*,#22539,.T.);
#29834=ORIENTED_EDGE('',*,*,#22540,.T.);
#29835=ORIENTED_EDGE('',*,*,#22539,.F.);
#29836=ORIENTED_EDGE('',*,*,#22541,.F.);
#29837=ORIENTED_EDGE('',*,*,#22542,.T.);
#29838=ORIENTED_EDGE('',*,*,#22543,.T.);
#29839=ORIENTED_EDGE('',*,*,#22544,.F.);
#29840=ORIENTED_EDGE('',*,*,#22535,.T.);
#29841=ORIENTED_EDGE('',*,*,#22536,.T.);
#29842=ORIENTED_EDGE('',*,*,#22545,.T.);
#29843=ORIENTED_EDGE('',*,*,#22546,.T.);
#29844=ORIENTED_EDGE('',*,*,#22545,.F.);
#29845=ORIENTED_EDGE('',*,*,#22547,.T.);
#29846=ORIENTED_EDGE('',*,*,#22548,.T.);
#29847=ORIENTED_EDGE('',*,*,#22549,.F.);
#29848=ORIENTED_EDGE('',*,*,#22550,.F.);
#29849=ORIENTED_EDGE('',*,*,#22551,.T.);
#29850=ORIENTED_EDGE('',*,*,#22552,.T.);
#29851=ORIENTED_EDGE('',*,*,#22553,.F.);
#29852=ORIENTED_EDGE('',*,*,#22554,.T.);
#29853=ORIENTED_EDGE('',*,*,#22555,.T.);
#29854=ORIENTED_EDGE('',*,*,#22556,.F.);
#29855=ORIENTED_EDGE('',*,*,#22557,.F.);
#29856=ORIENTED_EDGE('',*,*,#22558,.F.);
#29857=ORIENTED_EDGE('',*,*,#22559,.T.);
#29858=ORIENTED_EDGE('',*,*,#22560,.F.);
#29859=ORIENTED_EDGE('',*,*,#22561,.T.);
#29860=ORIENTED_EDGE('',*,*,#22562,.F.);
#29861=ORIENTED_EDGE('',*,*,#22563,.T.);
#29862=ORIENTED_EDGE('',*,*,#22564,.F.);
#29863=ORIENTED_EDGE('',*,*,#22565,.T.);
#29864=ORIENTED_EDGE('',*,*,#22566,.F.);
#29865=ORIENTED_EDGE('',*,*,#22567,.T.);
#29866=ORIENTED_EDGE('',*,*,#22568,.F.);
#29867=ORIENTED_EDGE('',*,*,#22569,.T.);
#29868=ORIENTED_EDGE('',*,*,#22570,.F.);
#29869=ORIENTED_EDGE('',*,*,#22571,.F.);
#29870=ORIENTED_EDGE('',*,*,#22572,.T.);
#29871=ORIENTED_EDGE('',*,*,#22573,.T.);
#29872=ORIENTED_EDGE('',*,*,#22574,.F.);
#29873=ORIENTED_EDGE('',*,*,#22575,.F.);
#29874=ORIENTED_EDGE('',*,*,#22576,.T.);
#29875=ORIENTED_EDGE('',*,*,#22577,.T.);
#29876=ORIENTED_EDGE('',*,*,#22574,.T.);
#29877=ORIENTED_EDGE('',*,*,#22578,.F.);
#29878=ORIENTED_EDGE('',*,*,#22579,.F.);
#29879=ORIENTED_EDGE('',*,*,#22580,.T.);
#29880=ORIENTED_EDGE('',*,*,#22581,.T.);
#29881=ORIENTED_EDGE('',*,*,#22582,.F.);
#29882=ORIENTED_EDGE('',*,*,#22572,.F.);
#29883=ORIENTED_EDGE('',*,*,#22583,.F.);
#29884=ORIENTED_EDGE('',*,*,#22584,.T.);
#29885=ORIENTED_EDGE('',*,*,#22576,.F.);
#29886=ORIENTED_EDGE('',*,*,#22585,.T.);
#29887=ORIENTED_EDGE('',*,*,#22584,.F.);
#29888=ORIENTED_EDGE('',*,*,#22586,.F.);
#29889=ORIENTED_EDGE('',*,*,#22587,.F.);
#29890=ORIENTED_EDGE('',*,*,#22588,.F.);
#29891=ORIENTED_EDGE('',*,*,#22589,.T.);
#29892=ORIENTED_EDGE('',*,*,#22590,.T.);
#29893=ORIENTED_EDGE('',*,*,#22591,.T.);
#29894=ORIENTED_EDGE('',*,*,#22592,.F.);
#29895=ORIENTED_EDGE('',*,*,#22593,.F.);
#29896=ORIENTED_EDGE('',*,*,#22594,.T.);
#29897=ORIENTED_EDGE('',*,*,#22592,.T.);
#29898=ORIENTED_EDGE('',*,*,#22595,.F.);
#29899=ORIENTED_EDGE('',*,*,#22596,.T.);
#29900=ORIENTED_EDGE('',*,*,#22593,.T.);
#29901=ORIENTED_EDGE('',*,*,#22597,.T.);
#29902=ORIENTED_EDGE('',*,*,#22598,.F.);
#29903=ORIENTED_EDGE('',*,*,#22599,.F.);
#29904=ORIENTED_EDGE('',*,*,#22600,.F.);
#29905=ORIENTED_EDGE('',*,*,#22588,.T.);
#29906=ORIENTED_EDGE('',*,*,#22601,.T.);
#29907=ORIENTED_EDGE('',*,*,#22600,.T.);
#29908=ORIENTED_EDGE('',*,*,#22602,.F.);
#29909=ORIENTED_EDGE('',*,*,#22603,.F.);
#29910=ORIENTED_EDGE('',*,*,#22604,.T.);
#29911=ORIENTED_EDGE('',*,*,#22605,.T.);
#29912=ORIENTED_EDGE('',*,*,#22606,.F.);
#29913=ORIENTED_EDGE('',*,*,#22607,.T.);
#29914=ORIENTED_EDGE('',*,*,#22608,.T.);
#29915=ORIENTED_EDGE('',*,*,#22606,.T.);
#29916=ORIENTED_EDGE('',*,*,#22609,.F.);
#29917=ORIENTED_EDGE('',*,*,#22610,.F.);
#29918=ORIENTED_EDGE('',*,*,#22611,.F.);
#29919=ORIENTED_EDGE('',*,*,#22604,.F.);
#29920=ORIENTED_EDGE('',*,*,#22612,.T.);
#29921=ORIENTED_EDGE('',*,*,#22613,.T.);
#29922=ORIENTED_EDGE('',*,*,#22614,.F.);
#29923=ORIENTED_EDGE('',*,*,#22615,.T.);
#29924=ORIENTED_EDGE('',*,*,#22616,.F.);
#29925=ORIENTED_EDGE('',*,*,#22617,.F.);
#29926=ORIENTED_EDGE('',*,*,#22607,.F.);
#29927=ORIENTED_EDGE('',*,*,#22618,.T.);
#29928=ORIENTED_EDGE('',*,*,#22613,.F.);
#29929=ORIENTED_EDGE('',*,*,#22619,.F.);
#29930=ORIENTED_EDGE('',*,*,#22620,.F.);
#29931=ORIENTED_EDGE('',*,*,#22621,.T.);
#29932=ORIENTED_EDGE('',*,*,#22622,.F.);
#29933=ORIENTED_EDGE('',*,*,#22623,.F.);
#29934=ORIENTED_EDGE('',*,*,#22624,.T.);
#29935=ORIENTED_EDGE('',*,*,#22625,.T.);
#29936=ORIENTED_EDGE('',*,*,#22626,.F.);
#29937=ORIENTED_EDGE('',*,*,#22627,.F.);
#29938=ORIENTED_EDGE('',*,*,#22628,.T.);
#29939=ORIENTED_EDGE('',*,*,#22629,.T.);
#29940=ORIENTED_EDGE('',*,*,#22630,.T.);
#29941=ORIENTED_EDGE('',*,*,#22605,.F.);
#29942=ORIENTED_EDGE('',*,*,#22616,.T.);
#29943=ORIENTED_EDGE('',*,*,#22631,.F.);
#29944=ORIENTED_EDGE('',*,*,#22609,.T.);
#29945=ORIENTED_EDGE('',*,*,#22591,.F.);
#29946=ORIENTED_EDGE('',*,*,#22632,.T.);
#29947=ORIENTED_EDGE('',*,*,#22597,.F.);
#29948=ORIENTED_EDGE('',*,*,#22595,.T.);
#29949=ORIENTED_EDGE('',*,*,#22573,.F.);
#29950=ORIENTED_EDGE('',*,*,#22582,.T.);
#29951=ORIENTED_EDGE('',*,*,#22633,.F.);
#29952=ORIENTED_EDGE('',*,*,#22578,.T.);
#29953=ORIENTED_EDGE('',*,*,#22634,.T.);
#29954=ORIENTED_EDGE('',*,*,#22635,.T.);
#29955=ORIENTED_EDGE('',*,*,#22636,.T.);
#29956=ORIENTED_EDGE('',*,*,#22637,.T.);
#29957=ORIENTED_EDGE('',*,*,#22638,.T.);
#29958=ORIENTED_EDGE('',*,*,#22639,.T.);
#29959=ORIENTED_EDGE('',*,*,#22640,.T.);
#29960=ORIENTED_EDGE('',*,*,#22641,.T.);
#29961=ORIENTED_EDGE('',*,*,#22642,.T.);
#29962=ORIENTED_EDGE('',*,*,#22643,.F.);
#29963=ORIENTED_EDGE('',*,*,#22644,.F.);
#29964=ORIENTED_EDGE('',*,*,#22645,.F.);
#29965=ORIENTED_EDGE('',*,*,#22646,.T.);
#29966=ORIENTED_EDGE('',*,*,#22647,.T.);
#29967=ORIENTED_EDGE('',*,*,#22648,.F.);
#29968=ORIENTED_EDGE('',*,*,#22649,.F.);
#29969=ORIENTED_EDGE('',*,*,#22650,.T.);
#29970=ORIENTED_EDGE('',*,*,#22651,.T.);
#29971=ORIENTED_EDGE('',*,*,#22652,.F.);
#29972=ORIENTED_EDGE('',*,*,#22653,.T.);
#29973=ORIENTED_EDGE('',*,*,#22654,.F.);
#29974=ORIENTED_EDGE('',*,*,#22655,.T.);
#29975=ORIENTED_EDGE('',*,*,#22656,.T.);
#29976=ORIENTED_EDGE('',*,*,#22657,.F.);
#29977=ORIENTED_EDGE('',*,*,#22658,.T.);
#29978=ORIENTED_EDGE('',*,*,#22659,.T.);
#29979=ORIENTED_EDGE('',*,*,#22660,.T.);
#29980=ORIENTED_EDGE('',*,*,#22661,.T.);
#29981=ORIENTED_EDGE('',*,*,#22662,.T.);
#29982=ORIENTED_EDGE('',*,*,#22663,.T.);
#29983=ORIENTED_EDGE('',*,*,#22664,.F.);
#29984=ORIENTED_EDGE('',*,*,#22543,.F.);
#29985=ORIENTED_EDGE('',*,*,#22546,.F.);
#29986=ORIENTED_EDGE('',*,*,#22540,.F.);
#29987=ORIENTED_EDGE('',*,*,#22665,.F.);
#29988=ORIENTED_EDGE('',*,*,#22666,.F.);
#29989=ORIENTED_EDGE('',*,*,#22667,.T.);
#29990=ORIENTED_EDGE('',*,*,#22668,.T.);
#29991=ORIENTED_EDGE('',*,*,#22669,.T.);
#29992=ORIENTED_EDGE('',*,*,#22670,.F.);
#29993=ORIENTED_EDGE('',*,*,#22671,.F.);
#29994=ORIENTED_EDGE('',*,*,#22672,.T.);
#29995=ORIENTED_EDGE('',*,*,#22673,.F.);
#29996=ORIENTED_EDGE('',*,*,#22674,.F.);
#29997=ORIENTED_EDGE('',*,*,#22675,.T.);
#29998=ORIENTED_EDGE('',*,*,#22676,.T.);
#29999=ORIENTED_EDGE('',*,*,#22677,.F.);
#30000=ORIENTED_EDGE('',*,*,#22678,.T.);
#30001=ORIENTED_EDGE('',*,*,#22679,.T.);
#30002=ORIENTED_EDGE('',*,*,#22655,.F.);
#30003=ORIENTED_EDGE('',*,*,#22680,.F.);
#30004=ORIENTED_EDGE('',*,*,#22681,.F.);
#30005=ORIENTED_EDGE('',*,*,#22682,.F.);
#30006=ORIENTED_EDGE('',*,*,#22683,.T.);
#30007=ORIENTED_EDGE('',*,*,#22677,.T.);
#30008=ORIENTED_EDGE('',*,*,#22684,.T.);
#30009=ORIENTED_EDGE('',*,*,#22685,.F.);
#30010=ORIENTED_EDGE('',*,*,#22686,.T.);
#30011=ORIENTED_EDGE('',*,*,#22687,.T.);
#30012=ORIENTED_EDGE('',*,*,#22661,.F.);
#30013=ORIENTED_EDGE('',*,*,#22688,.F.);
#30014=ORIENTED_EDGE('',*,*,#22689,.F.);
#30015=ORIENTED_EDGE('',*,*,#22690,.F.);
#30016=ORIENTED_EDGE('',*,*,#22691,.T.);
#30017=ORIENTED_EDGE('',*,*,#22685,.T.);
#30018=ORIENTED_EDGE('',*,*,#22692,.T.);
#30019=ORIENTED_EDGE('',*,*,#22693,.F.);
#30020=ORIENTED_EDGE('',*,*,#22694,.T.);
#30021=ORIENTED_EDGE('',*,*,#22690,.T.);
#30022=ORIENTED_EDGE('',*,*,#22695,.F.);
#30023=ORIENTED_EDGE('',*,*,#22696,.T.);
#30024=ORIENTED_EDGE('',*,*,#22657,.T.);
#30025=ORIENTED_EDGE('',*,*,#22679,.F.);
#30026=ORIENTED_EDGE('',*,*,#22697,.T.);
#30027=ORIENTED_EDGE('',*,*,#22693,.T.);
#30028=ORIENTED_EDGE('',*,*,#22656,.F.);
#30029=ORIENTED_EDGE('',*,*,#22698,.F.);
#30030=ORIENTED_EDGE('',*,*,#22699,.T.);
#30031=ORIENTED_EDGE('',*,*,#22682,.T.);
#30032=ORIENTED_EDGE('',*,*,#22700,.F.);
#30033=ORIENTED_EDGE('',*,*,#22701,.T.);
#30034=ORIENTED_EDGE('',*,*,#22663,.F.);
#30035=ORIENTED_EDGE('',*,*,#22687,.F.);
#30036=ORIENTED_EDGE('',*,*,#22702,.T.);
#30037=ORIENTED_EDGE('',*,*,#22698,.T.);
#30038=ORIENTED_EDGE('',*,*,#22662,.F.);
#30039=ORIENTED_EDGE('',*,*,#22660,.F.);
#30040=ORIENTED_EDGE('',*,*,#22703,.F.);
#30041=ORIENTED_EDGE('',*,*,#22704,.T.);
#30042=ORIENTED_EDGE('',*,*,#22688,.T.);
#30043=ORIENTED_EDGE('',*,*,#22659,.F.);
#30044=ORIENTED_EDGE('',*,*,#22705,.F.);
#30045=ORIENTED_EDGE('',*,*,#22706,.T.);
#30046=ORIENTED_EDGE('',*,*,#22703,.T.);
#30047=ORIENTED_EDGE('',*,*,#22658,.F.);
#30048=ORIENTED_EDGE('',*,*,#22696,.F.);
#30049=ORIENTED_EDGE('',*,*,#22707,.T.);
#30050=ORIENTED_EDGE('',*,*,#22705,.T.);
#30051=ORIENTED_EDGE('',*,*,#22695,.T.);
#30052=ORIENTED_EDGE('',*,*,#22692,.F.);
#30053=ORIENTED_EDGE('',*,*,#22689,.T.);
#30054=ORIENTED_EDGE('',*,*,#22704,.F.);
#30055=ORIENTED_EDGE('',*,*,#22706,.F.);
#30056=ORIENTED_EDGE('',*,*,#22707,.F.);
#30057=ORIENTED_EDGE('',*,*,#22538,.T.);
#30058=ORIENTED_EDGE('',*,*,#22654,.T.);
#30059=ORIENTED_EDGE('',*,*,#22542,.F.);
#30060=ORIENTED_EDGE('',*,*,#22708,.F.);
#30061=ORIENTED_EDGE('',*,*,#22680,.T.);
#30062=ORIENTED_EDGE('',*,*,#22664,.T.);
#30063=ORIENTED_EDGE('',*,*,#22701,.F.);
#30064=ORIENTED_EDGE('',*,*,#22709,.F.);
#30065=ORIENTED_EDGE('',*,*,#22544,.T.);
#30066=ORIENTED_EDGE('',*,*,#22681,.T.);
#30067=ORIENTED_EDGE('',*,*,#22708,.T.);
#30068=ORIENTED_EDGE('',*,*,#22541,.T.);
#30069=ORIENTED_EDGE('',*,*,#22709,.T.);
#30070=ORIENTED_EDGE('',*,*,#22700,.T.);
#30071=ORIENTED_EDGE('',*,*,#22684,.F.);
#30072=ORIENTED_EDGE('',*,*,#22534,.T.);
#30073=ORIENTED_EDGE('',*,*,#22710,.F.);
#30074=ORIENTED_EDGE('',*,*,#22639,.F.);
#30075=ORIENTED_EDGE('',*,*,#22711,.F.);
#30076=ORIENTED_EDGE('',*,*,#22694,.F.);
#30077=ORIENTED_EDGE('',*,*,#22711,.T.);
#30078=ORIENTED_EDGE('',*,*,#22638,.F.);
#30079=ORIENTED_EDGE('',*,*,#22712,.F.);
#30080=ORIENTED_EDGE('',*,*,#22691,.F.);
#30081=ORIENTED_EDGE('',*,*,#22710,.T.);
#30082=ORIENTED_EDGE('',*,*,#22697,.F.);
#30083=ORIENTED_EDGE('',*,*,#22713,.F.);
#30084=ORIENTED_EDGE('',*,*,#22640,.F.);
#30085=ORIENTED_EDGE('',*,*,#22712,.T.);
#30086=ORIENTED_EDGE('',*,*,#22637,.F.);
#30087=ORIENTED_EDGE('',*,*,#22714,.F.);
#30088=ORIENTED_EDGE('',*,*,#22686,.F.);
#30089=ORIENTED_EDGE('',*,*,#22713,.T.);
#30090=ORIENTED_EDGE('',*,*,#22678,.F.);
#30091=ORIENTED_EDGE('',*,*,#22715,.F.);
#30092=ORIENTED_EDGE('',*,*,#22641,.F.);
#30093=ORIENTED_EDGE('',*,*,#22714,.T.);
#30094=ORIENTED_EDGE('',*,*,#22636,.F.);
#30095=ORIENTED_EDGE('',*,*,#22716,.F.);
#30096=ORIENTED_EDGE('',*,*,#22702,.F.);
#30097=ORIENTED_EDGE('',*,*,#22715,.T.);
#30098=ORIENTED_EDGE('',*,*,#22683,.F.);
#30099=ORIENTED_EDGE('',*,*,#22717,.F.);
#30100=ORIENTED_EDGE('',*,*,#22634,.F.);
#30101=ORIENTED_EDGE('',*,*,#22716,.T.);
#30102=ORIENTED_EDGE('',*,*,#22635,.F.);
#30103=ORIENTED_EDGE('',*,*,#22717,.T.);
#30104=ORIENTED_EDGE('',*,*,#22699,.F.);
#30105=ORIENTED_EDGE('',*,*,#22666,.T.);
#30106=ORIENTED_EDGE('',*,*,#22718,.F.);
#30107=ORIENTED_EDGE('',*,*,#22547,.F.);
#30108=ORIENTED_EDGE('',*,*,#22719,.T.);
#30109=ORIENTED_EDGE('',*,*,#22665,.T.);
#30110=ORIENTED_EDGE('',*,*,#22720,.F.);
#30111=ORIENTED_EDGE('',*,*,#22548,.F.);
#30112=ORIENTED_EDGE('',*,*,#22718,.T.);
#30113=ORIENTED_EDGE('',*,*,#22676,.F.);
#30114=ORIENTED_EDGE('',*,*,#22721,.F.);
#30115=ORIENTED_EDGE('',*,*,#22549,.T.);
#30116=ORIENTED_EDGE('',*,*,#22720,.T.);
#30117=ORIENTED_EDGE('',*,*,#22675,.F.);
#30118=ORIENTED_EDGE('',*,*,#22722,.F.);
#30119=ORIENTED_EDGE('',*,*,#22550,.T.);
#30120=ORIENTED_EDGE('',*,*,#22721,.T.);
#30121=ORIENTED_EDGE('',*,*,#22674,.T.);
#30122=ORIENTED_EDGE('',*,*,#22723,.F.);
#30123=ORIENTED_EDGE('',*,*,#22551,.F.);
#30124=ORIENTED_EDGE('',*,*,#22722,.T.);
#30125=ORIENTED_EDGE('',*,*,#22673,.T.);
#30126=ORIENTED_EDGE('',*,*,#22724,.F.);
#30127=ORIENTED_EDGE('',*,*,#22552,.F.);
#30128=ORIENTED_EDGE('',*,*,#22723,.T.);
#30129=ORIENTED_EDGE('',*,*,#22672,.F.);
#30130=ORIENTED_EDGE('',*,*,#22725,.F.);
#30131=ORIENTED_EDGE('',*,*,#22553,.T.);
#30132=ORIENTED_EDGE('',*,*,#22724,.T.);
#30133=ORIENTED_EDGE('',*,*,#22671,.T.);
#30134=ORIENTED_EDGE('',*,*,#22726,.F.);
#30135=ORIENTED_EDGE('',*,*,#22554,.F.);
#30136=ORIENTED_EDGE('',*,*,#22725,.T.);
#30137=ORIENTED_EDGE('',*,*,#22670,.T.);
#30138=ORIENTED_EDGE('',*,*,#22727,.F.);
#30139=ORIENTED_EDGE('',*,*,#22555,.F.);
#30140=ORIENTED_EDGE('',*,*,#22726,.T.);
#30141=ORIENTED_EDGE('',*,*,#22669,.F.);
#30142=ORIENTED_EDGE('',*,*,#22728,.F.);
#30143=ORIENTED_EDGE('',*,*,#22556,.T.);
#30144=ORIENTED_EDGE('',*,*,#22727,.T.);
#30145=ORIENTED_EDGE('',*,*,#22668,.F.);
#30146=ORIENTED_EDGE('',*,*,#22729,.F.);
#30147=ORIENTED_EDGE('',*,*,#22557,.T.);
#30148=ORIENTED_EDGE('',*,*,#22728,.T.);
#30149=ORIENTED_EDGE('',*,*,#22667,.F.);
#30150=ORIENTED_EDGE('',*,*,#22719,.F.);
#30151=ORIENTED_EDGE('',*,*,#22558,.T.);
#30152=ORIENTED_EDGE('',*,*,#22729,.T.);
#30153=ORIENTED_EDGE('',*,*,#22642,.F.);
#30154=ORIENTED_EDGE('',*,*,#22730,.F.);
#30155=ORIENTED_EDGE('',*,*,#22619,.T.);
#30156=ORIENTED_EDGE('',*,*,#22731,.T.);
#30157=ORIENTED_EDGE('',*,*,#22643,.T.);
#30158=ORIENTED_EDGE('',*,*,#22731,.F.);
#30159=ORIENTED_EDGE('',*,*,#22630,.F.);
#30160=ORIENTED_EDGE('',*,*,#22732,.T.);
#30161=ORIENTED_EDGE('',*,*,#22644,.T.);
#30162=ORIENTED_EDGE('',*,*,#22732,.F.);
#30163=ORIENTED_EDGE('',*,*,#22629,.F.);
#30164=ORIENTED_EDGE('',*,*,#22733,.T.);
#30165=ORIENTED_EDGE('',*,*,#22645,.T.);
#30166=ORIENTED_EDGE('',*,*,#22733,.F.);
#30167=ORIENTED_EDGE('',*,*,#22628,.F.);
#30168=ORIENTED_EDGE('',*,*,#22734,.T.);
#30169=ORIENTED_EDGE('',*,*,#22646,.F.);
#30170=ORIENTED_EDGE('',*,*,#22734,.F.);
#30171=ORIENTED_EDGE('',*,*,#22627,.T.);
#30172=ORIENTED_EDGE('',*,*,#22735,.T.);
#30173=ORIENTED_EDGE('',*,*,#22647,.F.);
#30174=ORIENTED_EDGE('',*,*,#22735,.F.);
#30175=ORIENTED_EDGE('',*,*,#22626,.T.);
#30176=ORIENTED_EDGE('',*,*,#22736,.T.);
#30177=ORIENTED_EDGE('',*,*,#22648,.T.);
#30178=ORIENTED_EDGE('',*,*,#22736,.F.);
#30179=ORIENTED_EDGE('',*,*,#22625,.F.);
#30180=ORIENTED_EDGE('',*,*,#22737,.T.);
#30181=ORIENTED_EDGE('',*,*,#22649,.T.);
#30182=ORIENTED_EDGE('',*,*,#22737,.F.);
#30183=ORIENTED_EDGE('',*,*,#22624,.F.);
#30184=ORIENTED_EDGE('',*,*,#22738,.T.);
#30185=ORIENTED_EDGE('',*,*,#22650,.F.);
#30186=ORIENTED_EDGE('',*,*,#22738,.F.);
#30187=ORIENTED_EDGE('',*,*,#22623,.T.);
#30188=ORIENTED_EDGE('',*,*,#22739,.T.);
#30189=ORIENTED_EDGE('',*,*,#22651,.F.);
#30190=ORIENTED_EDGE('',*,*,#22739,.F.);
#30191=ORIENTED_EDGE('',*,*,#22622,.T.);
#30192=ORIENTED_EDGE('',*,*,#22740,.T.);
#30193=ORIENTED_EDGE('',*,*,#22652,.T.);
#30194=ORIENTED_EDGE('',*,*,#22740,.F.);
#30195=ORIENTED_EDGE('',*,*,#22621,.F.);
#30196=ORIENTED_EDGE('',*,*,#22741,.T.);
#30197=ORIENTED_EDGE('',*,*,#22653,.F.);
#30198=ORIENTED_EDGE('',*,*,#22741,.F.);
#30199=ORIENTED_EDGE('',*,*,#22620,.T.);
#30200=ORIENTED_EDGE('',*,*,#22730,.T.);
#30201=ORIENTED_EDGE('',*,*,#22581,.F.);
#30202=ORIENTED_EDGE('',*,*,#22742,.T.);
#30203=ORIENTED_EDGE('',*,*,#22579,.T.);
#30204=ORIENTED_EDGE('',*,*,#22633,.T.);
#30205=ORIENTED_EDGE('',*,*,#22615,.F.);
#30206=ORIENTED_EDGE('',*,*,#22743,.T.);
#30207=ORIENTED_EDGE('',*,*,#22610,.T.);
#30208=ORIENTED_EDGE('',*,*,#22631,.T.);
#30209=ORIENTED_EDGE('',*,*,#22744,.F.);
#30210=ORIENTED_EDGE('',*,*,#22598,.T.);
#30211=ORIENTED_EDGE('',*,*,#22632,.F.);
#30212=ORIENTED_EDGE('',*,*,#22590,.F.);
#30213=ORIENTED_EDGE('',*,*,#22614,.T.);
#30214=ORIENTED_EDGE('',*,*,#22618,.F.);
#30215=ORIENTED_EDGE('',*,*,#22611,.T.);
#30216=ORIENTED_EDGE('',*,*,#22743,.F.);
#30217=ORIENTED_EDGE('',*,*,#22603,.T.);
#30218=ORIENTED_EDGE('',*,*,#22608,.F.);
#30219=ORIENTED_EDGE('',*,*,#22617,.T.);
#30220=ORIENTED_EDGE('',*,*,#22612,.F.);
#30221=ORIENTED_EDGE('',*,*,#22744,.T.);
#30222=ORIENTED_EDGE('',*,*,#22589,.F.);
#30223=ORIENTED_EDGE('',*,*,#22602,.T.);
#30224=ORIENTED_EDGE('',*,*,#22599,.T.);
#30225=ORIENTED_EDGE('',*,*,#22596,.F.);
#30226=ORIENTED_EDGE('',*,*,#22601,.F.);
#30227=ORIENTED_EDGE('',*,*,#22587,.T.);
#30228=ORIENTED_EDGE('',*,*,#22594,.F.);
#30229=ORIENTED_EDGE('',*,*,#22571,.T.);
#30230=ORIENTED_EDGE('',*,*,#22577,.F.);
#30231=ORIENTED_EDGE('',*,*,#22586,.T.);
#30232=ORIENTED_EDGE('',*,*,#22583,.T.);
#30233=ORIENTED_EDGE('',*,*,#22580,.F.);
#30234=ORIENTED_EDGE('',*,*,#22585,.F.);
#30235=ORIENTED_EDGE('',*,*,#22575,.T.);
#30236=ORIENTED_EDGE('',*,*,#22742,.F.);
#30237=ORIENTED_EDGE('',*,*,#22745,.T.);
#30238=ORIENTED_EDGE('',*,*,#22746,.F.);
#30239=ORIENTED_EDGE('',*,*,#22747,.T.);
#30240=ORIENTED_EDGE('',*,*,#22748,.F.);
#30241=ORIENTED_EDGE('',*,*,#22749,.T.);
#30242=ORIENTED_EDGE('',*,*,#22750,.T.);
#30243=ORIENTED_EDGE('',*,*,#22751,.T.);
#30244=ORIENTED_EDGE('',*,*,#22752,.F.);
#30245=ORIENTED_EDGE('',*,*,#22560,.T.);
#30246=ORIENTED_EDGE('',*,*,#22753,.F.);
#30247=ORIENTED_EDGE('',*,*,#22745,.F.);
#30248=ORIENTED_EDGE('',*,*,#22754,.T.);
#30249=ORIENTED_EDGE('',*,*,#22559,.F.);
#30250=ORIENTED_EDGE('',*,*,#22755,.F.);
#30251=ORIENTED_EDGE('',*,*,#22746,.T.);
#30252=ORIENTED_EDGE('',*,*,#22753,.T.);
#30253=ORIENTED_EDGE('',*,*,#22562,.T.);
#30254=ORIENTED_EDGE('',*,*,#22756,.F.);
#30255=ORIENTED_EDGE('',*,*,#22747,.F.);
#30256=ORIENTED_EDGE('',*,*,#22755,.T.);
#30257=ORIENTED_EDGE('',*,*,#22561,.F.);
#30258=ORIENTED_EDGE('',*,*,#22754,.F.);
#30259=ORIENTED_EDGE('',*,*,#22748,.T.);
#30260=ORIENTED_EDGE('',*,*,#22756,.T.);
#30261=ORIENTED_EDGE('',*,*,#22757,.T.);
#30262=ORIENTED_EDGE('',*,*,#22758,.T.);
#30263=ORIENTED_EDGE('',*,*,#22759,.F.);
#30264=ORIENTED_EDGE('',*,*,#22760,.T.);
#30265=ORIENTED_EDGE('',*,*,#22761,.F.);
#30266=ORIENTED_EDGE('',*,*,#22762,.T.);
#30267=ORIENTED_EDGE('',*,*,#22763,.T.);
#30268=ORIENTED_EDGE('',*,*,#22760,.F.);
#30269=ORIENTED_EDGE('',*,*,#22764,.F.);
#30270=ORIENTED_EDGE('',*,*,#22762,.F.);
#30271=ORIENTED_EDGE('',*,*,#22765,.T.);
#30272=ORIENTED_EDGE('',*,*,#22766,.F.);
#30273=ORIENTED_EDGE('',*,*,#22751,.F.);
#30274=ORIENTED_EDGE('',*,*,#22767,.F.);
#30275=ORIENTED_EDGE('',*,*,#22766,.T.);
#30276=ORIENTED_EDGE('',*,*,#22768,.T.);
#30277=ORIENTED_EDGE('',*,*,#22769,.T.);
#30278=ORIENTED_EDGE('',*,*,#22752,.T.);
#30279=ORIENTED_EDGE('',*,*,#22768,.F.);
#30280=ORIENTED_EDGE('',*,*,#22765,.F.);
#30281=ORIENTED_EDGE('',*,*,#22761,.T.);
#30282=ORIENTED_EDGE('',*,*,#22759,.T.);
#30283=ORIENTED_EDGE('',*,*,#22530,.T.);
#30284=ORIENTED_EDGE('',*,*,#22749,.F.);
#30285=ORIENTED_EDGE('',*,*,#22769,.F.);
#30286=ORIENTED_EDGE('',*,*,#22758,.F.);
#30287=ORIENTED_EDGE('',*,*,#22770,.T.);
#30288=ORIENTED_EDGE('',*,*,#22750,.F.);
#30289=ORIENTED_EDGE('',*,*,#22770,.F.);
#30290=ORIENTED_EDGE('',*,*,#22757,.F.);
#30291=ORIENTED_EDGE('',*,*,#22763,.F.);
#30292=ORIENTED_EDGE('',*,*,#22764,.T.);
#30293=ORIENTED_EDGE('',*,*,#22767,.T.);
#30294=ORIENTED_EDGE('',*,*,#22528,.F.);
#30295=ORIENTED_EDGE('',*,*,#22567,.F.);
#30296=ORIENTED_EDGE('',*,*,#22771,.F.);
#30297=ORIENTED_EDGE('',*,*,#22772,.T.);
#30298=ORIENTED_EDGE('',*,*,#22773,.T.);
#30299=ORIENTED_EDGE('',*,*,#22570,.T.);
#30300=ORIENTED_EDGE('',*,*,#22774,.F.);
#30301=ORIENTED_EDGE('',*,*,#22775,.F.);
#30302=ORIENTED_EDGE('',*,*,#22771,.T.);
#30303=ORIENTED_EDGE('',*,*,#22569,.F.);
#30304=ORIENTED_EDGE('',*,*,#22776,.F.);
#30305=ORIENTED_EDGE('',*,*,#22777,.T.);
#30306=ORIENTED_EDGE('',*,*,#22774,.T.);
#30307=ORIENTED_EDGE('',*,*,#22568,.T.);
#30308=ORIENTED_EDGE('',*,*,#22773,.F.);
#30309=ORIENTED_EDGE('',*,*,#22778,.F.);
#30310=ORIENTED_EDGE('',*,*,#22776,.T.);
#30311=ORIENTED_EDGE('',*,*,#22772,.F.);
#30312=ORIENTED_EDGE('',*,*,#22775,.T.);
#30313=ORIENTED_EDGE('',*,*,#22777,.F.);
#30314=ORIENTED_EDGE('',*,*,#22778,.T.);
#30315=ORIENTED_EDGE('',*,*,#22779,.F.);
#30316=ORIENTED_EDGE('',*,*,#22780,.T.);
#30317=ORIENTED_EDGE('',*,*,#22781,.T.);
#30318=ORIENTED_EDGE('',*,*,#22782,.T.);
#30319=ORIENTED_EDGE('',*,*,#22783,.T.);
#30320=ORIENTED_EDGE('',*,*,#22784,.T.);
#30321=ORIENTED_EDGE('',*,*,#22785,.F.);
#30322=ORIENTED_EDGE('',*,*,#22786,.F.);
#30323=ORIENTED_EDGE('',*,*,#22787,.F.);
#30324=ORIENTED_EDGE('',*,*,#22786,.T.);
#30325=ORIENTED_EDGE('',*,*,#22788,.F.);
#30326=ORIENTED_EDGE('',*,*,#22789,.F.);
#30327=ORIENTED_EDGE('',*,*,#22790,.T.);
#30328=ORIENTED_EDGE('',*,*,#22791,.T.);
#30329=ORIENTED_EDGE('',*,*,#22784,.F.);
#30330=ORIENTED_EDGE('',*,*,#22792,.T.);
#30331=ORIENTED_EDGE('',*,*,#22782,.F.);
#30332=ORIENTED_EDGE('',*,*,#22793,.F.);
#30333=ORIENTED_EDGE('',*,*,#22790,.F.);
#30334=ORIENTED_EDGE('',*,*,#22794,.T.);
#30335=ORIENTED_EDGE('',*,*,#22780,.F.);
#30336=ORIENTED_EDGE('',*,*,#22795,.F.);
#30337=ORIENTED_EDGE('',*,*,#22789,.T.);
#30338=ORIENTED_EDGE('',*,*,#22796,.T.);
#30339=ORIENTED_EDGE('',*,*,#22781,.F.);
#30340=ORIENTED_EDGE('',*,*,#22796,.F.);
#30341=ORIENTED_EDGE('',*,*,#22788,.T.);
#30342=ORIENTED_EDGE('',*,*,#22785,.T.);
#30343=ORIENTED_EDGE('',*,*,#22791,.F.);
#30344=ORIENTED_EDGE('',*,*,#22793,.T.);
#30345=ORIENTED_EDGE('',*,*,#22525,.F.);
#30346=ORIENTED_EDGE('',*,*,#22795,.T.);
#30347=ORIENTED_EDGE('',*,*,#22779,.T.);
#30348=ORIENTED_EDGE('',*,*,#22794,.F.);
#30349=ORIENTED_EDGE('',*,*,#22792,.F.);
#30350=ORIENTED_EDGE('',*,*,#22783,.F.);
#30351=ORIENTED_EDGE('',*,*,#22787,.T.);
#30352=ORIENTED_EDGE('',*,*,#22527,.F.);
#30353=ORIENTED_EDGE('',*,*,#22797,.F.);
#30354=ORIENTED_EDGE('',*,*,#22798,.T.);
#30355=ORIENTED_EDGE('',*,*,#22799,.F.);
#30356=ORIENTED_EDGE('',*,*,#22800,.T.);
#30357=ORIENTED_EDGE('',*,*,#22801,.F.);
#30358=ORIENTED_EDGE('',*,*,#22802,.T.);
#30359=ORIENTED_EDGE('',*,*,#22803,.T.);
#30360=ORIENTED_EDGE('',*,*,#22804,.T.);
#30361=ORIENTED_EDGE('',*,*,#22563,.F.);
#30362=ORIENTED_EDGE('',*,*,#22805,.F.);
#30363=ORIENTED_EDGE('',*,*,#22797,.T.);
#30364=ORIENTED_EDGE('',*,*,#22806,.T.);
#30365=ORIENTED_EDGE('',*,*,#22566,.T.);
#30366=ORIENTED_EDGE('',*,*,#22807,.F.);
#30367=ORIENTED_EDGE('',*,*,#22798,.F.);
#30368=ORIENTED_EDGE('',*,*,#22805,.T.);
#30369=ORIENTED_EDGE('',*,*,#22565,.F.);
#30370=ORIENTED_EDGE('',*,*,#22808,.F.);
#30371=ORIENTED_EDGE('',*,*,#22799,.T.);
#30372=ORIENTED_EDGE('',*,*,#22807,.T.);
#30373=ORIENTED_EDGE('',*,*,#22564,.T.);
#30374=ORIENTED_EDGE('',*,*,#22806,.F.);
#30375=ORIENTED_EDGE('',*,*,#22800,.F.);
#30376=ORIENTED_EDGE('',*,*,#22808,.T.);
#30377=ORIENTED_EDGE('',*,*,#22809,.F.);
#30378=ORIENTED_EDGE('',*,*,#22810,.T.);
#30379=ORIENTED_EDGE('',*,*,#22811,.T.);
#30380=ORIENTED_EDGE('',*,*,#22812,.F.);
#30381=ORIENTED_EDGE('',*,*,#22813,.T.);
#30382=ORIENTED_EDGE('',*,*,#22814,.F.);
#30383=ORIENTED_EDGE('',*,*,#22811,.F.);
#30384=ORIENTED_EDGE('',*,*,#22815,.T.);
#30385=ORIENTED_EDGE('',*,*,#22816,.T.);
#30386=ORIENTED_EDGE('',*,*,#22817,.F.);
#30387=ORIENTED_EDGE('',*,*,#22818,.F.);
#30388=ORIENTED_EDGE('',*,*,#22809,.T.);
#30389=ORIENTED_EDGE('',*,*,#22804,.F.);
#30390=ORIENTED_EDGE('',*,*,#22819,.F.);
#30391=ORIENTED_EDGE('',*,*,#22817,.T.);
#30392=ORIENTED_EDGE('',*,*,#22820,.T.);
#30393=ORIENTED_EDGE('',*,*,#22802,.F.);
#30394=ORIENTED_EDGE('',*,*,#22821,.F.);
#30395=ORIENTED_EDGE('',*,*,#22813,.F.);
#30396=ORIENTED_EDGE('',*,*,#22822,.T.);
#30397=ORIENTED_EDGE('',*,*,#22803,.F.);
#30398=ORIENTED_EDGE('',*,*,#22822,.F.);
#30399=ORIENTED_EDGE('',*,*,#22815,.F.);
#30400=ORIENTED_EDGE('',*,*,#22810,.F.);
#30401=ORIENTED_EDGE('',*,*,#22818,.T.);
#30402=ORIENTED_EDGE('',*,*,#22819,.T.);
#30403=ORIENTED_EDGE('',*,*,#22522,.T.);
#30404=ORIENTED_EDGE('',*,*,#22821,.T.);
#30405=ORIENTED_EDGE('',*,*,#22801,.T.);
#30406=ORIENTED_EDGE('',*,*,#22820,.F.);
#30407=ORIENTED_EDGE('',*,*,#22816,.F.);
#30408=ORIENTED_EDGE('',*,*,#22812,.T.);
#30409=ORIENTED_EDGE('',*,*,#22814,.T.);
#30410=ORIENTED_EDGE('',*,*,#22524,.F.);
#30411=ORIENTED_EDGE('',*,*,#22823,.F.);
#30412=ORIENTED_EDGE('',*,*,#22824,.F.);
#30413=ORIENTED_EDGE('',*,*,#22825,.F.);
#30414=ORIENTED_EDGE('',*,*,#22826,.F.);
#30415=ORIENTED_EDGE('',*,*,#22827,.T.);
#30416=ORIENTED_EDGE('',*,*,#22828,.T.);
#30417=ORIENTED_EDGE('',*,*,#22829,.T.);
#30418=ORIENTED_EDGE('',*,*,#22830,.T.);
#30419=ORIENTED_EDGE('',*,*,#22826,.T.);
#30420=ORIENTED_EDGE('',*,*,#22831,.F.);
#30421=ORIENTED_EDGE('',*,*,#22827,.F.);
#30422=ORIENTED_EDGE('',*,*,#22832,.T.);
#30423=ORIENTED_EDGE('',*,*,#22823,.T.);
#30424=ORIENTED_EDGE('',*,*,#22832,.F.);
#30425=ORIENTED_EDGE('',*,*,#22830,.F.);
#30426=ORIENTED_EDGE('',*,*,#22833,.T.);
#30427=ORIENTED_EDGE('',*,*,#22824,.T.);
#30428=ORIENTED_EDGE('',*,*,#22833,.F.);
#30429=ORIENTED_EDGE('',*,*,#22829,.F.);
#30430=ORIENTED_EDGE('',*,*,#22834,.T.);
#30431=ORIENTED_EDGE('',*,*,#22825,.T.);
#30432=ORIENTED_EDGE('',*,*,#22834,.F.);
#30433=ORIENTED_EDGE('',*,*,#22828,.F.);
#30434=ORIENTED_EDGE('',*,*,#22831,.T.);
#30435=ORIENTED_EDGE('',*,*,#22835,.F.);
#30436=ORIENTED_EDGE('',*,*,#22836,.T.);
#30437=ORIENTED_EDGE('',*,*,#22837,.T.);
#30438=ORIENTED_EDGE('',*,*,#22836,.F.);
#30439=ORIENTED_EDGE('',*,*,#22838,.F.);
#30440=ORIENTED_EDGE('',*,*,#22839,.T.);
#30441=ORIENTED_EDGE('',*,*,#22840,.T.);
#30442=ORIENTED_EDGE('',*,*,#22839,.F.);
#30443=ORIENTED_EDGE('',*,*,#22841,.F.);
#30444=ORIENTED_EDGE('',*,*,#22842,.T.);
#30445=ORIENTED_EDGE('',*,*,#22843,.T.);
#30446=ORIENTED_EDGE('',*,*,#22844,.T.);
#30447=ORIENTED_EDGE('',*,*,#22845,.F.);
#30448=ORIENTED_EDGE('',*,*,#22846,.F.);
#30449=ORIENTED_EDGE('',*,*,#22847,.T.);
#30450=ORIENTED_EDGE('',*,*,#22848,.T.);
#30451=ORIENTED_EDGE('',*,*,#22849,.T.);
#30452=ORIENTED_EDGE('',*,*,#22850,.T.);
#30453=ORIENTED_EDGE('',*,*,#22851,.F.);
#30454=ORIENTED_EDGE('',*,*,#22852,.F.);
#30455=ORIENTED_EDGE('',*,*,#22853,.T.);
#30456=ORIENTED_EDGE('',*,*,#22845,.T.);
#30457=ORIENTED_EDGE('',*,*,#22854,.T.);
#30458=ORIENTED_EDGE('',*,*,#22855,.F.);
#30459=ORIENTED_EDGE('',*,*,#22856,.F.);
#30460=ORIENTED_EDGE('',*,*,#22857,.F.);
#30461=ORIENTED_EDGE('',*,*,#22850,.F.);
#30462=ORIENTED_EDGE('',*,*,#22858,.F.);
#30463=ORIENTED_EDGE('',*,*,#22859,.T.);
#30464=ORIENTED_EDGE('',*,*,#22860,.T.);
#30465=ORIENTED_EDGE('',*,*,#22861,.T.);
#30466=ORIENTED_EDGE('',*,*,#22862,.F.);
#30467=ORIENTED_EDGE('',*,*,#22863,.T.);
#30468=ORIENTED_EDGE('',*,*,#22864,.T.);
#30469=ORIENTED_EDGE('',*,*,#22865,.F.);
#30470=ORIENTED_EDGE('',*,*,#22866,.F.);
#30471=ORIENTED_EDGE('',*,*,#22867,.F.);
#30472=ORIENTED_EDGE('',*,*,#22868,.F.);
#30473=ORIENTED_EDGE('',*,*,#22869,.T.);
#30474=ORIENTED_EDGE('',*,*,#22870,.T.);
#30475=ORIENTED_EDGE('',*,*,#22864,.F.);
#30476=ORIENTED_EDGE('',*,*,#22871,.F.);
#30477=ORIENTED_EDGE('',*,*,#22872,.T.);
#30478=ORIENTED_EDGE('',*,*,#22873,.T.);
#30479=ORIENTED_EDGE('',*,*,#22874,.T.);
#30480=ORIENTED_EDGE('',*,*,#22875,.F.);
#30481=ORIENTED_EDGE('',*,*,#22876,.T.);
#30482=ORIENTED_EDGE('',*,*,#22867,.T.);
#30483=ORIENTED_EDGE('',*,*,#22877,.T.);
#30484=ORIENTED_EDGE('',*,*,#22878,.F.);
#30485=ORIENTED_EDGE('',*,*,#22879,.F.);
#30486=ORIENTED_EDGE('',*,*,#22880,.F.);
#30487=ORIENTED_EDGE('',*,*,#22881,.T.);
#30488=ORIENTED_EDGE('',*,*,#22882,.T.);
#30489=ORIENTED_EDGE('',*,*,#22883,.T.);
#30490=ORIENTED_EDGE('',*,*,#22884,.T.);
#30491=ORIENTED_EDGE('',*,*,#22885,.F.);
#30492=ORIENTED_EDGE('',*,*,#22886,.F.);
#30493=ORIENTED_EDGE('',*,*,#22854,.F.);
#30494=ORIENTED_EDGE('',*,*,#22848,.F.);
#30495=ORIENTED_EDGE('',*,*,#22887,.T.);
#30496=ORIENTED_EDGE('',*,*,#22851,.T.);
#30497=ORIENTED_EDGE('',*,*,#22862,.T.);
#30498=ORIENTED_EDGE('',*,*,#22888,.T.);
#30499=ORIENTED_EDGE('',*,*,#22889,.F.);
#30500=ORIENTED_EDGE('',*,*,#22890,.F.);
#30501=ORIENTED_EDGE('',*,*,#22877,.F.);
#30502=ORIENTED_EDGE('',*,*,#22870,.F.);
#30503=ORIENTED_EDGE('',*,*,#22891,.T.);
#30504=ORIENTED_EDGE('',*,*,#22865,.T.);
#30505=ORIENTED_EDGE('',*,*,#22875,.T.);
#30506=ORIENTED_EDGE('',*,*,#22892,.T.);
#30507=ORIENTED_EDGE('',*,*,#22893,.T.);
#30508=ORIENTED_EDGE('',*,*,#22894,.F.);
#30509=ORIENTED_EDGE('',*,*,#22895,.F.);
#30510=ORIENTED_EDGE('',*,*,#22896,.T.);
#30511=ORIENTED_EDGE('',*,*,#22897,.F.);
#30512=ORIENTED_EDGE('',*,*,#22898,.F.);
#30513=ORIENTED_EDGE('',*,*,#22899,.F.);
#30514=ORIENTED_EDGE('',*,*,#22900,.F.);
#30515=ORIENTED_EDGE('',*,*,#22901,.T.);
#30516=ORIENTED_EDGE('',*,*,#22902,.T.);
#30517=ORIENTED_EDGE('',*,*,#22903,.F.);
#30518=ORIENTED_EDGE('',*,*,#22904,.F.);
#30519=ORIENTED_EDGE('',*,*,#22905,.F.);
#30520=ORIENTED_EDGE('',*,*,#22906,.T.);
#30521=ORIENTED_EDGE('',*,*,#22895,.T.);
#30522=ORIENTED_EDGE('',*,*,#22907,.F.);
#30523=ORIENTED_EDGE('',*,*,#22908,.F.);
#30524=ORIENTED_EDGE('',*,*,#22909,.T.);
#30525=ORIENTED_EDGE('',*,*,#22894,.T.);
#30526=ORIENTED_EDGE('',*,*,#22910,.F.);
#30527=ORIENTED_EDGE('',*,*,#22911,.F.);
#30528=ORIENTED_EDGE('',*,*,#22907,.T.);
#30529=ORIENTED_EDGE('',*,*,#22893,.F.);
#30530=ORIENTED_EDGE('',*,*,#22912,.F.);
#30531=ORIENTED_EDGE('',*,*,#22913,.T.);
#30532=ORIENTED_EDGE('',*,*,#22910,.T.);
#30533=ORIENTED_EDGE('',*,*,#22896,.F.);
#30534=ORIENTED_EDGE('',*,*,#22909,.F.);
#30535=ORIENTED_EDGE('',*,*,#22914,.T.);
#30536=ORIENTED_EDGE('',*,*,#22912,.T.);
#30537=ORIENTED_EDGE('',*,*,#22908,.T.);
#30538=ORIENTED_EDGE('',*,*,#22911,.T.);
#30539=ORIENTED_EDGE('',*,*,#22913,.F.);
#30540=ORIENTED_EDGE('',*,*,#22914,.F.);
#30541=ORIENTED_EDGE('',*,*,#22915,.F.);
#30542=ORIENTED_EDGE('',*,*,#22916,.F.);
#30543=ORIENTED_EDGE('',*,*,#22917,.F.);
#30544=ORIENTED_EDGE('',*,*,#22918,.F.);
#30545=ORIENTED_EDGE('',*,*,#22905,.T.);
#30546=ORIENTED_EDGE('',*,*,#22919,.F.);
#30547=ORIENTED_EDGE('',*,*,#22920,.F.);
#30548=ORIENTED_EDGE('',*,*,#22904,.T.);
#30549=ORIENTED_EDGE('',*,*,#22921,.T.);
#30550=ORIENTED_EDGE('',*,*,#22922,.T.);
#30551=ORIENTED_EDGE('',*,*,#22923,.T.);
#30552=ORIENTED_EDGE('',*,*,#22903,.T.);
#30553=ORIENTED_EDGE('',*,*,#22924,.T.);
#30554=ORIENTED_EDGE('',*,*,#22925,.T.);
#30555=ORIENTED_EDGE('',*,*,#22926,.F.);
#30556=ORIENTED_EDGE('',*,*,#22881,.F.);
#30557=ORIENTED_EDGE('',*,*,#22927,.T.);
#30558=ORIENTED_EDGE('',*,*,#22928,.F.);
#30559=ORIENTED_EDGE('',*,*,#22929,.F.);
#30560=ORIENTED_EDGE('',*,*,#22906,.F.);
#30561=ORIENTED_EDGE('',*,*,#22930,.F.);
#30562=ORIENTED_EDGE('',*,*,#22931,.F.);
#30563=ORIENTED_EDGE('',*,*,#22932,.T.);
#30564=ORIENTED_EDGE('',*,*,#22926,.T.);
#30565=ORIENTED_EDGE('',*,*,#22933,.F.);
#30566=ORIENTED_EDGE('',*,*,#22934,.F.);
#30567=ORIENTED_EDGE('',*,*,#22882,.F.);
#30568=ORIENTED_EDGE('',*,*,#22900,.T.);
#30569=ORIENTED_EDGE('',*,*,#22935,.F.);
#30570=ORIENTED_EDGE('',*,*,#22936,.F.);
#30571=ORIENTED_EDGE('',*,*,#22899,.T.);
#30572=ORIENTED_EDGE('',*,*,#22937,.T.);
#30573=ORIENTED_EDGE('',*,*,#22938,.T.);
#30574=ORIENTED_EDGE('',*,*,#22939,.T.);
#30575=ORIENTED_EDGE('',*,*,#22898,.T.);
#30576=ORIENTED_EDGE('',*,*,#22940,.T.);
#30577=ORIENTED_EDGE('',*,*,#22941,.T.);
#30578=ORIENTED_EDGE('',*,*,#22942,.F.);
#30579=ORIENTED_EDGE('',*,*,#22883,.F.);
#30580=ORIENTED_EDGE('',*,*,#22934,.T.);
#30581=ORIENTED_EDGE('',*,*,#22943,.F.);
#30582=ORIENTED_EDGE('',*,*,#22944,.F.);
#30583=ORIENTED_EDGE('',*,*,#22901,.F.);
#30584=ORIENTED_EDGE('',*,*,#22945,.F.);
#30585=ORIENTED_EDGE('',*,*,#22946,.F.);
#30586=ORIENTED_EDGE('',*,*,#22947,.T.);
#30587=ORIENTED_EDGE('',*,*,#22942,.T.);
#30588=ORIENTED_EDGE('',*,*,#22948,.T.);
#30589=ORIENTED_EDGE('',*,*,#22927,.F.);
#30590=ORIENTED_EDGE('',*,*,#22884,.F.);
#30591=ORIENTED_EDGE('',*,*,#22887,.F.);
#30592=ORIENTED_EDGE('',*,*,#22847,.F.);
#30593=ORIENTED_EDGE('',*,*,#22949,.T.);
#30594=ORIENTED_EDGE('',*,*,#22852,.T.);
#30595=ORIENTED_EDGE('',*,*,#22950,.F.);
#30596=ORIENTED_EDGE('',*,*,#22855,.T.);
#30597=ORIENTED_EDGE('',*,*,#22886,.T.);
#30598=ORIENTED_EDGE('',*,*,#22951,.F.);
#30599=ORIENTED_EDGE('',*,*,#22861,.F.);
#30600=ORIENTED_EDGE('',*,*,#22952,.T.);
#30601=ORIENTED_EDGE('',*,*,#22953,.T.);
#30602=ORIENTED_EDGE('',*,*,#22888,.F.);
#30603=ORIENTED_EDGE('',*,*,#22949,.F.);
#30604=ORIENTED_EDGE('',*,*,#22846,.T.);
#30605=ORIENTED_EDGE('',*,*,#22954,.T.);
#30606=ORIENTED_EDGE('',*,*,#22955,.F.);
#30607=ORIENTED_EDGE('',*,*,#22956,.F.);
#30608=ORIENTED_EDGE('',*,*,#22950,.T.);
#30609=ORIENTED_EDGE('',*,*,#22957,.T.);
#30610=ORIENTED_EDGE('',*,*,#22952,.F.);
#30611=ORIENTED_EDGE('',*,*,#22958,.F.);
#30612=ORIENTED_EDGE('',*,*,#22959,.T.);
#30613=ORIENTED_EDGE('',*,*,#22960,.T.);
#30614=ORIENTED_EDGE('',*,*,#22849,.F.);
#30615=ORIENTED_EDGE('',*,*,#22885,.T.);
#30616=ORIENTED_EDGE('',*,*,#22953,.F.);
#30617=ORIENTED_EDGE('',*,*,#22957,.F.);
#30618=ORIENTED_EDGE('',*,*,#22951,.T.);
#30619=ORIENTED_EDGE('',*,*,#22891,.F.);
#30620=ORIENTED_EDGE('',*,*,#22869,.F.);
#30621=ORIENTED_EDGE('',*,*,#22961,.T.);
#30622=ORIENTED_EDGE('',*,*,#22866,.T.);
#30623=ORIENTED_EDGE('',*,*,#22962,.F.);
#30624=ORIENTED_EDGE('',*,*,#22878,.T.);
#30625=ORIENTED_EDGE('',*,*,#22890,.T.);
#30626=ORIENTED_EDGE('',*,*,#22963,.F.);
#30627=ORIENTED_EDGE('',*,*,#22874,.F.);
#30628=ORIENTED_EDGE('',*,*,#22964,.T.);
#30629=ORIENTED_EDGE('',*,*,#22965,.T.);
#30630=ORIENTED_EDGE('',*,*,#22892,.F.);
#30631=ORIENTED_EDGE('',*,*,#22863,.F.);
#30632=ORIENTED_EDGE('',*,*,#22961,.F.);
#30633=ORIENTED_EDGE('',*,*,#22868,.T.);
#30634=ORIENTED_EDGE('',*,*,#22966,.T.);
#30635=ORIENTED_EDGE('',*,*,#22967,.F.);
#30636=ORIENTED_EDGE('',*,*,#22968,.F.);
#30637=ORIENTED_EDGE('',*,*,#22962,.T.);
#30638=ORIENTED_EDGE('',*,*,#22969,.T.);
#30639=ORIENTED_EDGE('',*,*,#22964,.F.);
#30640=ORIENTED_EDGE('',*,*,#22970,.F.);
#30641=ORIENTED_EDGE('',*,*,#22971,.T.);
#30642=ORIENTED_EDGE('',*,*,#22972,.T.);
#30643=ORIENTED_EDGE('',*,*,#22889,.T.);
#30644=ORIENTED_EDGE('',*,*,#22965,.F.);
#30645=ORIENTED_EDGE('',*,*,#22969,.F.);
#30646=ORIENTED_EDGE('',*,*,#22963,.T.);
#30647=ORIENTED_EDGE('',*,*,#22973,.F.);
#30648=ORIENTED_EDGE('',*,*,#22954,.F.);
#30649=ORIENTED_EDGE('',*,*,#22853,.F.);
#30650=ORIENTED_EDGE('',*,*,#22974,.F.);
#30651=ORIENTED_EDGE('',*,*,#22975,.T.);
#30652=ORIENTED_EDGE('',*,*,#22976,.F.);
#30653=ORIENTED_EDGE('',*,*,#22858,.T.);
#30654=ORIENTED_EDGE('',*,*,#22960,.F.);
#30655=ORIENTED_EDGE('',*,*,#22837,.F.);
#30656=ORIENTED_EDGE('',*,*,#22956,.T.);
#30657=ORIENTED_EDGE('',*,*,#22977,.T.);
#30658=ORIENTED_EDGE('',*,*,#22958,.T.);
#30659=ORIENTED_EDGE('',*,*,#22860,.F.);
#30660=ORIENTED_EDGE('',*,*,#22978,.T.);
#30661=ORIENTED_EDGE('',*,*,#22979,.F.);
#30662=ORIENTED_EDGE('',*,*,#22980,.T.);
#30663=ORIENTED_EDGE('',*,*,#22856,.T.);
#30664=ORIENTED_EDGE('',*,*,#22835,.T.);
#30665=ORIENTED_EDGE('',*,*,#22981,.F.);
#30666=ORIENTED_EDGE('',*,*,#22975,.F.);
#30667=ORIENTED_EDGE('',*,*,#22982,.T.);
#30668=ORIENTED_EDGE('',*,*,#22979,.T.);
#30669=ORIENTED_EDGE('',*,*,#22983,.F.);
#30670=ORIENTED_EDGE('',*,*,#22966,.F.);
#30671=ORIENTED_EDGE('',*,*,#22876,.F.);
#30672=ORIENTED_EDGE('',*,*,#22984,.F.);
#30673=ORIENTED_EDGE('',*,*,#22985,.T.);
#30674=ORIENTED_EDGE('',*,*,#22986,.F.);
#30675=ORIENTED_EDGE('',*,*,#22871,.T.);
#30676=ORIENTED_EDGE('',*,*,#22972,.F.);
#30677=ORIENTED_EDGE('',*,*,#22840,.F.);
#30678=ORIENTED_EDGE('',*,*,#22968,.T.);
#30679=ORIENTED_EDGE('',*,*,#22987,.T.);
#30680=ORIENTED_EDGE('',*,*,#22970,.T.);
#30681=ORIENTED_EDGE('',*,*,#22873,.F.);
#30682=ORIENTED_EDGE('',*,*,#22988,.F.);
#30683=ORIENTED_EDGE('',*,*,#22989,.F.);
#30684=ORIENTED_EDGE('',*,*,#22990,.F.);
#30685=ORIENTED_EDGE('',*,*,#22879,.T.);
#30686=ORIENTED_EDGE('',*,*,#22838,.T.);
#30687=ORIENTED_EDGE('',*,*,#22991,.F.);
#30688=ORIENTED_EDGE('',*,*,#22985,.F.);
#30689=ORIENTED_EDGE('',*,*,#22992,.F.);
#30690=ORIENTED_EDGE('',*,*,#22989,.T.);
#30691=ORIENTED_EDGE('',*,*,#22984,.T.);
#30692=ORIENTED_EDGE('',*,*,#22880,.T.);
#30693=ORIENTED_EDGE('',*,*,#22990,.T.);
#30694=ORIENTED_EDGE('',*,*,#22992,.T.);
#30695=ORIENTED_EDGE('',*,*,#22986,.T.);
#30696=ORIENTED_EDGE('',*,*,#22991,.T.);
#30697=ORIENTED_EDGE('',*,*,#22988,.T.);
#30698=ORIENTED_EDGE('',*,*,#22872,.F.);
#30699=ORIENTED_EDGE('',*,*,#22974,.T.);
#30700=ORIENTED_EDGE('',*,*,#22857,.T.);
#30701=ORIENTED_EDGE('',*,*,#22980,.F.);
#30702=ORIENTED_EDGE('',*,*,#22982,.F.);
#30703=ORIENTED_EDGE('',*,*,#22976,.T.);
#30704=ORIENTED_EDGE('',*,*,#22981,.T.);
#30705=ORIENTED_EDGE('',*,*,#22978,.F.);
#30706=ORIENTED_EDGE('',*,*,#22859,.F.);
#30707=ORIENTED_EDGE('',*,*,#22983,.T.);
#30708=ORIENTED_EDGE('',*,*,#22971,.F.);
#30709=ORIENTED_EDGE('',*,*,#22987,.F.);
#30710=ORIENTED_EDGE('',*,*,#22967,.T.);
#30711=ORIENTED_EDGE('',*,*,#22955,.T.);
#30712=ORIENTED_EDGE('',*,*,#22973,.T.);
#30713=ORIENTED_EDGE('',*,*,#22959,.F.);
#30714=ORIENTED_EDGE('',*,*,#22977,.F.);
#30715=ORIENTED_EDGE('',*,*,#22993,.F.);
#30716=ORIENTED_EDGE('',*,*,#22937,.F.);
#30717=ORIENTED_EDGE('',*,*,#22994,.T.);
#30718=ORIENTED_EDGE('',*,*,#22932,.F.);
#30719=ORIENTED_EDGE('',*,*,#22995,.F.);
#30720=ORIENTED_EDGE('',*,*,#22947,.F.);
#30721=ORIENTED_EDGE('',*,*,#22996,.T.);
#30722=ORIENTED_EDGE('',*,*,#22921,.F.);
#30723=ORIENTED_EDGE('',*,*,#22923,.F.);
#30724=ORIENTED_EDGE('',*,*,#22997,.F.);
#30725=ORIENTED_EDGE('',*,*,#22945,.T.);
#30726=ORIENTED_EDGE('',*,*,#22995,.T.);
#30727=ORIENTED_EDGE('',*,*,#22922,.F.);
#30728=ORIENTED_EDGE('',*,*,#22996,.F.);
#30729=ORIENTED_EDGE('',*,*,#22946,.T.);
#30730=ORIENTED_EDGE('',*,*,#22997,.T.);
#30731=ORIENTED_EDGE('',*,*,#22925,.F.);
#30732=ORIENTED_EDGE('',*,*,#22998,.F.);
#30733=ORIENTED_EDGE('',*,*,#22943,.T.);
#30734=ORIENTED_EDGE('',*,*,#22933,.T.);
#30735=ORIENTED_EDGE('',*,*,#22924,.F.);
#30736=ORIENTED_EDGE('',*,*,#22902,.F.);
#30737=ORIENTED_EDGE('',*,*,#22944,.T.);
#30738=ORIENTED_EDGE('',*,*,#22998,.T.);
#30739=ORIENTED_EDGE('',*,*,#22929,.T.);
#30740=ORIENTED_EDGE('',*,*,#22999,.F.);
#30741=ORIENTED_EDGE('',*,*,#22940,.F.);
#30742=ORIENTED_EDGE('',*,*,#22897,.T.);
#30743=ORIENTED_EDGE('',*,*,#22928,.T.);
#30744=ORIENTED_EDGE('',*,*,#22948,.F.);
#30745=ORIENTED_EDGE('',*,*,#22941,.F.);
#30746=ORIENTED_EDGE('',*,*,#22999,.T.);
#30747=ORIENTED_EDGE('',*,*,#22931,.T.);
#30748=ORIENTED_EDGE('',*,*,#23000,.F.);
#30749=ORIENTED_EDGE('',*,*,#22938,.F.);
#30750=ORIENTED_EDGE('',*,*,#22993,.T.);
#30751=ORIENTED_EDGE('',*,*,#22930,.T.);
#30752=ORIENTED_EDGE('',*,*,#22994,.F.);
#30753=ORIENTED_EDGE('',*,*,#22939,.F.);
#30754=ORIENTED_EDGE('',*,*,#23000,.T.);
#30755=ORIENTED_EDGE('',*,*,#22917,.T.);
#30756=ORIENTED_EDGE('',*,*,#23001,.F.);
#30757=ORIENTED_EDGE('',*,*,#22842,.F.);
#30758=ORIENTED_EDGE('',*,*,#23002,.T.);
#30759=ORIENTED_EDGE('',*,*,#22916,.T.);
#30760=ORIENTED_EDGE('',*,*,#23003,.F.);
#30761=ORIENTED_EDGE('',*,*,#22843,.F.);
#30762=ORIENTED_EDGE('',*,*,#23001,.T.);
#30763=ORIENTED_EDGE('',*,*,#22915,.T.);
#30764=ORIENTED_EDGE('',*,*,#23004,.F.);
#30765=ORIENTED_EDGE('',*,*,#22844,.F.);
#30766=ORIENTED_EDGE('',*,*,#23003,.T.);
#30767=ORIENTED_EDGE('',*,*,#22918,.T.);
#30768=ORIENTED_EDGE('',*,*,#23002,.F.);
#30769=ORIENTED_EDGE('',*,*,#22841,.T.);
#30770=ORIENTED_EDGE('',*,*,#23004,.T.);
#30771=ORIENTED_EDGE('',*,*,#22920,.T.);
#30772=ORIENTED_EDGE('',*,*,#23005,.T.);
#30773=ORIENTED_EDGE('',*,*,#23005,.F.);
#30774=ORIENTED_EDGE('',*,*,#22919,.T.);
#30775=ORIENTED_EDGE('',*,*,#22936,.T.);
#30776=ORIENTED_EDGE('',*,*,#23006,.T.);
#30777=ORIENTED_EDGE('',*,*,#23006,.F.);
#30778=ORIENTED_EDGE('',*,*,#22935,.T.);
#30779=ORIENTED_EDGE('',*,*,#23007,.F.);
#30780=ORIENTED_EDGE('',*,*,#23008,.T.);
#30781=ORIENTED_EDGE('',*,*,#23009,.T.);
#30782=ORIENTED_EDGE('',*,*,#23008,.F.);
#30783=ORIENTED_EDGE('',*,*,#23010,.F.);
#30784=ORIENTED_EDGE('',*,*,#23011,.T.);
#30785=ORIENTED_EDGE('',*,*,#23012,.T.);
#30786=ORIENTED_EDGE('',*,*,#23011,.F.);
#30787=ORIENTED_EDGE('',*,*,#23013,.F.);
#30788=ORIENTED_EDGE('',*,*,#23014,.T.);
#30789=ORIENTED_EDGE('',*,*,#23010,.T.);
#30790=ORIENTED_EDGE('',*,*,#23014,.F.);
#30791=ORIENTED_EDGE('',*,*,#23015,.T.);
#30792=ORIENTED_EDGE('',*,*,#23016,.T.);
#30793=ORIENTED_EDGE('',*,*,#23007,.T.);
#30794=ORIENTED_EDGE('',*,*,#23016,.F.);
#30795=ORIENTED_EDGE('',*,*,#23017,.F.);
#30796=ORIENTED_EDGE('',*,*,#23018,.F.);
#30797=ORIENTED_EDGE('',*,*,#23019,.T.);
#30798=ORIENTED_EDGE('',*,*,#23020,.F.);
#30799=ORIENTED_EDGE('',*,*,#23021,.T.);
#30800=ORIENTED_EDGE('',*,*,#23022,.T.);
#30801=ORIENTED_EDGE('',*,*,#23023,.F.);
#30802=ORIENTED_EDGE('',*,*,#23024,.T.);
#30803=ORIENTED_EDGE('',*,*,#23025,.T.);
#30804=ORIENTED_EDGE('',*,*,#23026,.T.);
#30805=ORIENTED_EDGE('',*,*,#23027,.F.);
#30806=ORIENTED_EDGE('',*,*,#23028,.F.);
#30807=ORIENTED_EDGE('',*,*,#23015,.F.);
#30808=ORIENTED_EDGE('',*,*,#23029,.F.);
#30809=ORIENTED_EDGE('',*,*,#23030,.F.);
#30810=ORIENTED_EDGE('',*,*,#23031,.T.);
#30811=ORIENTED_EDGE('',*,*,#23032,.T.);
#30812=ORIENTED_EDGE('',*,*,#23033,.F.);
#30813=ORIENTED_EDGE('',*,*,#23034,.T.);
#30814=ORIENTED_EDGE('',*,*,#23035,.T.);
#30815=ORIENTED_EDGE('',*,*,#23036,.F.);
#30816=ORIENTED_EDGE('',*,*,#23037,.F.);
#30817=ORIENTED_EDGE('',*,*,#23038,.F.);
#30818=ORIENTED_EDGE('',*,*,#23039,.T.);
#30819=ORIENTED_EDGE('',*,*,#23040,.T.);
#30820=ORIENTED_EDGE('',*,*,#23012,.F.);
#30821=ORIENTED_EDGE('',*,*,#23027,.T.);
#30822=ORIENTED_EDGE('',*,*,#23041,.T.);
#30823=ORIENTED_EDGE('',*,*,#23032,.F.);
#30824=ORIENTED_EDGE('',*,*,#23042,.T.);
#30825=ORIENTED_EDGE('',*,*,#23021,.F.);
#30826=ORIENTED_EDGE('',*,*,#23043,.T.);
#30827=ORIENTED_EDGE('',*,*,#23038,.T.);
#30828=ORIENTED_EDGE('',*,*,#23044,.T.);
#30829=ORIENTED_EDGE('',*,*,#23045,.F.);
#30830=ORIENTED_EDGE('',*,*,#23030,.T.);
#30831=ORIENTED_EDGE('',*,*,#23046,.F.);
#30832=ORIENTED_EDGE('',*,*,#23017,.T.);
#30833=ORIENTED_EDGE('',*,*,#23047,.F.);
#30834=ORIENTED_EDGE('',*,*,#23019,.F.);
#30835=ORIENTED_EDGE('',*,*,#23048,.T.);
#30836=ORIENTED_EDGE('',*,*,#23040,.F.);
#30837=ORIENTED_EDGE('',*,*,#23018,.T.);
#30838=ORIENTED_EDGE('',*,*,#23046,.T.);
#30839=ORIENTED_EDGE('',*,*,#23029,.T.);
#30840=ORIENTED_EDGE('',*,*,#23048,.F.);
#30841=ORIENTED_EDGE('',*,*,#23049,.F.);
#30842=ORIENTED_EDGE('',*,*,#23025,.F.);
#30843=ORIENTED_EDGE('',*,*,#23050,.T.);
#30844=ORIENTED_EDGE('',*,*,#23034,.F.);
#30845=ORIENTED_EDGE('',*,*,#23051,.T.);
#30846=ORIENTED_EDGE('',*,*,#23035,.F.);
#30847=ORIENTED_EDGE('',*,*,#23050,.F.);
#30848=ORIENTED_EDGE('',*,*,#23024,.F.);
#30849=ORIENTED_EDGE('',*,*,#23052,.F.);
#30850=ORIENTED_EDGE('',*,*,#23036,.T.);
#30851=ORIENTED_EDGE('',*,*,#23051,.F.);
#30852=ORIENTED_EDGE('',*,*,#23023,.T.);
#30853=ORIENTED_EDGE('',*,*,#23053,.T.);
#30854=ORIENTED_EDGE('',*,*,#23054,.T.);
#30855=ORIENTED_EDGE('',*,*,#23049,.T.);
#30856=ORIENTED_EDGE('',*,*,#23055,.F.);
#30857=ORIENTED_EDGE('',*,*,#23056,.T.);
#30858=ORIENTED_EDGE('',*,*,#23057,.F.);
#30859=ORIENTED_EDGE('',*,*,#23058,.F.);
#30860=ORIENTED_EDGE('',*,*,#23041,.F.);
#30861=ORIENTED_EDGE('',*,*,#23033,.T.);
#30862=ORIENTED_EDGE('',*,*,#23058,.T.);
#30863=ORIENTED_EDGE('',*,*,#23059,.F.);
#30864=ORIENTED_EDGE('',*,*,#23055,.T.);
#30865=ORIENTED_EDGE('',*,*,#23026,.F.);
#30866=ORIENTED_EDGE('',*,*,#23054,.F.);
#30867=ORIENTED_EDGE('',*,*,#23060,.T.);
#30868=ORIENTED_EDGE('',*,*,#23056,.F.);
#30869=ORIENTED_EDGE('',*,*,#23052,.T.);
#30870=ORIENTED_EDGE('',*,*,#23061,.T.);
#30871=ORIENTED_EDGE('',*,*,#23062,.T.);
#30872=ORIENTED_EDGE('',*,*,#23063,.F.);
#30873=ORIENTED_EDGE('',*,*,#23064,.F.);
#30874=ORIENTED_EDGE('',*,*,#23065,.T.);
#30875=ORIENTED_EDGE('',*,*,#23044,.F.);
#30876=ORIENTED_EDGE('',*,*,#23066,.F.);
#30877=ORIENTED_EDGE('',*,*,#23066,.T.);
#30878=ORIENTED_EDGE('',*,*,#23037,.T.);
#30879=ORIENTED_EDGE('',*,*,#23063,.T.);
#30880=ORIENTED_EDGE('',*,*,#23067,.F.);
#30881=ORIENTED_EDGE('',*,*,#23065,.F.);
#30882=ORIENTED_EDGE('',*,*,#23068,.T.);
#30883=ORIENTED_EDGE('',*,*,#23061,.F.);
#30884=ORIENTED_EDGE('',*,*,#23022,.F.);
#30885=ORIENTED_EDGE('',*,*,#23069,.F.);
#30886=ORIENTED_EDGE('',*,*,#23070,.F.);
#30887=ORIENTED_EDGE('',*,*,#23071,.F.);
#30888=ORIENTED_EDGE('',*,*,#23072,.F.);
#30889=ORIENTED_EDGE('',*,*,#23073,.T.);
#30890=ORIENTED_EDGE('',*,*,#23074,.T.);
#30891=ORIENTED_EDGE('',*,*,#23075,.T.);
#30892=ORIENTED_EDGE('',*,*,#23076,.F.);
#30893=ORIENTED_EDGE('',*,*,#23077,.F.);
#30894=ORIENTED_EDGE('',*,*,#23078,.F.);
#30895=ORIENTED_EDGE('',*,*,#23079,.F.);
#30896=ORIENTED_EDGE('',*,*,#23080,.F.);
#30897=ORIENTED_EDGE('',*,*,#23081,.F.);
#30898=ORIENTED_EDGE('',*,*,#23078,.T.);
#30899=ORIENTED_EDGE('',*,*,#23082,.T.);
#30900=ORIENTED_EDGE('',*,*,#23072,.T.);
#30901=ORIENTED_EDGE('',*,*,#23082,.F.);
#30902=ORIENTED_EDGE('',*,*,#23077,.T.);
#30903=ORIENTED_EDGE('',*,*,#23083,.F.);
#30904=ORIENTED_EDGE('',*,*,#23067,.T.);
#30905=ORIENTED_EDGE('',*,*,#23084,.F.);
#30906=ORIENTED_EDGE('',*,*,#23075,.F.);
#30907=ORIENTED_EDGE('',*,*,#23085,.T.);
#30908=ORIENTED_EDGE('',*,*,#23059,.T.);
#30909=ORIENTED_EDGE('',*,*,#23086,.T.);
#30910=ORIENTED_EDGE('',*,*,#23069,.T.);
#30911=ORIENTED_EDGE('',*,*,#23062,.F.);
#30912=ORIENTED_EDGE('',*,*,#23087,.T.);
#30913=ORIENTED_EDGE('',*,*,#23076,.T.);
#30914=ORIENTED_EDGE('',*,*,#23084,.T.);
#30915=ORIENTED_EDGE('',*,*,#23088,.T.);
#30916=ORIENTED_EDGE('',*,*,#23079,.T.);
#30917=ORIENTED_EDGE('',*,*,#23081,.T.);
#30918=ORIENTED_EDGE('',*,*,#23071,.T.);
#30919=ORIENTED_EDGE('',*,*,#23089,.F.);
#30920=ORIENTED_EDGE('',*,*,#23060,.F.);
#30921=ORIENTED_EDGE('',*,*,#23090,.T.);
#30922=ORIENTED_EDGE('',*,*,#23073,.F.);
#30923=ORIENTED_EDGE('',*,*,#23087,.F.);
#30924=ORIENTED_EDGE('',*,*,#23068,.F.);
#30925=ORIENTED_EDGE('',*,*,#23083,.T.);
#30926=ORIENTED_EDGE('',*,*,#23080,.T.);
#30927=ORIENTED_EDGE('',*,*,#23088,.F.);
#30928=ORIENTED_EDGE('',*,*,#23064,.T.);
#30929=ORIENTED_EDGE('',*,*,#23089,.T.);
#30930=ORIENTED_EDGE('',*,*,#23070,.T.);
#30931=ORIENTED_EDGE('',*,*,#23086,.F.);
#30932=ORIENTED_EDGE('',*,*,#23057,.T.);
#30933=ORIENTED_EDGE('',*,*,#23053,.F.);
#30934=ORIENTED_EDGE('',*,*,#23085,.F.);
#30935=ORIENTED_EDGE('',*,*,#23074,.F.);
#30936=ORIENTED_EDGE('',*,*,#23090,.F.);
#30937=ORIENTED_EDGE('',*,*,#23091,.T.);
#30938=ORIENTED_EDGE('',*,*,#23092,.T.);
#30939=ORIENTED_EDGE('',*,*,#23047,.T.);
#30940=ORIENTED_EDGE('',*,*,#23093,.F.);
#30941=ORIENTED_EDGE('',*,*,#23094,.T.);
#30942=ORIENTED_EDGE('',*,*,#23095,.F.);
#30943=ORIENTED_EDGE('',*,*,#23096,.F.);
#30944=ORIENTED_EDGE('',*,*,#23043,.F.);
#30945=ORIENTED_EDGE('',*,*,#23039,.F.);
#30946=ORIENTED_EDGE('',*,*,#23096,.T.);
#30947=ORIENTED_EDGE('',*,*,#23097,.T.);
#30948=ORIENTED_EDGE('',*,*,#23093,.T.);
#30949=ORIENTED_EDGE('',*,*,#23020,.T.);
#30950=ORIENTED_EDGE('',*,*,#23092,.F.);
#30951=ORIENTED_EDGE('',*,*,#23098,.F.);
#30952=ORIENTED_EDGE('',*,*,#23094,.F.);
#30953=ORIENTED_EDGE('',*,*,#23045,.T.);
#30954=ORIENTED_EDGE('',*,*,#23099,.T.);
#30955=ORIENTED_EDGE('',*,*,#23100,.T.);
#30956=ORIENTED_EDGE('',*,*,#23101,.F.);
#30957=ORIENTED_EDGE('',*,*,#23102,.F.);
#30958=ORIENTED_EDGE('',*,*,#23103,.T.);
#30959=ORIENTED_EDGE('',*,*,#23042,.F.);
#30960=ORIENTED_EDGE('',*,*,#23104,.F.);
#30961=ORIENTED_EDGE('',*,*,#23104,.T.);
#30962=ORIENTED_EDGE('',*,*,#23031,.F.);
#30963=ORIENTED_EDGE('',*,*,#23101,.T.);
#30964=ORIENTED_EDGE('',*,*,#23105,.T.);
#30965=ORIENTED_EDGE('',*,*,#23103,.F.);
#30966=ORIENTED_EDGE('',*,*,#23106,.F.);
#30967=ORIENTED_EDGE('',*,*,#23099,.F.);
#30968=ORIENTED_EDGE('',*,*,#23028,.T.);
#30969=ORIENTED_EDGE('',*,*,#23107,.F.);
#30970=ORIENTED_EDGE('',*,*,#23108,.F.);
#30971=ORIENTED_EDGE('',*,*,#23109,.F.);
#30972=ORIENTED_EDGE('',*,*,#23110,.F.);
#30973=ORIENTED_EDGE('',*,*,#23111,.T.);
#30974=ORIENTED_EDGE('',*,*,#23112,.F.);
#30975=ORIENTED_EDGE('',*,*,#23113,.F.);
#30976=ORIENTED_EDGE('',*,*,#23114,.F.);
#30977=ORIENTED_EDGE('',*,*,#23115,.F.);
#30978=ORIENTED_EDGE('',*,*,#23116,.F.);
#30979=ORIENTED_EDGE('',*,*,#23117,.F.);
#30980=ORIENTED_EDGE('',*,*,#23118,.F.);
#30981=ORIENTED_EDGE('',*,*,#23119,.T.);
#30982=ORIENTED_EDGE('',*,*,#23118,.T.);
#30983=ORIENTED_EDGE('',*,*,#23120,.F.);
#30984=ORIENTED_EDGE('',*,*,#23108,.T.);
#30985=ORIENTED_EDGE('',*,*,#23120,.T.);
#30986=ORIENTED_EDGE('',*,*,#23117,.T.);
#30987=ORIENTED_EDGE('',*,*,#23121,.T.);
#30988=ORIENTED_EDGE('',*,*,#23105,.F.);
#30989=ORIENTED_EDGE('',*,*,#23122,.F.);
#30990=ORIENTED_EDGE('',*,*,#23112,.T.);
#30991=ORIENTED_EDGE('',*,*,#23123,.T.);
#30992=ORIENTED_EDGE('',*,*,#23097,.F.);
#30993=ORIENTED_EDGE('',*,*,#23124,.F.);
#30994=ORIENTED_EDGE('',*,*,#23109,.T.);
#30995=ORIENTED_EDGE('',*,*,#23100,.F.);
#30996=ORIENTED_EDGE('',*,*,#23125,.T.);
#30997=ORIENTED_EDGE('',*,*,#23113,.T.);
#30998=ORIENTED_EDGE('',*,*,#23122,.T.);
#30999=ORIENTED_EDGE('',*,*,#23126,.F.);
#31000=ORIENTED_EDGE('',*,*,#23115,.T.);
#31001=ORIENTED_EDGE('',*,*,#23119,.F.);
#31002=ORIENTED_EDGE('',*,*,#23107,.T.);
#31003=ORIENTED_EDGE('',*,*,#23127,.T.);
#31004=ORIENTED_EDGE('',*,*,#23098,.T.);
#31005=ORIENTED_EDGE('',*,*,#23128,.T.);
#31006=ORIENTED_EDGE('',*,*,#23114,.T.);
#31007=ORIENTED_EDGE('',*,*,#23125,.F.);
#31008=ORIENTED_EDGE('',*,*,#23106,.T.);
#31009=ORIENTED_EDGE('',*,*,#23121,.F.);
#31010=ORIENTED_EDGE('',*,*,#23116,.T.);
#31011=ORIENTED_EDGE('',*,*,#23126,.T.);
#31012=ORIENTED_EDGE('',*,*,#23102,.T.);
#31013=ORIENTED_EDGE('',*,*,#23127,.F.);
#31014=ORIENTED_EDGE('',*,*,#23110,.T.);
#31015=ORIENTED_EDGE('',*,*,#23124,.T.);
#31016=ORIENTED_EDGE('',*,*,#23095,.T.);
#31017=ORIENTED_EDGE('',*,*,#23091,.F.);
#31018=ORIENTED_EDGE('',*,*,#23123,.F.);
#31019=ORIENTED_EDGE('',*,*,#23111,.F.);
#31020=ORIENTED_EDGE('',*,*,#23128,.F.);
#31021=ORIENTED_EDGE('',*,*,#23013,.T.);
#31022=ORIENTED_EDGE('',*,*,#23129,.F.);
#31023=ORIENTED_EDGE('',*,*,#23130,.F.);
#31024=ORIENTED_EDGE('',*,*,#23131,.F.);
#31025=ORIENTED_EDGE('',*,*,#23132,.F.);
#31026=ORIENTED_EDGE('',*,*,#23133,.F.);
#31027=ORIENTED_EDGE('',*,*,#23134,.F.);
#31028=ORIENTED_EDGE('',*,*,#23135,.F.);
#31029=ORIENTED_EDGE('',*,*,#23136,.F.);
#31030=ORIENTED_EDGE('',*,*,#23137,.F.);
#31031=ORIENTED_EDGE('',*,*,#23138,.F.);
#31032=ORIENTED_EDGE('',*,*,#23139,.F.);
#31033=ORIENTED_EDGE('',*,*,#23140,.F.);
#31034=ORIENTED_EDGE('',*,*,#23141,.F.);
#31035=ORIENTED_EDGE('',*,*,#23142,.F.);
#31036=ORIENTED_EDGE('',*,*,#23143,.F.);
#31037=ORIENTED_EDGE('',*,*,#23144,.F.);
#31038=ORIENTED_EDGE('',*,*,#23145,.F.);
#31039=ORIENTED_EDGE('',*,*,#23146,.F.);
#31040=ORIENTED_EDGE('',*,*,#23147,.F.);
#31041=ORIENTED_EDGE('',*,*,#23148,.F.);
#31042=ORIENTED_EDGE('',*,*,#23149,.F.);
#31043=ORIENTED_EDGE('',*,*,#23150,.F.);
#31044=ORIENTED_EDGE('',*,*,#23151,.F.);
#31045=ORIENTED_EDGE('',*,*,#23152,.F.);
#31046=ORIENTED_EDGE('',*,*,#23153,.F.);
#31047=ORIENTED_EDGE('',*,*,#23154,.F.);
#31048=ORIENTED_EDGE('',*,*,#23155,.F.);
#31049=ORIENTED_EDGE('',*,*,#23156,.F.);
#31050=ORIENTED_EDGE('',*,*,#23157,.F.);
#31051=ORIENTED_EDGE('',*,*,#23158,.F.);
#31052=ORIENTED_EDGE('',*,*,#23159,.F.);
#31053=ORIENTED_EDGE('',*,*,#23160,.F.);
#31054=ORIENTED_EDGE('',*,*,#23161,.F.);
#31055=ORIENTED_EDGE('',*,*,#23162,.F.);
#31056=ORIENTED_EDGE('',*,*,#23163,.F.);
#31057=ORIENTED_EDGE('',*,*,#23164,.F.);
#31058=ORIENTED_EDGE('',*,*,#23165,.F.);
#31059=ORIENTED_EDGE('',*,*,#23166,.F.);
#31060=ORIENTED_EDGE('',*,*,#23167,.F.);
#31061=ORIENTED_EDGE('',*,*,#23168,.F.);
#31062=ORIENTED_EDGE('',*,*,#23169,.F.);
#31063=ORIENTED_EDGE('',*,*,#23170,.F.);
#31064=ORIENTED_EDGE('',*,*,#23171,.F.);
#31065=ORIENTED_EDGE('',*,*,#23172,.F.);
#31066=ORIENTED_EDGE('',*,*,#23173,.F.);
#31067=ORIENTED_EDGE('',*,*,#23174,.F.);
#31068=ORIENTED_EDGE('',*,*,#23175,.F.);
#31069=ORIENTED_EDGE('',*,*,#23176,.F.);
#31070=ORIENTED_EDGE('',*,*,#23177,.F.);
#31071=ORIENTED_EDGE('',*,*,#23178,.F.);
#31072=ORIENTED_EDGE('',*,*,#23179,.F.);
#31073=ORIENTED_EDGE('',*,*,#23180,.F.);
#31074=ORIENTED_EDGE('',*,*,#23181,.F.);
#31075=ORIENTED_EDGE('',*,*,#23182,.F.);
#31076=ORIENTED_EDGE('',*,*,#23183,.F.);
#31077=ORIENTED_EDGE('',*,*,#23184,.F.);
#31078=ORIENTED_EDGE('',*,*,#23185,.F.);
#31079=ORIENTED_EDGE('',*,*,#23186,.F.);
#31080=ORIENTED_EDGE('',*,*,#23187,.F.);
#31081=ORIENTED_EDGE('',*,*,#23188,.F.);
#31082=ORIENTED_EDGE('',*,*,#23189,.F.);
#31083=ORIENTED_EDGE('',*,*,#23190,.F.);
#31084=ORIENTED_EDGE('',*,*,#23191,.F.);
#31085=ORIENTED_EDGE('',*,*,#23192,.F.);
#31086=ORIENTED_EDGE('',*,*,#23193,.F.);
#31087=ORIENTED_EDGE('',*,*,#23194,.F.);
#31088=ORIENTED_EDGE('',*,*,#23195,.F.);
#31089=ORIENTED_EDGE('',*,*,#23196,.F.);
#31090=ORIENTED_EDGE('',*,*,#23197,.F.);
#31091=ORIENTED_EDGE('',*,*,#23198,.F.);
#31092=ORIENTED_EDGE('',*,*,#23199,.F.);
#31093=ORIENTED_EDGE('',*,*,#23200,.F.);
#31094=ORIENTED_EDGE('',*,*,#23201,.F.);
#31095=ORIENTED_EDGE('',*,*,#23202,.F.);
#31096=ORIENTED_EDGE('',*,*,#23203,.F.);
#31097=ORIENTED_EDGE('',*,*,#23204,.F.);
#31098=ORIENTED_EDGE('',*,*,#23205,.F.);
#31099=ORIENTED_EDGE('',*,*,#23206,.F.);
#31100=ORIENTED_EDGE('',*,*,#23207,.F.);
#31101=ORIENTED_EDGE('',*,*,#23208,.F.);
#31102=ORIENTED_EDGE('',*,*,#23209,.F.);
#31103=ORIENTED_EDGE('',*,*,#23210,.F.);
#31104=ORIENTED_EDGE('',*,*,#23211,.F.);
#31105=ORIENTED_EDGE('',*,*,#23212,.F.);
#31106=ORIENTED_EDGE('',*,*,#23213,.F.);
#31107=ORIENTED_EDGE('',*,*,#23214,.F.);
#31108=ORIENTED_EDGE('',*,*,#23215,.F.);
#31109=ORIENTED_EDGE('',*,*,#23216,.F.);
#31110=ORIENTED_EDGE('',*,*,#23217,.F.);
#31111=ORIENTED_EDGE('',*,*,#23218,.F.);
#31112=ORIENTED_EDGE('',*,*,#23219,.F.);
#31113=ORIENTED_EDGE('',*,*,#23220,.F.);
#31114=ORIENTED_EDGE('',*,*,#23221,.F.);
#31115=ORIENTED_EDGE('',*,*,#23222,.F.);
#31116=ORIENTED_EDGE('',*,*,#23223,.F.);
#31117=ORIENTED_EDGE('',*,*,#23224,.F.);
#31118=ORIENTED_EDGE('',*,*,#23225,.F.);
#31119=ORIENTED_EDGE('',*,*,#23226,.F.);
#31120=ORIENTED_EDGE('',*,*,#23227,.F.);
#31121=ORIENTED_EDGE('',*,*,#23228,.F.);
#31122=ORIENTED_EDGE('',*,*,#23229,.F.);
#31123=ORIENTED_EDGE('',*,*,#23230,.F.);
#31124=ORIENTED_EDGE('',*,*,#23231,.F.);
#31125=ORIENTED_EDGE('',*,*,#23232,.F.);
#31126=ORIENTED_EDGE('',*,*,#23233,.F.);
#31127=ORIENTED_EDGE('',*,*,#23234,.F.);
#31128=ORIENTED_EDGE('',*,*,#23235,.F.);
#31129=ORIENTED_EDGE('',*,*,#23236,.F.);
#31130=ORIENTED_EDGE('',*,*,#23237,.F.);
#31131=ORIENTED_EDGE('',*,*,#23238,.F.);
#31132=ORIENTED_EDGE('',*,*,#23239,.F.);
#31133=ORIENTED_EDGE('',*,*,#23240,.F.);
#31134=ORIENTED_EDGE('',*,*,#23241,.F.);
#31135=ORIENTED_EDGE('',*,*,#23242,.F.);
#31136=ORIENTED_EDGE('',*,*,#23243,.F.);
#31137=ORIENTED_EDGE('',*,*,#23244,.F.);
#31138=ORIENTED_EDGE('',*,*,#23245,.F.);
#31139=ORIENTED_EDGE('',*,*,#23246,.F.);
#31140=ORIENTED_EDGE('',*,*,#23247,.F.);
#31141=ORIENTED_EDGE('',*,*,#23248,.F.);
#31142=ORIENTED_EDGE('',*,*,#23249,.F.);
#31143=ORIENTED_EDGE('',*,*,#23250,.F.);
#31144=ORIENTED_EDGE('',*,*,#23251,.F.);
#31145=ORIENTED_EDGE('',*,*,#23252,.F.);
#31146=ORIENTED_EDGE('',*,*,#23253,.F.);
#31147=ORIENTED_EDGE('',*,*,#23254,.F.);
#31148=ORIENTED_EDGE('',*,*,#23255,.F.);
#31149=ORIENTED_EDGE('',*,*,#23256,.F.);
#31150=ORIENTED_EDGE('',*,*,#23257,.F.);
#31151=ORIENTED_EDGE('',*,*,#23258,.F.);
#31152=ORIENTED_EDGE('',*,*,#23259,.F.);
#31153=ORIENTED_EDGE('',*,*,#23260,.F.);
#31154=ORIENTED_EDGE('',*,*,#23261,.F.);
#31155=ORIENTED_EDGE('',*,*,#23262,.F.);
#31156=ORIENTED_EDGE('',*,*,#23263,.F.);
#31157=ORIENTED_EDGE('',*,*,#23264,.F.);
#31158=ORIENTED_EDGE('',*,*,#23265,.F.);
#31159=ORIENTED_EDGE('',*,*,#23266,.F.);
#31160=ORIENTED_EDGE('',*,*,#23267,.F.);
#31161=ORIENTED_EDGE('',*,*,#23268,.F.);
#31162=ORIENTED_EDGE('',*,*,#23269,.F.);
#31163=ORIENTED_EDGE('',*,*,#23270,.F.);
#31164=ORIENTED_EDGE('',*,*,#23271,.F.);
#31165=ORIENTED_EDGE('',*,*,#23272,.F.);
#31166=ORIENTED_EDGE('',*,*,#23273,.F.);
#31167=ORIENTED_EDGE('',*,*,#23274,.F.);
#31168=ORIENTED_EDGE('',*,*,#23275,.F.);
#31169=ORIENTED_EDGE('',*,*,#23276,.F.);
#31170=ORIENTED_EDGE('',*,*,#23277,.F.);
#31171=ORIENTED_EDGE('',*,*,#23278,.F.);
#31172=ORIENTED_EDGE('',*,*,#23279,.F.);
#31173=ORIENTED_EDGE('',*,*,#23280,.F.);
#31174=ORIENTED_EDGE('',*,*,#23281,.F.);
#31175=ORIENTED_EDGE('',*,*,#23282,.F.);
#31176=ORIENTED_EDGE('',*,*,#23283,.F.);
#31177=ORIENTED_EDGE('',*,*,#23284,.F.);
#31178=ORIENTED_EDGE('',*,*,#23285,.F.);
#31179=ORIENTED_EDGE('',*,*,#23286,.F.);
#31180=ORIENTED_EDGE('',*,*,#23287,.F.);
#31181=ORIENTED_EDGE('',*,*,#23288,.F.);
#31182=ORIENTED_EDGE('',*,*,#23289,.F.);
#31183=ORIENTED_EDGE('',*,*,#23290,.F.);
#31184=ORIENTED_EDGE('',*,*,#23291,.F.);
#31185=ORIENTED_EDGE('',*,*,#23292,.F.);
#31186=ORIENTED_EDGE('',*,*,#23293,.F.);
#31187=ORIENTED_EDGE('',*,*,#23294,.F.);
#31188=ORIENTED_EDGE('',*,*,#23295,.F.);
#31189=ORIENTED_EDGE('',*,*,#23296,.F.);
#31190=ORIENTED_EDGE('',*,*,#23297,.F.);
#31191=ORIENTED_EDGE('',*,*,#23298,.F.);
#31192=ORIENTED_EDGE('',*,*,#23299,.F.);
#31193=ORIENTED_EDGE('',*,*,#23300,.F.);
#31194=ORIENTED_EDGE('',*,*,#23301,.F.);
#31195=ORIENTED_EDGE('',*,*,#23302,.F.);
#31196=ORIENTED_EDGE('',*,*,#23303,.F.);
#31197=ORIENTED_EDGE('',*,*,#23304,.F.);
#31198=ORIENTED_EDGE('',*,*,#23305,.F.);
#31199=ORIENTED_EDGE('',*,*,#23306,.F.);
#31200=ORIENTED_EDGE('',*,*,#23307,.F.);
#31201=ORIENTED_EDGE('',*,*,#23308,.F.);
#31202=ORIENTED_EDGE('',*,*,#23309,.F.);
#31203=ORIENTED_EDGE('',*,*,#23310,.F.);
#31204=ORIENTED_EDGE('',*,*,#23311,.F.);
#31205=ORIENTED_EDGE('',*,*,#23312,.F.);
#31206=ORIENTED_EDGE('',*,*,#23313,.F.);
#31207=ORIENTED_EDGE('',*,*,#23314,.F.);
#31208=ORIENTED_EDGE('',*,*,#23315,.F.);
#31209=ORIENTED_EDGE('',*,*,#23316,.F.);
#31210=ORIENTED_EDGE('',*,*,#23317,.F.);
#31211=ORIENTED_EDGE('',*,*,#23318,.F.);
#31212=ORIENTED_EDGE('',*,*,#23319,.F.);
#31213=ORIENTED_EDGE('',*,*,#23320,.F.);
#31214=ORIENTED_EDGE('',*,*,#23321,.F.);
#31215=ORIENTED_EDGE('',*,*,#23322,.F.);
#31216=ORIENTED_EDGE('',*,*,#23323,.F.);
#31217=ORIENTED_EDGE('',*,*,#23324,.F.);
#31218=ORIENTED_EDGE('',*,*,#23325,.F.);
#31219=ORIENTED_EDGE('',*,*,#23326,.F.);
#31220=ORIENTED_EDGE('',*,*,#23327,.F.);
#31221=ORIENTED_EDGE('',*,*,#23328,.F.);
#31222=ORIENTED_EDGE('',*,*,#23329,.F.);
#31223=ORIENTED_EDGE('',*,*,#23330,.F.);
#31224=ORIENTED_EDGE('',*,*,#23331,.F.);
#31225=ORIENTED_EDGE('',*,*,#23332,.F.);
#31226=ORIENTED_EDGE('',*,*,#23333,.F.);
#31227=ORIENTED_EDGE('',*,*,#23334,.F.);
#31228=ORIENTED_EDGE('',*,*,#23335,.F.);
#31229=ORIENTED_EDGE('',*,*,#23336,.F.);
#31230=ORIENTED_EDGE('',*,*,#23337,.F.);
#31231=ORIENTED_EDGE('',*,*,#23338,.F.);
#31232=ORIENTED_EDGE('',*,*,#23339,.F.);
#31233=ORIENTED_EDGE('',*,*,#23340,.F.);
#31234=ORIENTED_EDGE('',*,*,#23341,.F.);
#31235=ORIENTED_EDGE('',*,*,#23342,.F.);
#31236=ORIENTED_EDGE('',*,*,#23343,.F.);
#31237=ORIENTED_EDGE('',*,*,#23344,.F.);
#31238=ORIENTED_EDGE('',*,*,#23345,.F.);
#31239=ORIENTED_EDGE('',*,*,#23346,.F.);
#31240=ORIENTED_EDGE('',*,*,#23347,.F.);
#31241=ORIENTED_EDGE('',*,*,#23348,.F.);
#31242=ORIENTED_EDGE('',*,*,#23349,.F.);
#31243=ORIENTED_EDGE('',*,*,#23350,.F.);
#31244=ORIENTED_EDGE('',*,*,#23351,.F.);
#31245=ORIENTED_EDGE('',*,*,#23352,.F.);
#31246=ORIENTED_EDGE('',*,*,#23353,.F.);
#31247=ORIENTED_EDGE('',*,*,#23354,.F.);
#31248=ORIENTED_EDGE('',*,*,#23355,.F.);
#31249=ORIENTED_EDGE('',*,*,#23356,.F.);
#31250=ORIENTED_EDGE('',*,*,#23357,.F.);
#31251=ORIENTED_EDGE('',*,*,#23358,.F.);
#31252=ORIENTED_EDGE('',*,*,#23359,.F.);
#31253=ORIENTED_EDGE('',*,*,#23360,.F.);
#31254=ORIENTED_EDGE('',*,*,#23361,.F.);
#31255=ORIENTED_EDGE('',*,*,#23362,.F.);
#31256=ORIENTED_EDGE('',*,*,#23363,.F.);
#31257=ORIENTED_EDGE('',*,*,#23364,.F.);
#31258=ORIENTED_EDGE('',*,*,#23365,.F.);
#31259=ORIENTED_EDGE('',*,*,#23366,.F.);
#31260=ORIENTED_EDGE('',*,*,#23367,.F.);
#31261=ORIENTED_EDGE('',*,*,#23368,.F.);
#31262=ORIENTED_EDGE('',*,*,#23369,.F.);
#31263=ORIENTED_EDGE('',*,*,#23370,.F.);
#31264=ORIENTED_EDGE('',*,*,#23371,.F.);
#31265=ORIENTED_EDGE('',*,*,#23372,.F.);
#31266=ORIENTED_EDGE('',*,*,#23373,.F.);
#31267=ORIENTED_EDGE('',*,*,#23374,.F.);
#31268=ORIENTED_EDGE('',*,*,#23375,.F.);
#31269=ORIENTED_EDGE('',*,*,#23376,.F.);
#31270=ORIENTED_EDGE('',*,*,#23377,.F.);
#31271=ORIENTED_EDGE('',*,*,#23378,.F.);
#31272=ORIENTED_EDGE('',*,*,#23379,.F.);
#31273=ORIENTED_EDGE('',*,*,#23380,.F.);
#31274=ORIENTED_EDGE('',*,*,#23381,.F.);
#31275=ORIENTED_EDGE('',*,*,#23382,.F.);
#31276=ORIENTED_EDGE('',*,*,#23383,.F.);
#31277=ORIENTED_EDGE('',*,*,#23384,.F.);
#31278=ORIENTED_EDGE('',*,*,#23385,.F.);
#31279=ORIENTED_EDGE('',*,*,#23386,.F.);
#31280=ORIENTED_EDGE('',*,*,#23387,.F.);
#31281=ORIENTED_EDGE('',*,*,#23388,.F.);
#31282=ORIENTED_EDGE('',*,*,#23389,.F.);
#31283=ORIENTED_EDGE('',*,*,#23390,.F.);
#31284=ORIENTED_EDGE('',*,*,#23391,.F.);
#31285=ORIENTED_EDGE('',*,*,#23392,.F.);
#31286=ORIENTED_EDGE('',*,*,#23393,.F.);
#31287=ORIENTED_EDGE('',*,*,#23394,.F.);
#31288=ORIENTED_EDGE('',*,*,#23395,.F.);
#31289=ORIENTED_EDGE('',*,*,#23396,.F.);
#31290=ORIENTED_EDGE('',*,*,#23397,.F.);
#31291=ORIENTED_EDGE('',*,*,#23398,.F.);
#31292=ORIENTED_EDGE('',*,*,#23399,.F.);
#31293=ORIENTED_EDGE('',*,*,#23400,.F.);
#31294=ORIENTED_EDGE('',*,*,#23401,.F.);
#31295=ORIENTED_EDGE('',*,*,#23402,.F.);
#31296=ORIENTED_EDGE('',*,*,#23403,.F.);
#31297=ORIENTED_EDGE('',*,*,#23404,.F.);
#31298=ORIENTED_EDGE('',*,*,#23405,.F.);
#31299=ORIENTED_EDGE('',*,*,#23406,.F.);
#31300=ORIENTED_EDGE('',*,*,#23407,.F.);
#31301=ORIENTED_EDGE('',*,*,#23408,.F.);
#31302=ORIENTED_EDGE('',*,*,#23409,.F.);
#31303=ORIENTED_EDGE('',*,*,#23410,.F.);
#31304=ORIENTED_EDGE('',*,*,#23411,.F.);
#31305=ORIENTED_EDGE('',*,*,#23412,.F.);
#31306=ORIENTED_EDGE('',*,*,#23413,.F.);
#31307=ORIENTED_EDGE('',*,*,#23414,.F.);
#31308=ORIENTED_EDGE('',*,*,#23415,.F.);
#31309=ORIENTED_EDGE('',*,*,#23416,.F.);
#31310=ORIENTED_EDGE('',*,*,#23417,.F.);
#31311=ORIENTED_EDGE('',*,*,#23418,.F.);
#31312=ORIENTED_EDGE('',*,*,#23419,.F.);
#31313=ORIENTED_EDGE('',*,*,#23420,.F.);
#31314=ORIENTED_EDGE('',*,*,#23421,.F.);
#31315=ORIENTED_EDGE('',*,*,#23422,.F.);
#31316=ORIENTED_EDGE('',*,*,#23423,.F.);
#31317=ORIENTED_EDGE('',*,*,#23424,.F.);
#31318=ORIENTED_EDGE('',*,*,#23425,.F.);
#31319=ORIENTED_EDGE('',*,*,#23426,.F.);
#31320=ORIENTED_EDGE('',*,*,#23427,.F.);
#31321=ORIENTED_EDGE('',*,*,#23428,.F.);
#31322=ORIENTED_EDGE('',*,*,#23429,.F.);
#31323=ORIENTED_EDGE('',*,*,#23430,.F.);
#31324=ORIENTED_EDGE('',*,*,#23431,.F.);
#31325=ORIENTED_EDGE('',*,*,#23432,.F.);
#31326=ORIENTED_EDGE('',*,*,#23433,.F.);
#31327=ORIENTED_EDGE('',*,*,#23434,.F.);
#31328=ORIENTED_EDGE('',*,*,#23435,.F.);
#31329=ORIENTED_EDGE('',*,*,#23436,.F.);
#31330=ORIENTED_EDGE('',*,*,#23437,.F.);
#31331=ORIENTED_EDGE('',*,*,#23438,.F.);
#31332=ORIENTED_EDGE('',*,*,#23439,.F.);
#31333=ORIENTED_EDGE('',*,*,#23440,.F.);
#31334=ORIENTED_EDGE('',*,*,#23441,.F.);
#31335=ORIENTED_EDGE('',*,*,#23442,.F.);
#31336=ORIENTED_EDGE('',*,*,#23443,.F.);
#31337=ORIENTED_EDGE('',*,*,#23444,.F.);
#31338=ORIENTED_EDGE('',*,*,#23445,.F.);
#31339=ORIENTED_EDGE('',*,*,#23446,.F.);
#31340=ORIENTED_EDGE('',*,*,#23447,.F.);
#31341=ORIENTED_EDGE('',*,*,#23448,.F.);
#31342=ORIENTED_EDGE('',*,*,#23449,.F.);
#31343=ORIENTED_EDGE('',*,*,#23450,.F.);
#31344=ORIENTED_EDGE('',*,*,#23451,.F.);
#31345=ORIENTED_EDGE('',*,*,#23452,.F.);
#31346=ORIENTED_EDGE('',*,*,#23453,.F.);
#31347=ORIENTED_EDGE('',*,*,#23454,.F.);
#31348=ORIENTED_EDGE('',*,*,#23455,.F.);
#31349=ORIENTED_EDGE('',*,*,#23456,.F.);
#31350=ORIENTED_EDGE('',*,*,#23457,.F.);
#31351=ORIENTED_EDGE('',*,*,#23458,.F.);
#31352=ORIENTED_EDGE('',*,*,#23459,.F.);
#31353=ORIENTED_EDGE('',*,*,#23460,.F.);
#31354=ORIENTED_EDGE('',*,*,#23461,.F.);
#31355=ORIENTED_EDGE('',*,*,#23462,.F.);
#31356=ORIENTED_EDGE('',*,*,#23463,.F.);
#31357=ORIENTED_EDGE('',*,*,#23464,.F.);
#31358=ORIENTED_EDGE('',*,*,#23465,.F.);
#31359=ORIENTED_EDGE('',*,*,#23466,.F.);
#31360=ORIENTED_EDGE('',*,*,#23467,.F.);
#31361=ORIENTED_EDGE('',*,*,#23468,.F.);
#31362=ORIENTED_EDGE('',*,*,#23469,.F.);
#31363=ORIENTED_EDGE('',*,*,#23470,.F.);
#31364=ORIENTED_EDGE('',*,*,#23471,.F.);
#31365=ORIENTED_EDGE('',*,*,#23472,.F.);
#31366=ORIENTED_EDGE('',*,*,#23473,.F.);
#31367=ORIENTED_EDGE('',*,*,#23474,.F.);
#31368=ORIENTED_EDGE('',*,*,#23475,.F.);
#31369=ORIENTED_EDGE('',*,*,#23476,.F.);
#31370=ORIENTED_EDGE('',*,*,#23477,.F.);
#31371=ORIENTED_EDGE('',*,*,#23478,.F.);
#31372=ORIENTED_EDGE('',*,*,#23479,.F.);
#31373=ORIENTED_EDGE('',*,*,#23480,.F.);
#31374=ORIENTED_EDGE('',*,*,#23481,.F.);
#31375=ORIENTED_EDGE('',*,*,#23482,.F.);
#31376=ORIENTED_EDGE('',*,*,#23483,.F.);
#31377=ORIENTED_EDGE('',*,*,#23484,.F.);
#31378=ORIENTED_EDGE('',*,*,#23485,.F.);
#31379=ORIENTED_EDGE('',*,*,#23486,.F.);
#31380=ORIENTED_EDGE('',*,*,#23487,.F.);
#31381=ORIENTED_EDGE('',*,*,#23488,.F.);
#31382=ORIENTED_EDGE('',*,*,#23489,.F.);
#31383=ORIENTED_EDGE('',*,*,#23490,.F.);
#31384=ORIENTED_EDGE('',*,*,#23491,.F.);
#31385=ORIENTED_EDGE('',*,*,#23492,.F.);
#31386=ORIENTED_EDGE('',*,*,#23493,.F.);
#31387=ORIENTED_EDGE('',*,*,#23494,.F.);
#31388=ORIENTED_EDGE('',*,*,#23495,.F.);
#31389=ORIENTED_EDGE('',*,*,#23496,.F.);
#31390=ORIENTED_EDGE('',*,*,#23497,.F.);
#31391=ORIENTED_EDGE('',*,*,#23498,.F.);
#31392=ORIENTED_EDGE('',*,*,#23499,.F.);
#31393=ORIENTED_EDGE('',*,*,#23500,.F.);
#31394=ORIENTED_EDGE('',*,*,#23501,.F.);
#31395=ORIENTED_EDGE('',*,*,#23502,.F.);
#31396=ORIENTED_EDGE('',*,*,#23503,.F.);
#31397=ORIENTED_EDGE('',*,*,#23504,.F.);
#31398=ORIENTED_EDGE('',*,*,#23505,.F.);
#31399=ORIENTED_EDGE('',*,*,#23506,.F.);
#31400=ORIENTED_EDGE('',*,*,#23507,.F.);
#31401=ORIENTED_EDGE('',*,*,#23508,.F.);
#31402=ORIENTED_EDGE('',*,*,#23509,.F.);
#31403=ORIENTED_EDGE('',*,*,#23510,.F.);
#31404=ORIENTED_EDGE('',*,*,#23511,.F.);
#31405=ORIENTED_EDGE('',*,*,#23512,.F.);
#31406=ORIENTED_EDGE('',*,*,#23513,.F.);
#31407=ORIENTED_EDGE('',*,*,#23514,.F.);
#31408=ORIENTED_EDGE('',*,*,#23515,.F.);
#31409=ORIENTED_EDGE('',*,*,#23516,.F.);
#31410=ORIENTED_EDGE('',*,*,#23517,.F.);
#31411=ORIENTED_EDGE('',*,*,#23518,.F.);
#31412=ORIENTED_EDGE('',*,*,#23519,.F.);
#31413=ORIENTED_EDGE('',*,*,#23520,.F.);
#31414=ORIENTED_EDGE('',*,*,#23521,.F.);
#31415=ORIENTED_EDGE('',*,*,#23522,.F.);
#31416=ORIENTED_EDGE('',*,*,#23523,.F.);
#31417=ORIENTED_EDGE('',*,*,#23524,.F.);
#31418=ORIENTED_EDGE('',*,*,#23525,.F.);
#31419=ORIENTED_EDGE('',*,*,#23526,.F.);
#31420=ORIENTED_EDGE('',*,*,#23527,.F.);
#31421=ORIENTED_EDGE('',*,*,#23528,.F.);
#31422=ORIENTED_EDGE('',*,*,#23529,.F.);
#31423=ORIENTED_EDGE('',*,*,#23530,.F.);
#31424=ORIENTED_EDGE('',*,*,#23531,.F.);
#31425=ORIENTED_EDGE('',*,*,#23532,.F.);
#31426=ORIENTED_EDGE('',*,*,#23533,.F.);
#31427=ORIENTED_EDGE('',*,*,#23534,.F.);
#31428=ORIENTED_EDGE('',*,*,#23535,.F.);
#31429=ORIENTED_EDGE('',*,*,#23536,.F.);
#31430=ORIENTED_EDGE('',*,*,#23537,.F.);
#31431=ORIENTED_EDGE('',*,*,#23538,.F.);
#31432=ORIENTED_EDGE('',*,*,#23539,.F.);
#31433=ORIENTED_EDGE('',*,*,#23540,.F.);
#31434=ORIENTED_EDGE('',*,*,#23541,.F.);
#31435=ORIENTED_EDGE('',*,*,#23542,.F.);
#31436=ORIENTED_EDGE('',*,*,#23543,.F.);
#31437=ORIENTED_EDGE('',*,*,#23544,.F.);
#31438=ORIENTED_EDGE('',*,*,#23545,.F.);
#31439=ORIENTED_EDGE('',*,*,#23546,.F.);
#31440=ORIENTED_EDGE('',*,*,#23547,.F.);
#31441=ORIENTED_EDGE('',*,*,#23548,.F.);
#31442=ORIENTED_EDGE('',*,*,#23549,.F.);
#31443=ORIENTED_EDGE('',*,*,#23550,.F.);
#31444=ORIENTED_EDGE('',*,*,#23551,.F.);
#31445=ORIENTED_EDGE('',*,*,#23552,.F.);
#31446=ORIENTED_EDGE('',*,*,#23553,.F.);
#31447=ORIENTED_EDGE('',*,*,#23554,.F.);
#31448=ORIENTED_EDGE('',*,*,#23555,.F.);
#31449=ORIENTED_EDGE('',*,*,#23556,.F.);
#31450=ORIENTED_EDGE('',*,*,#23557,.F.);
#31451=ORIENTED_EDGE('',*,*,#23558,.F.);
#31452=ORIENTED_EDGE('',*,*,#23559,.F.);
#31453=ORIENTED_EDGE('',*,*,#23560,.F.);
#31454=ORIENTED_EDGE('',*,*,#23561,.F.);
#31455=ORIENTED_EDGE('',*,*,#23562,.F.);
#31456=ORIENTED_EDGE('',*,*,#23563,.F.);
#31457=ORIENTED_EDGE('',*,*,#23564,.F.);
#31458=ORIENTED_EDGE('',*,*,#23565,.F.);
#31459=ORIENTED_EDGE('',*,*,#23566,.F.);
#31460=ORIENTED_EDGE('',*,*,#23567,.F.);
#31461=ORIENTED_EDGE('',*,*,#23568,.F.);
#31462=ORIENTED_EDGE('',*,*,#23569,.F.);
#31463=ORIENTED_EDGE('',*,*,#23570,.F.);
#31464=ORIENTED_EDGE('',*,*,#23571,.F.);
#31465=ORIENTED_EDGE('',*,*,#23572,.F.);
#31466=ORIENTED_EDGE('',*,*,#23573,.F.);
#31467=ORIENTED_EDGE('',*,*,#23574,.F.);
#31468=ORIENTED_EDGE('',*,*,#23575,.F.);
#31469=ORIENTED_EDGE('',*,*,#23576,.F.);
#31470=ORIENTED_EDGE('',*,*,#23577,.F.);
#31471=ORIENTED_EDGE('',*,*,#23578,.F.);
#31472=ORIENTED_EDGE('',*,*,#23579,.F.);
#31473=ORIENTED_EDGE('',*,*,#23580,.F.);
#31474=ORIENTED_EDGE('',*,*,#23581,.F.);
#31475=ORIENTED_EDGE('',*,*,#23582,.F.);
#31476=ORIENTED_EDGE('',*,*,#23583,.F.);
#31477=ORIENTED_EDGE('',*,*,#23584,.F.);
#31478=ORIENTED_EDGE('',*,*,#23585,.F.);
#31479=ORIENTED_EDGE('',*,*,#23586,.F.);
#31480=ORIENTED_EDGE('',*,*,#23587,.F.);
#31481=ORIENTED_EDGE('',*,*,#23588,.F.);
#31482=ORIENTED_EDGE('',*,*,#23589,.F.);
#31483=ORIENTED_EDGE('',*,*,#23590,.F.);
#31484=ORIENTED_EDGE('',*,*,#23591,.F.);
#31485=ORIENTED_EDGE('',*,*,#23592,.F.);
#31486=ORIENTED_EDGE('',*,*,#23593,.F.);
#31487=ORIENTED_EDGE('',*,*,#23594,.F.);
#31488=ORIENTED_EDGE('',*,*,#23595,.F.);
#31489=ORIENTED_EDGE('',*,*,#23596,.F.);
#31490=ORIENTED_EDGE('',*,*,#23597,.F.);
#31491=ORIENTED_EDGE('',*,*,#23598,.F.);
#31492=ORIENTED_EDGE('',*,*,#23599,.F.);
#31493=ORIENTED_EDGE('',*,*,#23600,.F.);
#31494=ORIENTED_EDGE('',*,*,#23601,.F.);
#31495=ORIENTED_EDGE('',*,*,#23602,.F.);
#31496=ORIENTED_EDGE('',*,*,#23603,.F.);
#31497=ORIENTED_EDGE('',*,*,#23604,.F.);
#31498=ORIENTED_EDGE('',*,*,#23605,.F.);
#31499=ORIENTED_EDGE('',*,*,#23606,.F.);
#31500=ORIENTED_EDGE('',*,*,#23607,.F.);
#31501=ORIENTED_EDGE('',*,*,#23608,.F.);
#31502=ORIENTED_EDGE('',*,*,#23609,.F.);
#31503=ORIENTED_EDGE('',*,*,#23610,.F.);
#31504=ORIENTED_EDGE('',*,*,#23611,.F.);
#31505=ORIENTED_EDGE('',*,*,#23612,.F.);
#31506=ORIENTED_EDGE('',*,*,#23613,.F.);
#31507=ORIENTED_EDGE('',*,*,#23614,.F.);
#31508=ORIENTED_EDGE('',*,*,#23615,.F.);
#31509=ORIENTED_EDGE('',*,*,#23616,.F.);
#31510=ORIENTED_EDGE('',*,*,#23617,.F.);
#31511=ORIENTED_EDGE('',*,*,#23618,.F.);
#31512=ORIENTED_EDGE('',*,*,#23619,.F.);
#31513=ORIENTED_EDGE('',*,*,#23620,.F.);
#31514=ORIENTED_EDGE('',*,*,#23621,.F.);
#31515=ORIENTED_EDGE('',*,*,#23622,.F.);
#31516=ORIENTED_EDGE('',*,*,#23623,.F.);
#31517=ORIENTED_EDGE('',*,*,#23624,.F.);
#31518=ORIENTED_EDGE('',*,*,#23625,.F.);
#31519=ORIENTED_EDGE('',*,*,#23626,.F.);
#31520=ORIENTED_EDGE('',*,*,#23627,.F.);
#31521=ORIENTED_EDGE('',*,*,#23628,.F.);
#31522=ORIENTED_EDGE('',*,*,#23629,.F.);
#31523=ORIENTED_EDGE('',*,*,#23630,.F.);
#31524=ORIENTED_EDGE('',*,*,#23631,.F.);
#31525=ORIENTED_EDGE('',*,*,#23632,.F.);
#31526=ORIENTED_EDGE('',*,*,#23633,.F.);
#31527=ORIENTED_EDGE('',*,*,#23634,.F.);
#31528=ORIENTED_EDGE('',*,*,#23635,.F.);
#31529=ORIENTED_EDGE('',*,*,#23636,.F.);
#31530=ORIENTED_EDGE('',*,*,#23637,.F.);
#31531=ORIENTED_EDGE('',*,*,#23638,.F.);
#31532=ORIENTED_EDGE('',*,*,#23639,.F.);
#31533=ORIENTED_EDGE('',*,*,#23640,.F.);
#31534=ORIENTED_EDGE('',*,*,#23641,.F.);
#31535=ORIENTED_EDGE('',*,*,#23642,.F.);
#31536=ORIENTED_EDGE('',*,*,#23643,.F.);
#31537=ORIENTED_EDGE('',*,*,#23644,.F.);
#31538=ORIENTED_EDGE('',*,*,#23645,.F.);
#31539=ORIENTED_EDGE('',*,*,#23646,.F.);
#31540=ORIENTED_EDGE('',*,*,#23647,.F.);
#31541=ORIENTED_EDGE('',*,*,#23648,.F.);
#31542=ORIENTED_EDGE('',*,*,#23649,.F.);
#31543=ORIENTED_EDGE('',*,*,#23650,.F.);
#31544=ORIENTED_EDGE('',*,*,#23651,.F.);
#31545=ORIENTED_EDGE('',*,*,#23652,.F.);
#31546=ORIENTED_EDGE('',*,*,#23653,.F.);
#31547=ORIENTED_EDGE('',*,*,#23654,.F.);
#31548=ORIENTED_EDGE('',*,*,#23655,.F.);
#31549=ORIENTED_EDGE('',*,*,#23656,.F.);
#31550=ORIENTED_EDGE('',*,*,#23657,.F.);
#31551=ORIENTED_EDGE('',*,*,#23658,.F.);
#31552=ORIENTED_EDGE('',*,*,#23659,.F.);
#31553=ORIENTED_EDGE('',*,*,#23660,.F.);
#31554=ORIENTED_EDGE('',*,*,#23661,.F.);
#31555=ORIENTED_EDGE('',*,*,#23662,.F.);
#31556=ORIENTED_EDGE('',*,*,#23663,.F.);
#31557=ORIENTED_EDGE('',*,*,#23664,.F.);
#31558=ORIENTED_EDGE('',*,*,#23665,.F.);
#31559=ORIENTED_EDGE('',*,*,#23666,.F.);
#31560=ORIENTED_EDGE('',*,*,#23667,.F.);
#31561=ORIENTED_EDGE('',*,*,#23668,.F.);
#31562=ORIENTED_EDGE('',*,*,#23669,.F.);
#31563=ORIENTED_EDGE('',*,*,#23670,.F.);
#31564=ORIENTED_EDGE('',*,*,#23671,.F.);
#31565=ORIENTED_EDGE('',*,*,#23672,.F.);
#31566=ORIENTED_EDGE('',*,*,#23673,.F.);
#31567=ORIENTED_EDGE('',*,*,#23674,.F.);
#31568=ORIENTED_EDGE('',*,*,#23675,.F.);
#31569=ORIENTED_EDGE('',*,*,#23676,.F.);
#31570=ORIENTED_EDGE('',*,*,#23677,.F.);
#31571=ORIENTED_EDGE('',*,*,#23678,.F.);
#31572=ORIENTED_EDGE('',*,*,#23679,.F.);
#31573=ORIENTED_EDGE('',*,*,#23680,.F.);
#31574=ORIENTED_EDGE('',*,*,#23681,.F.);
#31575=ORIENTED_EDGE('',*,*,#23682,.F.);
#31576=ORIENTED_EDGE('',*,*,#23683,.F.);
#31577=ORIENTED_EDGE('',*,*,#23684,.F.);
#31578=ORIENTED_EDGE('',*,*,#23685,.F.);
#31579=ORIENTED_EDGE('',*,*,#23686,.F.);
#31580=ORIENTED_EDGE('',*,*,#23687,.F.);
#31581=ORIENTED_EDGE('',*,*,#23688,.F.);
#31582=ORIENTED_EDGE('',*,*,#23689,.F.);
#31583=ORIENTED_EDGE('',*,*,#23690,.F.);
#31584=ORIENTED_EDGE('',*,*,#23691,.F.);
#31585=ORIENTED_EDGE('',*,*,#23692,.F.);
#31586=ORIENTED_EDGE('',*,*,#23693,.F.);
#31587=ORIENTED_EDGE('',*,*,#23694,.F.);
#31588=ORIENTED_EDGE('',*,*,#23695,.F.);
#31589=ORIENTED_EDGE('',*,*,#23696,.F.);
#31590=ORIENTED_EDGE('',*,*,#23697,.F.);
#31591=ORIENTED_EDGE('',*,*,#23698,.F.);
#31592=ORIENTED_EDGE('',*,*,#23699,.F.);
#31593=ORIENTED_EDGE('',*,*,#23700,.F.);
#31594=ORIENTED_EDGE('',*,*,#23701,.F.);
#31595=ORIENTED_EDGE('',*,*,#23702,.F.);
#31596=ORIENTED_EDGE('',*,*,#23703,.F.);
#31597=ORIENTED_EDGE('',*,*,#23704,.F.);
#31598=ORIENTED_EDGE('',*,*,#23705,.F.);
#31599=ORIENTED_EDGE('',*,*,#23706,.F.);
#31600=ORIENTED_EDGE('',*,*,#23707,.F.);
#31601=ORIENTED_EDGE('',*,*,#23708,.F.);
#31602=ORIENTED_EDGE('',*,*,#23709,.F.);
#31603=ORIENTED_EDGE('',*,*,#23710,.F.);
#31604=ORIENTED_EDGE('',*,*,#23711,.F.);
#31605=ORIENTED_EDGE('',*,*,#23712,.F.);
#31606=ORIENTED_EDGE('',*,*,#23713,.F.);
#31607=ORIENTED_EDGE('',*,*,#23714,.F.);
#31608=ORIENTED_EDGE('',*,*,#23715,.F.);
#31609=ORIENTED_EDGE('',*,*,#23716,.F.);
#31610=ORIENTED_EDGE('',*,*,#23717,.F.);
#31611=ORIENTED_EDGE('',*,*,#23718,.F.);
#31612=ORIENTED_EDGE('',*,*,#23719,.F.);
#31613=ORIENTED_EDGE('',*,*,#23720,.F.);
#31614=ORIENTED_EDGE('',*,*,#23721,.F.);
#31615=ORIENTED_EDGE('',*,*,#23722,.F.);
#31616=ORIENTED_EDGE('',*,*,#23723,.F.);
#31617=ORIENTED_EDGE('',*,*,#23724,.F.);
#31618=ORIENTED_EDGE('',*,*,#23725,.F.);
#31619=ORIENTED_EDGE('',*,*,#23726,.F.);
#31620=ORIENTED_EDGE('',*,*,#23727,.F.);
#31621=ORIENTED_EDGE('',*,*,#23728,.F.);
#31622=ORIENTED_EDGE('',*,*,#23729,.F.);
#31623=ORIENTED_EDGE('',*,*,#23730,.F.);
#31624=ORIENTED_EDGE('',*,*,#23731,.F.);
#31625=ORIENTED_EDGE('',*,*,#23732,.F.);
#31626=ORIENTED_EDGE('',*,*,#23733,.F.);
#31627=ORIENTED_EDGE('',*,*,#23734,.F.);
#31628=ORIENTED_EDGE('',*,*,#23735,.F.);
#31629=ORIENTED_EDGE('',*,*,#23736,.F.);
#31630=ORIENTED_EDGE('',*,*,#23737,.F.);
#31631=ORIENTED_EDGE('',*,*,#23738,.F.);
#31632=ORIENTED_EDGE('',*,*,#23739,.F.);
#31633=ORIENTED_EDGE('',*,*,#23740,.F.);
#31634=ORIENTED_EDGE('',*,*,#23741,.F.);
#31635=ORIENTED_EDGE('',*,*,#23742,.F.);
#31636=ORIENTED_EDGE('',*,*,#23743,.F.);
#31637=ORIENTED_EDGE('',*,*,#23744,.F.);
#31638=ORIENTED_EDGE('',*,*,#23745,.F.);
#31639=ORIENTED_EDGE('',*,*,#23746,.F.);
#31640=ORIENTED_EDGE('',*,*,#23747,.F.);
#31641=ORIENTED_EDGE('',*,*,#23748,.F.);
#31642=ORIENTED_EDGE('',*,*,#23749,.F.);
#31643=ORIENTED_EDGE('',*,*,#23750,.F.);
#31644=ORIENTED_EDGE('',*,*,#23751,.F.);
#31645=ORIENTED_EDGE('',*,*,#23752,.F.);
#31646=ORIENTED_EDGE('',*,*,#23753,.F.);
#31647=ORIENTED_EDGE('',*,*,#23754,.F.);
#31648=ORIENTED_EDGE('',*,*,#23755,.F.);
#31649=ORIENTED_EDGE('',*,*,#23756,.F.);
#31650=ORIENTED_EDGE('',*,*,#23757,.F.);
#31651=ORIENTED_EDGE('',*,*,#23758,.F.);
#31652=ORIENTED_EDGE('',*,*,#23759,.F.);
#31653=ORIENTED_EDGE('',*,*,#23760,.F.);
#31654=ORIENTED_EDGE('',*,*,#23761,.F.);
#31655=ORIENTED_EDGE('',*,*,#23762,.F.);
#31656=ORIENTED_EDGE('',*,*,#23763,.F.);
#31657=ORIENTED_EDGE('',*,*,#23764,.F.);
#31658=ORIENTED_EDGE('',*,*,#23765,.F.);
#31659=ORIENTED_EDGE('',*,*,#23766,.F.);
#31660=ORIENTED_EDGE('',*,*,#23767,.F.);
#31661=ORIENTED_EDGE('',*,*,#23768,.F.);
#31662=ORIENTED_EDGE('',*,*,#23769,.F.);
#31663=ORIENTED_EDGE('',*,*,#23770,.F.);
#31664=ORIENTED_EDGE('',*,*,#23771,.F.);
#31665=ORIENTED_EDGE('',*,*,#23772,.F.);
#31666=ORIENTED_EDGE('',*,*,#23773,.F.);
#31667=ORIENTED_EDGE('',*,*,#23774,.F.);
#31668=ORIENTED_EDGE('',*,*,#23775,.F.);
#31669=ORIENTED_EDGE('',*,*,#23776,.F.);
#31670=ORIENTED_EDGE('',*,*,#23777,.F.);
#31671=ORIENTED_EDGE('',*,*,#23778,.F.);
#31672=ORIENTED_EDGE('',*,*,#23779,.F.);
#31673=ORIENTED_EDGE('',*,*,#23780,.F.);
#31674=ORIENTED_EDGE('',*,*,#23781,.F.);
#31675=ORIENTED_EDGE('',*,*,#23782,.F.);
#31676=ORIENTED_EDGE('',*,*,#23783,.F.);
#31677=ORIENTED_EDGE('',*,*,#23784,.F.);
#31678=ORIENTED_EDGE('',*,*,#23785,.F.);
#31679=ORIENTED_EDGE('',*,*,#23786,.F.);
#31680=ORIENTED_EDGE('',*,*,#23787,.F.);
#31681=ORIENTED_EDGE('',*,*,#23788,.F.);
#31682=ORIENTED_EDGE('',*,*,#23789,.F.);
#31683=ORIENTED_EDGE('',*,*,#23790,.F.);
#31684=ORIENTED_EDGE('',*,*,#23791,.F.);
#31685=ORIENTED_EDGE('',*,*,#23792,.F.);
#31686=ORIENTED_EDGE('',*,*,#23793,.F.);
#31687=ORIENTED_EDGE('',*,*,#23794,.F.);
#31688=ORIENTED_EDGE('',*,*,#23795,.F.);
#31689=ORIENTED_EDGE('',*,*,#23796,.F.);
#31690=ORIENTED_EDGE('',*,*,#23797,.F.);
#31691=ORIENTED_EDGE('',*,*,#23798,.F.);
#31692=ORIENTED_EDGE('',*,*,#23799,.F.);
#31693=ORIENTED_EDGE('',*,*,#23800,.F.);
#31694=ORIENTED_EDGE('',*,*,#23801,.F.);
#31695=ORIENTED_EDGE('',*,*,#23802,.F.);
#31696=ORIENTED_EDGE('',*,*,#23803,.F.);
#31697=ORIENTED_EDGE('',*,*,#23804,.F.);
#31698=ORIENTED_EDGE('',*,*,#23805,.F.);
#31699=ORIENTED_EDGE('',*,*,#23806,.F.);
#31700=ORIENTED_EDGE('',*,*,#23807,.F.);
#31701=ORIENTED_EDGE('',*,*,#23808,.F.);
#31702=ORIENTED_EDGE('',*,*,#23809,.F.);
#31703=ORIENTED_EDGE('',*,*,#23810,.F.);
#31704=ORIENTED_EDGE('',*,*,#23811,.F.);
#31705=ORIENTED_EDGE('',*,*,#23812,.F.);
#31706=ORIENTED_EDGE('',*,*,#23813,.F.);
#31707=ORIENTED_EDGE('',*,*,#23814,.F.);
#31708=ORIENTED_EDGE('',*,*,#23815,.F.);
#31709=ORIENTED_EDGE('',*,*,#23816,.F.);
#31710=ORIENTED_EDGE('',*,*,#23817,.F.);
#31711=ORIENTED_EDGE('',*,*,#23818,.F.);
#31712=ORIENTED_EDGE('',*,*,#23819,.F.);
#31713=ORIENTED_EDGE('',*,*,#23820,.F.);
#31714=ORIENTED_EDGE('',*,*,#23821,.F.);
#31715=ORIENTED_EDGE('',*,*,#23822,.F.);
#31716=ORIENTED_EDGE('',*,*,#23823,.F.);
#31717=ORIENTED_EDGE('',*,*,#23824,.F.);
#31718=ORIENTED_EDGE('',*,*,#23825,.F.);
#31719=ORIENTED_EDGE('',*,*,#23826,.F.);
#31720=ORIENTED_EDGE('',*,*,#23827,.F.);
#31721=ORIENTED_EDGE('',*,*,#23828,.F.);
#31722=ORIENTED_EDGE('',*,*,#23829,.F.);
#31723=ORIENTED_EDGE('',*,*,#23830,.F.);
#31724=ORIENTED_EDGE('',*,*,#23831,.F.);
#31725=ORIENTED_EDGE('',*,*,#23832,.F.);
#31726=ORIENTED_EDGE('',*,*,#23833,.F.);
#31727=ORIENTED_EDGE('',*,*,#23834,.F.);
#31728=ORIENTED_EDGE('',*,*,#23835,.F.);
#31729=ORIENTED_EDGE('',*,*,#23836,.F.);
#31730=ORIENTED_EDGE('',*,*,#23837,.F.);
#31731=ORIENTED_EDGE('',*,*,#23838,.F.);
#31732=ORIENTED_EDGE('',*,*,#23839,.F.);
#31733=ORIENTED_EDGE('',*,*,#23840,.F.);
#31734=ORIENTED_EDGE('',*,*,#23841,.F.);
#31735=ORIENTED_EDGE('',*,*,#23842,.F.);
#31736=ORIENTED_EDGE('',*,*,#23843,.F.);
#31737=ORIENTED_EDGE('',*,*,#23844,.F.);
#31738=ORIENTED_EDGE('',*,*,#23845,.F.);
#31739=ORIENTED_EDGE('',*,*,#23846,.F.);
#31740=ORIENTED_EDGE('',*,*,#23847,.F.);
#31741=ORIENTED_EDGE('',*,*,#23848,.F.);
#31742=ORIENTED_EDGE('',*,*,#23849,.F.);
#31743=ORIENTED_EDGE('',*,*,#23850,.F.);
#31744=ORIENTED_EDGE('',*,*,#23851,.F.);
#31745=ORIENTED_EDGE('',*,*,#23852,.F.);
#31746=ORIENTED_EDGE('',*,*,#23853,.F.);
#31747=ORIENTED_EDGE('',*,*,#23854,.F.);
#31748=ORIENTED_EDGE('',*,*,#23855,.F.);
#31749=ORIENTED_EDGE('',*,*,#23856,.F.);
#31750=ORIENTED_EDGE('',*,*,#23857,.F.);
#31751=ORIENTED_EDGE('',*,*,#23858,.F.);
#31752=ORIENTED_EDGE('',*,*,#23859,.F.);
#31753=ORIENTED_EDGE('',*,*,#23860,.F.);
#31754=ORIENTED_EDGE('',*,*,#23861,.F.);
#31755=ORIENTED_EDGE('',*,*,#23862,.F.);
#31756=ORIENTED_EDGE('',*,*,#23863,.F.);
#31757=ORIENTED_EDGE('',*,*,#23864,.F.);
#31758=ORIENTED_EDGE('',*,*,#23865,.F.);
#31759=ORIENTED_EDGE('',*,*,#23866,.F.);
#31760=ORIENTED_EDGE('',*,*,#23867,.F.);
#31761=ORIENTED_EDGE('',*,*,#23868,.F.);
#31762=ORIENTED_EDGE('',*,*,#23869,.F.);
#31763=ORIENTED_EDGE('',*,*,#23870,.F.);
#31764=ORIENTED_EDGE('',*,*,#23871,.F.);
#31765=ORIENTED_EDGE('',*,*,#23872,.F.);
#31766=ORIENTED_EDGE('',*,*,#23873,.F.);
#31767=ORIENTED_EDGE('',*,*,#23874,.F.);
#31768=ORIENTED_EDGE('',*,*,#23875,.F.);
#31769=ORIENTED_EDGE('',*,*,#23876,.F.);
#31770=ORIENTED_EDGE('',*,*,#23877,.F.);
#31771=ORIENTED_EDGE('',*,*,#23878,.F.);
#31772=ORIENTED_EDGE('',*,*,#23879,.F.);
#31773=ORIENTED_EDGE('',*,*,#23880,.F.);
#31774=ORIENTED_EDGE('',*,*,#23881,.F.);
#31775=ORIENTED_EDGE('',*,*,#23882,.F.);
#31776=ORIENTED_EDGE('',*,*,#23883,.F.);
#31777=ORIENTED_EDGE('',*,*,#23884,.F.);
#31778=ORIENTED_EDGE('',*,*,#23885,.F.);
#31779=ORIENTED_EDGE('',*,*,#23886,.F.);
#31780=ORIENTED_EDGE('',*,*,#23887,.F.);
#31781=ORIENTED_EDGE('',*,*,#23888,.F.);
#31782=ORIENTED_EDGE('',*,*,#23889,.F.);
#31783=ORIENTED_EDGE('',*,*,#23890,.F.);
#31784=ORIENTED_EDGE('',*,*,#23891,.F.);
#31785=ORIENTED_EDGE('',*,*,#23892,.F.);
#31786=ORIENTED_EDGE('',*,*,#23893,.F.);
#31787=ORIENTED_EDGE('',*,*,#23894,.F.);
#31788=ORIENTED_EDGE('',*,*,#23895,.F.);
#31789=ORIENTED_EDGE('',*,*,#23896,.F.);
#31790=ORIENTED_EDGE('',*,*,#23897,.F.);
#31791=ORIENTED_EDGE('',*,*,#23898,.F.);
#31792=ORIENTED_EDGE('',*,*,#23899,.F.);
#31793=ORIENTED_EDGE('',*,*,#23900,.F.);
#31794=ORIENTED_EDGE('',*,*,#23901,.F.);
#31795=ORIENTED_EDGE('',*,*,#23902,.F.);
#31796=ORIENTED_EDGE('',*,*,#23903,.F.);
#31797=ORIENTED_EDGE('',*,*,#23904,.F.);
#31798=ORIENTED_EDGE('',*,*,#23905,.F.);
#31799=ORIENTED_EDGE('',*,*,#23906,.F.);
#31800=ORIENTED_EDGE('',*,*,#23907,.F.);
#31801=ORIENTED_EDGE('',*,*,#23908,.F.);
#31802=ORIENTED_EDGE('',*,*,#23909,.F.);
#31803=ORIENTED_EDGE('',*,*,#23910,.F.);
#31804=ORIENTED_EDGE('',*,*,#23911,.F.);
#31805=ORIENTED_EDGE('',*,*,#23912,.F.);
#31806=ORIENTED_EDGE('',*,*,#23913,.F.);
#31807=ORIENTED_EDGE('',*,*,#23914,.F.);
#31808=ORIENTED_EDGE('',*,*,#23915,.F.);
#31809=ORIENTED_EDGE('',*,*,#23916,.F.);
#31810=ORIENTED_EDGE('',*,*,#23917,.F.);
#31811=ORIENTED_EDGE('',*,*,#23918,.F.);
#31812=ORIENTED_EDGE('',*,*,#23919,.F.);
#31813=ORIENTED_EDGE('',*,*,#23920,.F.);
#31814=ORIENTED_EDGE('',*,*,#23921,.F.);
#31815=ORIENTED_EDGE('',*,*,#23922,.F.);
#31816=ORIENTED_EDGE('',*,*,#23923,.F.);
#31817=ORIENTED_EDGE('',*,*,#23924,.F.);
#31818=ORIENTED_EDGE('',*,*,#23925,.F.);
#31819=ORIENTED_EDGE('',*,*,#23926,.F.);
#31820=ORIENTED_EDGE('',*,*,#23927,.F.);
#31821=ORIENTED_EDGE('',*,*,#23928,.F.);
#31822=ORIENTED_EDGE('',*,*,#23929,.F.);
#31823=ORIENTED_EDGE('',*,*,#23930,.F.);
#31824=ORIENTED_EDGE('',*,*,#23931,.F.);
#31825=ORIENTED_EDGE('',*,*,#23932,.F.);
#31826=ORIENTED_EDGE('',*,*,#23933,.F.);
#31827=ORIENTED_EDGE('',*,*,#23934,.F.);
#31828=ORIENTED_EDGE('',*,*,#23935,.F.);
#31829=ORIENTED_EDGE('',*,*,#23936,.F.);
#31830=ORIENTED_EDGE('',*,*,#23937,.F.);
#31831=ORIENTED_EDGE('',*,*,#23938,.F.);
#31832=ORIENTED_EDGE('',*,*,#23939,.F.);
#31833=ORIENTED_EDGE('',*,*,#23940,.F.);
#31834=ORIENTED_EDGE('',*,*,#23941,.F.);
#31835=ORIENTED_EDGE('',*,*,#23942,.F.);
#31836=ORIENTED_EDGE('',*,*,#23943,.F.);
#31837=ORIENTED_EDGE('',*,*,#23944,.F.);
#31838=ORIENTED_EDGE('',*,*,#23945,.F.);
#31839=ORIENTED_EDGE('',*,*,#23946,.F.);
#31840=ORIENTED_EDGE('',*,*,#23947,.F.);
#31841=ORIENTED_EDGE('',*,*,#23948,.F.);
#31842=ORIENTED_EDGE('',*,*,#23949,.F.);
#31843=ORIENTED_EDGE('',*,*,#23950,.F.);
#31844=ORIENTED_EDGE('',*,*,#23951,.F.);
#31845=ORIENTED_EDGE('',*,*,#23952,.F.);
#31846=ORIENTED_EDGE('',*,*,#23953,.F.);
#31847=ORIENTED_EDGE('',*,*,#23954,.F.);
#31848=ORIENTED_EDGE('',*,*,#23955,.F.);
#31849=ORIENTED_EDGE('',*,*,#23956,.F.);
#31850=ORIENTED_EDGE('',*,*,#23957,.F.);
#31851=ORIENTED_EDGE('',*,*,#23958,.F.);
#31852=ORIENTED_EDGE('',*,*,#23959,.F.);
#31853=ORIENTED_EDGE('',*,*,#23960,.F.);
#31854=ORIENTED_EDGE('',*,*,#23961,.F.);
#31855=ORIENTED_EDGE('',*,*,#23962,.F.);
#31856=ORIENTED_EDGE('',*,*,#23963,.F.);
#31857=ORIENTED_EDGE('',*,*,#23964,.F.);
#31858=ORIENTED_EDGE('',*,*,#23965,.F.);
#31859=ORIENTED_EDGE('',*,*,#23966,.F.);
#31860=ORIENTED_EDGE('',*,*,#23967,.F.);
#31861=ORIENTED_EDGE('',*,*,#23968,.F.);
#31862=ORIENTED_EDGE('',*,*,#23969,.F.);
#31863=ORIENTED_EDGE('',*,*,#23970,.F.);
#31864=ORIENTED_EDGE('',*,*,#23971,.F.);
#31865=ORIENTED_EDGE('',*,*,#23972,.F.);
#31866=ORIENTED_EDGE('',*,*,#23973,.F.);
#31867=ORIENTED_EDGE('',*,*,#23974,.F.);
#31868=ORIENTED_EDGE('',*,*,#23975,.F.);
#31869=ORIENTED_EDGE('',*,*,#23976,.F.);
#31870=ORIENTED_EDGE('',*,*,#23977,.F.);
#31871=ORIENTED_EDGE('',*,*,#23978,.F.);
#31872=ORIENTED_EDGE('',*,*,#23979,.F.);
#31873=ORIENTED_EDGE('',*,*,#23980,.F.);
#31874=ORIENTED_EDGE('',*,*,#23981,.F.);
#31875=ORIENTED_EDGE('',*,*,#23982,.F.);
#31876=ORIENTED_EDGE('',*,*,#23983,.F.);
#31877=ORIENTED_EDGE('',*,*,#23984,.F.);
#31878=ORIENTED_EDGE('',*,*,#23985,.F.);
#31879=ORIENTED_EDGE('',*,*,#23986,.F.);
#31880=ORIENTED_EDGE('',*,*,#23987,.F.);
#31881=ORIENTED_EDGE('',*,*,#23988,.F.);
#31882=ORIENTED_EDGE('',*,*,#23989,.F.);
#31883=ORIENTED_EDGE('',*,*,#23990,.F.);
#31884=ORIENTED_EDGE('',*,*,#23991,.F.);
#31885=ORIENTED_EDGE('',*,*,#23992,.F.);
#31886=ORIENTED_EDGE('',*,*,#23993,.F.);
#31887=ORIENTED_EDGE('',*,*,#23994,.F.);
#31888=ORIENTED_EDGE('',*,*,#23995,.F.);
#31889=ORIENTED_EDGE('',*,*,#23996,.F.);
#31890=ORIENTED_EDGE('',*,*,#23997,.F.);
#31891=ORIENTED_EDGE('',*,*,#23998,.F.);
#31892=ORIENTED_EDGE('',*,*,#23999,.F.);
#31893=ORIENTED_EDGE('',*,*,#24000,.F.);
#31894=ORIENTED_EDGE('',*,*,#24001,.F.);
#31895=ORIENTED_EDGE('',*,*,#24002,.F.);
#31896=ORIENTED_EDGE('',*,*,#24003,.F.);
#31897=ORIENTED_EDGE('',*,*,#24004,.F.);
#31898=ORIENTED_EDGE('',*,*,#24005,.F.);
#31899=ORIENTED_EDGE('',*,*,#24006,.F.);
#31900=ORIENTED_EDGE('',*,*,#24007,.F.);
#31901=ORIENTED_EDGE('',*,*,#24008,.F.);
#31902=ORIENTED_EDGE('',*,*,#24009,.F.);
#31903=ORIENTED_EDGE('',*,*,#24010,.F.);
#31904=ORIENTED_EDGE('',*,*,#24011,.F.);
#31905=ORIENTED_EDGE('',*,*,#24012,.F.);
#31906=ORIENTED_EDGE('',*,*,#24013,.F.);
#31907=ORIENTED_EDGE('',*,*,#24014,.F.);
#31908=ORIENTED_EDGE('',*,*,#24015,.F.);
#31909=ORIENTED_EDGE('',*,*,#24016,.F.);
#31910=ORIENTED_EDGE('',*,*,#24017,.F.);
#31911=ORIENTED_EDGE('',*,*,#24018,.F.);
#31912=ORIENTED_EDGE('',*,*,#24019,.F.);
#31913=ORIENTED_EDGE('',*,*,#24020,.F.);
#31914=ORIENTED_EDGE('',*,*,#24021,.F.);
#31915=ORIENTED_EDGE('',*,*,#24022,.F.);
#31916=ORIENTED_EDGE('',*,*,#24023,.F.);
#31917=ORIENTED_EDGE('',*,*,#24024,.F.);
#31918=ORIENTED_EDGE('',*,*,#24025,.F.);
#31919=ORIENTED_EDGE('',*,*,#24026,.F.);
#31920=ORIENTED_EDGE('',*,*,#24027,.F.);
#31921=ORIENTED_EDGE('',*,*,#24028,.F.);
#31922=ORIENTED_EDGE('',*,*,#24029,.F.);
#31923=ORIENTED_EDGE('',*,*,#24030,.F.);
#31924=ORIENTED_EDGE('',*,*,#24031,.F.);
#31925=ORIENTED_EDGE('',*,*,#24032,.F.);
#31926=ORIENTED_EDGE('',*,*,#24033,.F.);
#31927=ORIENTED_EDGE('',*,*,#24034,.F.);
#31928=ORIENTED_EDGE('',*,*,#24035,.F.);
#31929=ORIENTED_EDGE('',*,*,#24036,.F.);
#31930=ORIENTED_EDGE('',*,*,#24037,.F.);
#31931=ORIENTED_EDGE('',*,*,#24038,.F.);
#31932=ORIENTED_EDGE('',*,*,#24039,.F.);
#31933=ORIENTED_EDGE('',*,*,#24040,.F.);
#31934=ORIENTED_EDGE('',*,*,#24041,.F.);
#31935=ORIENTED_EDGE('',*,*,#24042,.F.);
#31936=ORIENTED_EDGE('',*,*,#24043,.F.);
#31937=ORIENTED_EDGE('',*,*,#24044,.F.);
#31938=ORIENTED_EDGE('',*,*,#24045,.F.);
#31939=ORIENTED_EDGE('',*,*,#24046,.F.);
#31940=ORIENTED_EDGE('',*,*,#24047,.F.);
#31941=ORIENTED_EDGE('',*,*,#24048,.F.);
#31942=ORIENTED_EDGE('',*,*,#24049,.F.);
#31943=ORIENTED_EDGE('',*,*,#24050,.F.);
#31944=ORIENTED_EDGE('',*,*,#24051,.F.);
#31945=ORIENTED_EDGE('',*,*,#24052,.F.);
#31946=ORIENTED_EDGE('',*,*,#24053,.F.);
#31947=ORIENTED_EDGE('',*,*,#24054,.F.);
#31948=ORIENTED_EDGE('',*,*,#24055,.F.);
#31949=ORIENTED_EDGE('',*,*,#24056,.F.);
#31950=ORIENTED_EDGE('',*,*,#24057,.F.);
#31951=ORIENTED_EDGE('',*,*,#24058,.F.);
#31952=ORIENTED_EDGE('',*,*,#24059,.F.);
#31953=ORIENTED_EDGE('',*,*,#24060,.F.);
#31954=ORIENTED_EDGE('',*,*,#24061,.F.);
#31955=ORIENTED_EDGE('',*,*,#24062,.F.);
#31956=ORIENTED_EDGE('',*,*,#24063,.F.);
#31957=ORIENTED_EDGE('',*,*,#24064,.F.);
#31958=ORIENTED_EDGE('',*,*,#24065,.F.);
#31959=ORIENTED_EDGE('',*,*,#24066,.F.);
#31960=ORIENTED_EDGE('',*,*,#24067,.F.);
#31961=ORIENTED_EDGE('',*,*,#24068,.F.);
#31962=ORIENTED_EDGE('',*,*,#24069,.F.);
#31963=ORIENTED_EDGE('',*,*,#24070,.F.);
#31964=ORIENTED_EDGE('',*,*,#24071,.F.);
#31965=ORIENTED_EDGE('',*,*,#24072,.F.);
#31966=ORIENTED_EDGE('',*,*,#24073,.F.);
#31967=ORIENTED_EDGE('',*,*,#24074,.F.);
#31968=ORIENTED_EDGE('',*,*,#24075,.F.);
#31969=ORIENTED_EDGE('',*,*,#24076,.F.);
#31970=ORIENTED_EDGE('',*,*,#24077,.F.);
#31971=ORIENTED_EDGE('',*,*,#24078,.F.);
#31972=ORIENTED_EDGE('',*,*,#24079,.F.);
#31973=ORIENTED_EDGE('',*,*,#24080,.F.);
#31974=ORIENTED_EDGE('',*,*,#24081,.F.);
#31975=ORIENTED_EDGE('',*,*,#24082,.F.);
#31976=ORIENTED_EDGE('',*,*,#24083,.F.);
#31977=ORIENTED_EDGE('',*,*,#24084,.F.);
#31978=ORIENTED_EDGE('',*,*,#24085,.F.);
#31979=ORIENTED_EDGE('',*,*,#24086,.F.);
#31980=ORIENTED_EDGE('',*,*,#24087,.F.);
#31981=ORIENTED_EDGE('',*,*,#24088,.F.);
#31982=ORIENTED_EDGE('',*,*,#24089,.F.);
#31983=ORIENTED_EDGE('',*,*,#24090,.F.);
#31984=ORIENTED_EDGE('',*,*,#24091,.F.);
#31985=ORIENTED_EDGE('',*,*,#24092,.F.);
#31986=ORIENTED_EDGE('',*,*,#24093,.F.);
#31987=ORIENTED_EDGE('',*,*,#24094,.F.);
#31988=ORIENTED_EDGE('',*,*,#24095,.F.);
#31989=ORIENTED_EDGE('',*,*,#24096,.F.);
#31990=ORIENTED_EDGE('',*,*,#24097,.F.);
#31991=ORIENTED_EDGE('',*,*,#24098,.F.);
#31992=ORIENTED_EDGE('',*,*,#24099,.F.);
#31993=ORIENTED_EDGE('',*,*,#24100,.F.);
#31994=ORIENTED_EDGE('',*,*,#24101,.F.);
#31995=ORIENTED_EDGE('',*,*,#24102,.F.);
#31996=ORIENTED_EDGE('',*,*,#24103,.F.);
#31997=ORIENTED_EDGE('',*,*,#24104,.F.);
#31998=ORIENTED_EDGE('',*,*,#24105,.F.);
#31999=ORIENTED_EDGE('',*,*,#24106,.F.);
#32000=ORIENTED_EDGE('',*,*,#24107,.F.);
#32001=ORIENTED_EDGE('',*,*,#24108,.F.);
#32002=ORIENTED_EDGE('',*,*,#24109,.F.);
#32003=ORIENTED_EDGE('',*,*,#24110,.F.);
#32004=ORIENTED_EDGE('',*,*,#24111,.F.);
#32005=ORIENTED_EDGE('',*,*,#24112,.F.);
#32006=ORIENTED_EDGE('',*,*,#24113,.F.);
#32007=ORIENTED_EDGE('',*,*,#24114,.F.);
#32008=ORIENTED_EDGE('',*,*,#24115,.F.);
#32009=ORIENTED_EDGE('',*,*,#24116,.F.);
#32010=ORIENTED_EDGE('',*,*,#24117,.F.);
#32011=ORIENTED_EDGE('',*,*,#24118,.F.);
#32012=ORIENTED_EDGE('',*,*,#24119,.F.);
#32013=ORIENTED_EDGE('',*,*,#24120,.F.);
#32014=ORIENTED_EDGE('',*,*,#24121,.F.);
#32015=ORIENTED_EDGE('',*,*,#24122,.F.);
#32016=ORIENTED_EDGE('',*,*,#24123,.F.);
#32017=ORIENTED_EDGE('',*,*,#24124,.F.);
#32018=ORIENTED_EDGE('',*,*,#24125,.F.);
#32019=ORIENTED_EDGE('',*,*,#24126,.F.);
#32020=ORIENTED_EDGE('',*,*,#24127,.F.);
#32021=ORIENTED_EDGE('',*,*,#24128,.F.);
#32022=ORIENTED_EDGE('',*,*,#24129,.F.);
#32023=ORIENTED_EDGE('',*,*,#24130,.F.);
#32024=ORIENTED_EDGE('',*,*,#24131,.F.);
#32025=ORIENTED_EDGE('',*,*,#24132,.F.);
#32026=ORIENTED_EDGE('',*,*,#24133,.F.);
#32027=ORIENTED_EDGE('',*,*,#24134,.F.);
#32028=ORIENTED_EDGE('',*,*,#24135,.F.);
#32029=ORIENTED_EDGE('',*,*,#24136,.F.);
#32030=ORIENTED_EDGE('',*,*,#24137,.F.);
#32031=ORIENTED_EDGE('',*,*,#24138,.F.);
#32032=ORIENTED_EDGE('',*,*,#24139,.F.);
#32033=ORIENTED_EDGE('',*,*,#24140,.F.);
#32034=ORIENTED_EDGE('',*,*,#24141,.F.);
#32035=ORIENTED_EDGE('',*,*,#24142,.F.);
#32036=ORIENTED_EDGE('',*,*,#24143,.F.);
#32037=ORIENTED_EDGE('',*,*,#24144,.F.);
#32038=ORIENTED_EDGE('',*,*,#24145,.F.);
#32039=ORIENTED_EDGE('',*,*,#24146,.F.);
#32040=ORIENTED_EDGE('',*,*,#24147,.F.);
#32041=ORIENTED_EDGE('',*,*,#24148,.F.);
#32042=ORIENTED_EDGE('',*,*,#24149,.F.);
#32043=ORIENTED_EDGE('',*,*,#24150,.F.);
#32044=ORIENTED_EDGE('',*,*,#24151,.F.);
#32045=ORIENTED_EDGE('',*,*,#24152,.F.);
#32046=ORIENTED_EDGE('',*,*,#24153,.F.);
#32047=ORIENTED_EDGE('',*,*,#24154,.F.);
#32048=ORIENTED_EDGE('',*,*,#24155,.F.);
#32049=ORIENTED_EDGE('',*,*,#24156,.F.);
#32050=ORIENTED_EDGE('',*,*,#24157,.F.);
#32051=ORIENTED_EDGE('',*,*,#24158,.F.);
#32052=ORIENTED_EDGE('',*,*,#24159,.F.);
#32053=ORIENTED_EDGE('',*,*,#24160,.F.);
#32054=ORIENTED_EDGE('',*,*,#24161,.F.);
#32055=ORIENTED_EDGE('',*,*,#24162,.F.);
#32056=ORIENTED_EDGE('',*,*,#24163,.F.);
#32057=ORIENTED_EDGE('',*,*,#24164,.F.);
#32058=ORIENTED_EDGE('',*,*,#24165,.F.);
#32059=ORIENTED_EDGE('',*,*,#24166,.F.);
#32060=ORIENTED_EDGE('',*,*,#24167,.F.);
#32061=ORIENTED_EDGE('',*,*,#24168,.F.);
#32062=ORIENTED_EDGE('',*,*,#24169,.F.);
#32063=ORIENTED_EDGE('',*,*,#24170,.F.);
#32064=ORIENTED_EDGE('',*,*,#24171,.F.);
#32065=ORIENTED_EDGE('',*,*,#24172,.F.);
#32066=ORIENTED_EDGE('',*,*,#24173,.F.);
#32067=ORIENTED_EDGE('',*,*,#24174,.F.);
#32068=ORIENTED_EDGE('',*,*,#24175,.F.);
#32069=ORIENTED_EDGE('',*,*,#24176,.F.);
#32070=ORIENTED_EDGE('',*,*,#24177,.F.);
#32071=ORIENTED_EDGE('',*,*,#24178,.F.);
#32072=ORIENTED_EDGE('',*,*,#24179,.F.);
#32073=ORIENTED_EDGE('',*,*,#24180,.F.);
#32074=ORIENTED_EDGE('',*,*,#24181,.F.);
#32075=ORIENTED_EDGE('',*,*,#24182,.F.);
#32076=ORIENTED_EDGE('',*,*,#24183,.F.);
#32077=ORIENTED_EDGE('',*,*,#24184,.F.);
#32078=ORIENTED_EDGE('',*,*,#24185,.F.);
#32079=ORIENTED_EDGE('',*,*,#24186,.F.);
#32080=ORIENTED_EDGE('',*,*,#24187,.F.);
#32081=ORIENTED_EDGE('',*,*,#24188,.F.);
#32082=ORIENTED_EDGE('',*,*,#24189,.F.);
#32083=ORIENTED_EDGE('',*,*,#24190,.F.);
#32084=ORIENTED_EDGE('',*,*,#24191,.F.);
#32085=ORIENTED_EDGE('',*,*,#24192,.F.);
#32086=ORIENTED_EDGE('',*,*,#24193,.F.);
#32087=ORIENTED_EDGE('',*,*,#24194,.F.);
#32088=ORIENTED_EDGE('',*,*,#24195,.F.);
#32089=ORIENTED_EDGE('',*,*,#24196,.F.);
#32090=ORIENTED_EDGE('',*,*,#24197,.F.);
#32091=ORIENTED_EDGE('',*,*,#24198,.F.);
#32092=ORIENTED_EDGE('',*,*,#24199,.F.);
#32093=ORIENTED_EDGE('',*,*,#24200,.F.);
#32094=ORIENTED_EDGE('',*,*,#24201,.F.);
#32095=ORIENTED_EDGE('',*,*,#24202,.F.);
#32096=ORIENTED_EDGE('',*,*,#24203,.F.);
#32097=ORIENTED_EDGE('',*,*,#24204,.F.);
#32098=ORIENTED_EDGE('',*,*,#24205,.F.);
#32099=ORIENTED_EDGE('',*,*,#24206,.F.);
#32100=ORIENTED_EDGE('',*,*,#24207,.F.);
#32101=ORIENTED_EDGE('',*,*,#24208,.F.);
#32102=ORIENTED_EDGE('',*,*,#24209,.F.);
#32103=ORIENTED_EDGE('',*,*,#24210,.F.);
#32104=ORIENTED_EDGE('',*,*,#24211,.F.);
#32105=ORIENTED_EDGE('',*,*,#24212,.F.);
#32106=ORIENTED_EDGE('',*,*,#24213,.F.);
#32107=ORIENTED_EDGE('',*,*,#24214,.F.);
#32108=ORIENTED_EDGE('',*,*,#24215,.F.);
#32109=ORIENTED_EDGE('',*,*,#24216,.F.);
#32110=ORIENTED_EDGE('',*,*,#24217,.F.);
#32111=ORIENTED_EDGE('',*,*,#24218,.F.);
#32112=ORIENTED_EDGE('',*,*,#24219,.F.);
#32113=ORIENTED_EDGE('',*,*,#24220,.F.);
#32114=ORIENTED_EDGE('',*,*,#24221,.F.);
#32115=ORIENTED_EDGE('',*,*,#24222,.F.);
#32116=ORIENTED_EDGE('',*,*,#24223,.F.);
#32117=ORIENTED_EDGE('',*,*,#24224,.F.);
#32118=ORIENTED_EDGE('',*,*,#24225,.F.);
#32119=ORIENTED_EDGE('',*,*,#24226,.F.);
#32120=ORIENTED_EDGE('',*,*,#24227,.F.);
#32121=ORIENTED_EDGE('',*,*,#24228,.F.);
#32122=ORIENTED_EDGE('',*,*,#24229,.F.);
#32123=ORIENTED_EDGE('',*,*,#24230,.F.);
#32124=ORIENTED_EDGE('',*,*,#24231,.F.);
#32125=ORIENTED_EDGE('',*,*,#24232,.F.);
#32126=ORIENTED_EDGE('',*,*,#24233,.F.);
#32127=ORIENTED_EDGE('',*,*,#24234,.F.);
#32128=ORIENTED_EDGE('',*,*,#24235,.F.);
#32129=ORIENTED_EDGE('',*,*,#24236,.F.);
#32130=ORIENTED_EDGE('',*,*,#24237,.F.);
#32131=ORIENTED_EDGE('',*,*,#24238,.F.);
#32132=ORIENTED_EDGE('',*,*,#24239,.F.);
#32133=ORIENTED_EDGE('',*,*,#24240,.F.);
#32134=ORIENTED_EDGE('',*,*,#24241,.F.);
#32135=ORIENTED_EDGE('',*,*,#24242,.F.);
#32136=ORIENTED_EDGE('',*,*,#24243,.F.);
#32137=ORIENTED_EDGE('',*,*,#24244,.F.);
#32138=ORIENTED_EDGE('',*,*,#23009,.F.);
#32139=ORIENTED_EDGE('',*,*,#24245,.T.);
#32140=ORIENTED_EDGE('',*,*,#24246,.T.);
#32141=ORIENTED_EDGE('',*,*,#24247,.T.);
#32142=ORIENTED_EDGE('',*,*,#24248,.T.);
#32143=ORIENTED_EDGE('',*,*,#24249,.T.);
#32144=ORIENTED_EDGE('',*,*,#24250,.T.);
#32145=ORIENTED_EDGE('',*,*,#24251,.T.);
#32146=ORIENTED_EDGE('',*,*,#24252,.T.);
#32147=ORIENTED_EDGE('',*,*,#24253,.T.);
#32148=ORIENTED_EDGE('',*,*,#24254,.T.);
#32149=ORIENTED_EDGE('',*,*,#24255,.T.);
#32150=ORIENTED_EDGE('',*,*,#24256,.T.);
#32151=ORIENTED_EDGE('',*,*,#24257,.T.);
#32152=ORIENTED_EDGE('',*,*,#24258,.T.);
#32153=ORIENTED_EDGE('',*,*,#24259,.T.);
#32154=ORIENTED_EDGE('',*,*,#24260,.T.);
#32155=ORIENTED_EDGE('',*,*,#24261,.T.);
#32156=ORIENTED_EDGE('',*,*,#24262,.T.);
#32157=ORIENTED_EDGE('',*,*,#24263,.T.);
#32158=ORIENTED_EDGE('',*,*,#24264,.T.);
#32159=ORIENTED_EDGE('',*,*,#24265,.T.);
#32160=ORIENTED_EDGE('',*,*,#24266,.T.);
#32161=ORIENTED_EDGE('',*,*,#24267,.T.);
#32162=ORIENTED_EDGE('',*,*,#24268,.T.);
#32163=ORIENTED_EDGE('',*,*,#24269,.T.);
#32164=ORIENTED_EDGE('',*,*,#24270,.T.);
#32165=ORIENTED_EDGE('',*,*,#24271,.T.);
#32166=ORIENTED_EDGE('',*,*,#24272,.T.);
#32167=ORIENTED_EDGE('',*,*,#24273,.T.);
#32168=ORIENTED_EDGE('',*,*,#24274,.T.);
#32169=ORIENTED_EDGE('',*,*,#24275,.T.);
#32170=ORIENTED_EDGE('',*,*,#24276,.T.);
#32171=ORIENTED_EDGE('',*,*,#24277,.T.);
#32172=ORIENTED_EDGE('',*,*,#24278,.T.);
#32173=ORIENTED_EDGE('',*,*,#24279,.T.);
#32174=ORIENTED_EDGE('',*,*,#24280,.T.);
#32175=ORIENTED_EDGE('',*,*,#24281,.T.);
#32176=ORIENTED_EDGE('',*,*,#24282,.T.);
#32177=ORIENTED_EDGE('',*,*,#24283,.T.);
#32178=ORIENTED_EDGE('',*,*,#24284,.T.);
#32179=ORIENTED_EDGE('',*,*,#24285,.T.);
#32180=ORIENTED_EDGE('',*,*,#24286,.T.);
#32181=ORIENTED_EDGE('',*,*,#24287,.T.);
#32182=ORIENTED_EDGE('',*,*,#24288,.T.);
#32183=ORIENTED_EDGE('',*,*,#24289,.T.);
#32184=ORIENTED_EDGE('',*,*,#24290,.T.);
#32185=ORIENTED_EDGE('',*,*,#24291,.T.);
#32186=ORIENTED_EDGE('',*,*,#24292,.T.);
#32187=ORIENTED_EDGE('',*,*,#24293,.T.);
#32188=ORIENTED_EDGE('',*,*,#24294,.T.);
#32189=ORIENTED_EDGE('',*,*,#24295,.T.);
#32190=ORIENTED_EDGE('',*,*,#24296,.T.);
#32191=ORIENTED_EDGE('',*,*,#24297,.T.);
#32192=ORIENTED_EDGE('',*,*,#24298,.T.);
#32193=ORIENTED_EDGE('',*,*,#24299,.T.);
#32194=ORIENTED_EDGE('',*,*,#24300,.T.);
#32195=ORIENTED_EDGE('',*,*,#24301,.T.);
#32196=ORIENTED_EDGE('',*,*,#24302,.T.);
#32197=ORIENTED_EDGE('',*,*,#24303,.T.);
#32198=ORIENTED_EDGE('',*,*,#24304,.T.);
#32199=ORIENTED_EDGE('',*,*,#24305,.T.);
#32200=ORIENTED_EDGE('',*,*,#24306,.T.);
#32201=ORIENTED_EDGE('',*,*,#24307,.T.);
#32202=ORIENTED_EDGE('',*,*,#24308,.T.);
#32203=ORIENTED_EDGE('',*,*,#24309,.T.);
#32204=ORIENTED_EDGE('',*,*,#24310,.T.);
#32205=ORIENTED_EDGE('',*,*,#24311,.T.);
#32206=ORIENTED_EDGE('',*,*,#24312,.T.);
#32207=ORIENTED_EDGE('',*,*,#24313,.T.);
#32208=ORIENTED_EDGE('',*,*,#24314,.T.);
#32209=ORIENTED_EDGE('',*,*,#24315,.T.);
#32210=ORIENTED_EDGE('',*,*,#24316,.T.);
#32211=ORIENTED_EDGE('',*,*,#24317,.T.);
#32212=ORIENTED_EDGE('',*,*,#24318,.T.);
#32213=ORIENTED_EDGE('',*,*,#24319,.T.);
#32214=ORIENTED_EDGE('',*,*,#24320,.T.);
#32215=ORIENTED_EDGE('',*,*,#24321,.T.);
#32216=ORIENTED_EDGE('',*,*,#24322,.T.);
#32217=ORIENTED_EDGE('',*,*,#24323,.T.);
#32218=ORIENTED_EDGE('',*,*,#24324,.T.);
#32219=ORIENTED_EDGE('',*,*,#24325,.T.);
#32220=ORIENTED_EDGE('',*,*,#24326,.T.);
#32221=ORIENTED_EDGE('',*,*,#24327,.T.);
#32222=ORIENTED_EDGE('',*,*,#24328,.T.);
#32223=ORIENTED_EDGE('',*,*,#24329,.T.);
#32224=ORIENTED_EDGE('',*,*,#24330,.T.);
#32225=ORIENTED_EDGE('',*,*,#24331,.T.);
#32226=ORIENTED_EDGE('',*,*,#24332,.T.);
#32227=ORIENTED_EDGE('',*,*,#24333,.T.);
#32228=ORIENTED_EDGE('',*,*,#24334,.T.);
#32229=ORIENTED_EDGE('',*,*,#24335,.T.);
#32230=ORIENTED_EDGE('',*,*,#24336,.T.);
#32231=ORIENTED_EDGE('',*,*,#24337,.T.);
#32232=ORIENTED_EDGE('',*,*,#24338,.T.);
#32233=ORIENTED_EDGE('',*,*,#24339,.T.);
#32234=ORIENTED_EDGE('',*,*,#24340,.T.);
#32235=ORIENTED_EDGE('',*,*,#24341,.T.);
#32236=ORIENTED_EDGE('',*,*,#24342,.T.);
#32237=ORIENTED_EDGE('',*,*,#24343,.T.);
#32238=ORIENTED_EDGE('',*,*,#24344,.T.);
#32239=ORIENTED_EDGE('',*,*,#24345,.T.);
#32240=ORIENTED_EDGE('',*,*,#24346,.T.);
#32241=ORIENTED_EDGE('',*,*,#24347,.T.);
#32242=ORIENTED_EDGE('',*,*,#24348,.T.);
#32243=ORIENTED_EDGE('',*,*,#24349,.T.);
#32244=ORIENTED_EDGE('',*,*,#24350,.T.);
#32245=ORIENTED_EDGE('',*,*,#24351,.T.);
#32246=ORIENTED_EDGE('',*,*,#24352,.T.);
#32247=ORIENTED_EDGE('',*,*,#24353,.T.);
#32248=ORIENTED_EDGE('',*,*,#24354,.T.);
#32249=ORIENTED_EDGE('',*,*,#24355,.T.);
#32250=ORIENTED_EDGE('',*,*,#24356,.T.);
#32251=ORIENTED_EDGE('',*,*,#24357,.T.);
#32252=ORIENTED_EDGE('',*,*,#24358,.T.);
#32253=ORIENTED_EDGE('',*,*,#24359,.T.);
#32254=ORIENTED_EDGE('',*,*,#24360,.T.);
#32255=ORIENTED_EDGE('',*,*,#24361,.T.);
#32256=ORIENTED_EDGE('',*,*,#24362,.T.);
#32257=ORIENTED_EDGE('',*,*,#24363,.T.);
#32258=ORIENTED_EDGE('',*,*,#24364,.T.);
#32259=ORIENTED_EDGE('',*,*,#24365,.T.);
#32260=ORIENTED_EDGE('',*,*,#24366,.T.);
#32261=ORIENTED_EDGE('',*,*,#24367,.T.);
#32262=ORIENTED_EDGE('',*,*,#24368,.T.);
#32263=ORIENTED_EDGE('',*,*,#24369,.T.);
#32264=ORIENTED_EDGE('',*,*,#24370,.T.);
#32265=ORIENTED_EDGE('',*,*,#24371,.T.);
#32266=ORIENTED_EDGE('',*,*,#24372,.T.);
#32267=ORIENTED_EDGE('',*,*,#24373,.T.);
#32268=ORIENTED_EDGE('',*,*,#24374,.T.);
#32269=ORIENTED_EDGE('',*,*,#24375,.T.);
#32270=ORIENTED_EDGE('',*,*,#24376,.T.);
#32271=ORIENTED_EDGE('',*,*,#24377,.T.);
#32272=ORIENTED_EDGE('',*,*,#24378,.T.);
#32273=ORIENTED_EDGE('',*,*,#24379,.T.);
#32274=ORIENTED_EDGE('',*,*,#24380,.T.);
#32275=ORIENTED_EDGE('',*,*,#24381,.T.);
#32276=ORIENTED_EDGE('',*,*,#24382,.T.);
#32277=ORIENTED_EDGE('',*,*,#24383,.T.);
#32278=ORIENTED_EDGE('',*,*,#24384,.T.);
#32279=ORIENTED_EDGE('',*,*,#24385,.T.);
#32280=ORIENTED_EDGE('',*,*,#24386,.T.);
#32281=ORIENTED_EDGE('',*,*,#24387,.T.);
#32282=ORIENTED_EDGE('',*,*,#24388,.T.);
#32283=ORIENTED_EDGE('',*,*,#24389,.T.);
#32284=ORIENTED_EDGE('',*,*,#24390,.T.);
#32285=ORIENTED_EDGE('',*,*,#24391,.T.);
#32286=ORIENTED_EDGE('',*,*,#24392,.T.);
#32287=ORIENTED_EDGE('',*,*,#24393,.T.);
#32288=ORIENTED_EDGE('',*,*,#24394,.T.);
#32289=ORIENTED_EDGE('',*,*,#24395,.T.);
#32290=ORIENTED_EDGE('',*,*,#24396,.T.);
#32291=ORIENTED_EDGE('',*,*,#24397,.T.);
#32292=ORIENTED_EDGE('',*,*,#24398,.T.);
#32293=ORIENTED_EDGE('',*,*,#24399,.T.);
#32294=ORIENTED_EDGE('',*,*,#24400,.T.);
#32295=ORIENTED_EDGE('',*,*,#24401,.T.);
#32296=ORIENTED_EDGE('',*,*,#24402,.T.);
#32297=ORIENTED_EDGE('',*,*,#24403,.T.);
#32298=ORIENTED_EDGE('',*,*,#24404,.T.);
#32299=ORIENTED_EDGE('',*,*,#24405,.T.);
#32300=ORIENTED_EDGE('',*,*,#24406,.T.);
#32301=ORIENTED_EDGE('',*,*,#24407,.T.);
#32302=ORIENTED_EDGE('',*,*,#24408,.T.);
#32303=ORIENTED_EDGE('',*,*,#24409,.T.);
#32304=ORIENTED_EDGE('',*,*,#24410,.T.);
#32305=ORIENTED_EDGE('',*,*,#24411,.T.);
#32306=ORIENTED_EDGE('',*,*,#24412,.T.);
#32307=ORIENTED_EDGE('',*,*,#24413,.T.);
#32308=ORIENTED_EDGE('',*,*,#24414,.T.);
#32309=ORIENTED_EDGE('',*,*,#24415,.T.);
#32310=ORIENTED_EDGE('',*,*,#24416,.T.);
#32311=ORIENTED_EDGE('',*,*,#24417,.T.);
#32312=ORIENTED_EDGE('',*,*,#24418,.T.);
#32313=ORIENTED_EDGE('',*,*,#24419,.T.);
#32314=ORIENTED_EDGE('',*,*,#24420,.T.);
#32315=ORIENTED_EDGE('',*,*,#24421,.T.);
#32316=ORIENTED_EDGE('',*,*,#24422,.T.);
#32317=ORIENTED_EDGE('',*,*,#24423,.T.);
#32318=ORIENTED_EDGE('',*,*,#24424,.T.);
#32319=ORIENTED_EDGE('',*,*,#24425,.T.);
#32320=ORIENTED_EDGE('',*,*,#24426,.T.);
#32321=ORIENTED_EDGE('',*,*,#24427,.T.);
#32322=ORIENTED_EDGE('',*,*,#24428,.T.);
#32323=ORIENTED_EDGE('',*,*,#24429,.T.);
#32324=ORIENTED_EDGE('',*,*,#24430,.T.);
#32325=ORIENTED_EDGE('',*,*,#24431,.T.);
#32326=ORIENTED_EDGE('',*,*,#24432,.T.);
#32327=ORIENTED_EDGE('',*,*,#24433,.T.);
#32328=ORIENTED_EDGE('',*,*,#24434,.T.);
#32329=ORIENTED_EDGE('',*,*,#24435,.T.);
#32330=ORIENTED_EDGE('',*,*,#24436,.T.);
#32331=ORIENTED_EDGE('',*,*,#24437,.T.);
#32332=ORIENTED_EDGE('',*,*,#24438,.T.);
#32333=ORIENTED_EDGE('',*,*,#24439,.T.);
#32334=ORIENTED_EDGE('',*,*,#24440,.T.);
#32335=ORIENTED_EDGE('',*,*,#24441,.T.);
#32336=ORIENTED_EDGE('',*,*,#24442,.T.);
#32337=ORIENTED_EDGE('',*,*,#24443,.T.);
#32338=ORIENTED_EDGE('',*,*,#24444,.T.);
#32339=ORIENTED_EDGE('',*,*,#24445,.T.);
#32340=ORIENTED_EDGE('',*,*,#24446,.T.);
#32341=ORIENTED_EDGE('',*,*,#24447,.T.);
#32342=ORIENTED_EDGE('',*,*,#24448,.T.);
#32343=ORIENTED_EDGE('',*,*,#24449,.T.);
#32344=ORIENTED_EDGE('',*,*,#24450,.T.);
#32345=ORIENTED_EDGE('',*,*,#24451,.T.);
#32346=ORIENTED_EDGE('',*,*,#24452,.T.);
#32347=ORIENTED_EDGE('',*,*,#24453,.T.);
#32348=ORIENTED_EDGE('',*,*,#24454,.T.);
#32349=ORIENTED_EDGE('',*,*,#24455,.T.);
#32350=ORIENTED_EDGE('',*,*,#24456,.T.);
#32351=ORIENTED_EDGE('',*,*,#24457,.T.);
#32352=ORIENTED_EDGE('',*,*,#24458,.T.);
#32353=ORIENTED_EDGE('',*,*,#24459,.T.);
#32354=ORIENTED_EDGE('',*,*,#24460,.T.);
#32355=ORIENTED_EDGE('',*,*,#24461,.T.);
#32356=ORIENTED_EDGE('',*,*,#24462,.T.);
#32357=ORIENTED_EDGE('',*,*,#24463,.T.);
#32358=ORIENTED_EDGE('',*,*,#24464,.T.);
#32359=ORIENTED_EDGE('',*,*,#24465,.T.);
#32360=ORIENTED_EDGE('',*,*,#24466,.T.);
#32361=ORIENTED_EDGE('',*,*,#24467,.T.);
#32362=ORIENTED_EDGE('',*,*,#24468,.T.);
#32363=ORIENTED_EDGE('',*,*,#24469,.T.);
#32364=ORIENTED_EDGE('',*,*,#24470,.T.);
#32365=ORIENTED_EDGE('',*,*,#24471,.T.);
#32366=ORIENTED_EDGE('',*,*,#24472,.T.);
#32367=ORIENTED_EDGE('',*,*,#24473,.T.);
#32368=ORIENTED_EDGE('',*,*,#24474,.T.);
#32369=ORIENTED_EDGE('',*,*,#24475,.T.);
#32370=ORIENTED_EDGE('',*,*,#24476,.T.);
#32371=ORIENTED_EDGE('',*,*,#24477,.T.);
#32372=ORIENTED_EDGE('',*,*,#24478,.T.);
#32373=ORIENTED_EDGE('',*,*,#24479,.T.);
#32374=ORIENTED_EDGE('',*,*,#24480,.T.);
#32375=ORIENTED_EDGE('',*,*,#24481,.T.);
#32376=ORIENTED_EDGE('',*,*,#24482,.T.);
#32377=ORIENTED_EDGE('',*,*,#24483,.T.);
#32378=ORIENTED_EDGE('',*,*,#24484,.T.);
#32379=ORIENTED_EDGE('',*,*,#24485,.T.);
#32380=ORIENTED_EDGE('',*,*,#24486,.T.);
#32381=ORIENTED_EDGE('',*,*,#24487,.T.);
#32382=ORIENTED_EDGE('',*,*,#24488,.T.);
#32383=ORIENTED_EDGE('',*,*,#24489,.T.);
#32384=ORIENTED_EDGE('',*,*,#24490,.T.);
#32385=ORIENTED_EDGE('',*,*,#24491,.T.);
#32386=ORIENTED_EDGE('',*,*,#24492,.T.);
#32387=ORIENTED_EDGE('',*,*,#24493,.T.);
#32388=ORIENTED_EDGE('',*,*,#24494,.T.);
#32389=ORIENTED_EDGE('',*,*,#24495,.T.);
#32390=ORIENTED_EDGE('',*,*,#24496,.T.);
#32391=ORIENTED_EDGE('',*,*,#24497,.T.);
#32392=ORIENTED_EDGE('',*,*,#24498,.T.);
#32393=ORIENTED_EDGE('',*,*,#24499,.T.);
#32394=ORIENTED_EDGE('',*,*,#24500,.T.);
#32395=ORIENTED_EDGE('',*,*,#24501,.T.);
#32396=ORIENTED_EDGE('',*,*,#24502,.T.);
#32397=ORIENTED_EDGE('',*,*,#24503,.T.);
#32398=ORIENTED_EDGE('',*,*,#24504,.T.);
#32399=ORIENTED_EDGE('',*,*,#24505,.T.);
#32400=ORIENTED_EDGE('',*,*,#24506,.T.);
#32401=ORIENTED_EDGE('',*,*,#24507,.T.);
#32402=ORIENTED_EDGE('',*,*,#24508,.T.);
#32403=ORIENTED_EDGE('',*,*,#24509,.T.);
#32404=ORIENTED_EDGE('',*,*,#24510,.T.);
#32405=ORIENTED_EDGE('',*,*,#24511,.T.);
#32406=ORIENTED_EDGE('',*,*,#24512,.T.);
#32407=ORIENTED_EDGE('',*,*,#24513,.T.);
#32408=ORIENTED_EDGE('',*,*,#24514,.T.);
#32409=ORIENTED_EDGE('',*,*,#24515,.T.);
#32410=ORIENTED_EDGE('',*,*,#24516,.T.);
#32411=ORIENTED_EDGE('',*,*,#24517,.T.);
#32412=ORIENTED_EDGE('',*,*,#24518,.T.);
#32413=ORIENTED_EDGE('',*,*,#24519,.T.);
#32414=ORIENTED_EDGE('',*,*,#24520,.T.);
#32415=ORIENTED_EDGE('',*,*,#24521,.T.);
#32416=ORIENTED_EDGE('',*,*,#24522,.T.);
#32417=ORIENTED_EDGE('',*,*,#24523,.T.);
#32418=ORIENTED_EDGE('',*,*,#24524,.T.);
#32419=ORIENTED_EDGE('',*,*,#24525,.T.);
#32420=ORIENTED_EDGE('',*,*,#24526,.T.);
#32421=ORIENTED_EDGE('',*,*,#24527,.T.);
#32422=ORIENTED_EDGE('',*,*,#24528,.T.);
#32423=ORIENTED_EDGE('',*,*,#24529,.T.);
#32424=ORIENTED_EDGE('',*,*,#24530,.T.);
#32425=ORIENTED_EDGE('',*,*,#24531,.T.);
#32426=ORIENTED_EDGE('',*,*,#24532,.T.);
#32427=ORIENTED_EDGE('',*,*,#24533,.T.);
#32428=ORIENTED_EDGE('',*,*,#24534,.T.);
#32429=ORIENTED_EDGE('',*,*,#24535,.T.);
#32430=ORIENTED_EDGE('',*,*,#24536,.T.);
#32431=ORIENTED_EDGE('',*,*,#24537,.T.);
#32432=ORIENTED_EDGE('',*,*,#24538,.T.);
#32433=ORIENTED_EDGE('',*,*,#24539,.T.);
#32434=ORIENTED_EDGE('',*,*,#24540,.T.);
#32435=ORIENTED_EDGE('',*,*,#24541,.T.);
#32436=ORIENTED_EDGE('',*,*,#24542,.T.);
#32437=ORIENTED_EDGE('',*,*,#24543,.T.);
#32438=ORIENTED_EDGE('',*,*,#24544,.T.);
#32439=ORIENTED_EDGE('',*,*,#24545,.T.);
#32440=ORIENTED_EDGE('',*,*,#24546,.T.);
#32441=ORIENTED_EDGE('',*,*,#24547,.T.);
#32442=ORIENTED_EDGE('',*,*,#24548,.T.);
#32443=ORIENTED_EDGE('',*,*,#24549,.T.);
#32444=ORIENTED_EDGE('',*,*,#24550,.T.);
#32445=ORIENTED_EDGE('',*,*,#24551,.T.);
#32446=ORIENTED_EDGE('',*,*,#24552,.T.);
#32447=ORIENTED_EDGE('',*,*,#24553,.T.);
#32448=ORIENTED_EDGE('',*,*,#24554,.T.);
#32449=ORIENTED_EDGE('',*,*,#24555,.T.);
#32450=ORIENTED_EDGE('',*,*,#24556,.T.);
#32451=ORIENTED_EDGE('',*,*,#24557,.T.);
#32452=ORIENTED_EDGE('',*,*,#24558,.T.);
#32453=ORIENTED_EDGE('',*,*,#24559,.T.);
#32454=ORIENTED_EDGE('',*,*,#24560,.T.);
#32455=ORIENTED_EDGE('',*,*,#24561,.T.);
#32456=ORIENTED_EDGE('',*,*,#24562,.T.);
#32457=ORIENTED_EDGE('',*,*,#24563,.T.);
#32458=ORIENTED_EDGE('',*,*,#24564,.T.);
#32459=ORIENTED_EDGE('',*,*,#24565,.T.);
#32460=ORIENTED_EDGE('',*,*,#24566,.T.);
#32461=ORIENTED_EDGE('',*,*,#24567,.T.);
#32462=ORIENTED_EDGE('',*,*,#24568,.T.);
#32463=ORIENTED_EDGE('',*,*,#24569,.T.);
#32464=ORIENTED_EDGE('',*,*,#24570,.T.);
#32465=ORIENTED_EDGE('',*,*,#24571,.T.);
#32466=ORIENTED_EDGE('',*,*,#24572,.T.);
#32467=ORIENTED_EDGE('',*,*,#24573,.T.);
#32468=ORIENTED_EDGE('',*,*,#24574,.T.);
#32469=ORIENTED_EDGE('',*,*,#24575,.T.);
#32470=ORIENTED_EDGE('',*,*,#24576,.T.);
#32471=ORIENTED_EDGE('',*,*,#24577,.T.);
#32472=ORIENTED_EDGE('',*,*,#24578,.T.);
#32473=ORIENTED_EDGE('',*,*,#24579,.T.);
#32474=ORIENTED_EDGE('',*,*,#24580,.T.);
#32475=ORIENTED_EDGE('',*,*,#24581,.T.);
#32476=ORIENTED_EDGE('',*,*,#24582,.T.);
#32477=ORIENTED_EDGE('',*,*,#24583,.T.);
#32478=ORIENTED_EDGE('',*,*,#24584,.T.);
#32479=ORIENTED_EDGE('',*,*,#24585,.T.);
#32480=ORIENTED_EDGE('',*,*,#24586,.T.);
#32481=ORIENTED_EDGE('',*,*,#24587,.T.);
#32482=ORIENTED_EDGE('',*,*,#24588,.T.);
#32483=ORIENTED_EDGE('',*,*,#24589,.T.);
#32484=ORIENTED_EDGE('',*,*,#24590,.T.);
#32485=ORIENTED_EDGE('',*,*,#24591,.T.);
#32486=ORIENTED_EDGE('',*,*,#24592,.T.);
#32487=ORIENTED_EDGE('',*,*,#24593,.T.);
#32488=ORIENTED_EDGE('',*,*,#24594,.T.);
#32489=ORIENTED_EDGE('',*,*,#24595,.T.);
#32490=ORIENTED_EDGE('',*,*,#24596,.T.);
#32491=ORIENTED_EDGE('',*,*,#24597,.T.);
#32492=ORIENTED_EDGE('',*,*,#24598,.T.);
#32493=ORIENTED_EDGE('',*,*,#24599,.T.);
#32494=ORIENTED_EDGE('',*,*,#24600,.T.);
#32495=ORIENTED_EDGE('',*,*,#24601,.T.);
#32496=ORIENTED_EDGE('',*,*,#24602,.T.);
#32497=ORIENTED_EDGE('',*,*,#24603,.T.);
#32498=ORIENTED_EDGE('',*,*,#24604,.T.);
#32499=ORIENTED_EDGE('',*,*,#24605,.T.);
#32500=ORIENTED_EDGE('',*,*,#24606,.T.);
#32501=ORIENTED_EDGE('',*,*,#24607,.T.);
#32502=ORIENTED_EDGE('',*,*,#24608,.T.);
#32503=ORIENTED_EDGE('',*,*,#24609,.T.);
#32504=ORIENTED_EDGE('',*,*,#24610,.T.);
#32505=ORIENTED_EDGE('',*,*,#24611,.T.);
#32506=ORIENTED_EDGE('',*,*,#24612,.T.);
#32507=ORIENTED_EDGE('',*,*,#24613,.T.);
#32508=ORIENTED_EDGE('',*,*,#24614,.T.);
#32509=ORIENTED_EDGE('',*,*,#24615,.T.);
#32510=ORIENTED_EDGE('',*,*,#24616,.T.);
#32511=ORIENTED_EDGE('',*,*,#24617,.T.);
#32512=ORIENTED_EDGE('',*,*,#24618,.T.);
#32513=ORIENTED_EDGE('',*,*,#24619,.T.);
#32514=ORIENTED_EDGE('',*,*,#24620,.T.);
#32515=ORIENTED_EDGE('',*,*,#24621,.T.);
#32516=ORIENTED_EDGE('',*,*,#24622,.T.);
#32517=ORIENTED_EDGE('',*,*,#24623,.T.);
#32518=ORIENTED_EDGE('',*,*,#24624,.T.);
#32519=ORIENTED_EDGE('',*,*,#24625,.T.);
#32520=ORIENTED_EDGE('',*,*,#24626,.T.);
#32521=ORIENTED_EDGE('',*,*,#24627,.T.);
#32522=ORIENTED_EDGE('',*,*,#24628,.T.);
#32523=ORIENTED_EDGE('',*,*,#24629,.T.);
#32524=ORIENTED_EDGE('',*,*,#24630,.T.);
#32525=ORIENTED_EDGE('',*,*,#24631,.T.);
#32526=ORIENTED_EDGE('',*,*,#24632,.T.);
#32527=ORIENTED_EDGE('',*,*,#24633,.T.);
#32528=ORIENTED_EDGE('',*,*,#24634,.T.);
#32529=ORIENTED_EDGE('',*,*,#24635,.T.);
#32530=ORIENTED_EDGE('',*,*,#24636,.T.);
#32531=ORIENTED_EDGE('',*,*,#24637,.T.);
#32532=ORIENTED_EDGE('',*,*,#24638,.T.);
#32533=ORIENTED_EDGE('',*,*,#24639,.T.);
#32534=ORIENTED_EDGE('',*,*,#24640,.T.);
#32535=ORIENTED_EDGE('',*,*,#24641,.T.);
#32536=ORIENTED_EDGE('',*,*,#24642,.T.);
#32537=ORIENTED_EDGE('',*,*,#24643,.T.);
#32538=ORIENTED_EDGE('',*,*,#24644,.T.);
#32539=ORIENTED_EDGE('',*,*,#24645,.T.);
#32540=ORIENTED_EDGE('',*,*,#24646,.T.);
#32541=ORIENTED_EDGE('',*,*,#24647,.T.);
#32542=ORIENTED_EDGE('',*,*,#24648,.T.);
#32543=ORIENTED_EDGE('',*,*,#24649,.T.);
#32544=ORIENTED_EDGE('',*,*,#24650,.T.);
#32545=ORIENTED_EDGE('',*,*,#24651,.T.);
#32546=ORIENTED_EDGE('',*,*,#24652,.T.);
#32547=ORIENTED_EDGE('',*,*,#24653,.T.);
#32548=ORIENTED_EDGE('',*,*,#24654,.T.);
#32549=ORIENTED_EDGE('',*,*,#24655,.T.);
#32550=ORIENTED_EDGE('',*,*,#24656,.T.);
#32551=ORIENTED_EDGE('',*,*,#24657,.T.);
#32552=ORIENTED_EDGE('',*,*,#24658,.T.);
#32553=ORIENTED_EDGE('',*,*,#24659,.T.);
#32554=ORIENTED_EDGE('',*,*,#24660,.T.);
#32555=ORIENTED_EDGE('',*,*,#24661,.T.);
#32556=ORIENTED_EDGE('',*,*,#24662,.T.);
#32557=ORIENTED_EDGE('',*,*,#24663,.T.);
#32558=ORIENTED_EDGE('',*,*,#24664,.T.);
#32559=ORIENTED_EDGE('',*,*,#24665,.T.);
#32560=ORIENTED_EDGE('',*,*,#24666,.T.);
#32561=ORIENTED_EDGE('',*,*,#24667,.T.);
#32562=ORIENTED_EDGE('',*,*,#24668,.T.);
#32563=ORIENTED_EDGE('',*,*,#24669,.T.);
#32564=ORIENTED_EDGE('',*,*,#24670,.T.);
#32565=ORIENTED_EDGE('',*,*,#24671,.T.);
#32566=ORIENTED_EDGE('',*,*,#24672,.T.);
#32567=ORIENTED_EDGE('',*,*,#24673,.T.);
#32568=ORIENTED_EDGE('',*,*,#24674,.T.);
#32569=ORIENTED_EDGE('',*,*,#24675,.T.);
#32570=ORIENTED_EDGE('',*,*,#24676,.T.);
#32571=ORIENTED_EDGE('',*,*,#24677,.T.);
#32572=ORIENTED_EDGE('',*,*,#24678,.T.);
#32573=ORIENTED_EDGE('',*,*,#24679,.T.);
#32574=ORIENTED_EDGE('',*,*,#24680,.T.);
#32575=ORIENTED_EDGE('',*,*,#24681,.T.);
#32576=ORIENTED_EDGE('',*,*,#24682,.T.);
#32577=ORIENTED_EDGE('',*,*,#24683,.T.);
#32578=ORIENTED_EDGE('',*,*,#24684,.T.);
#32579=ORIENTED_EDGE('',*,*,#24685,.T.);
#32580=ORIENTED_EDGE('',*,*,#24686,.T.);
#32581=ORIENTED_EDGE('',*,*,#24687,.T.);
#32582=ORIENTED_EDGE('',*,*,#24688,.T.);
#32583=ORIENTED_EDGE('',*,*,#24689,.T.);
#32584=ORIENTED_EDGE('',*,*,#24690,.T.);
#32585=ORIENTED_EDGE('',*,*,#24691,.T.);
#32586=ORIENTED_EDGE('',*,*,#24692,.T.);
#32587=ORIENTED_EDGE('',*,*,#24693,.T.);
#32588=ORIENTED_EDGE('',*,*,#24694,.T.);
#32589=ORIENTED_EDGE('',*,*,#24695,.T.);
#32590=ORIENTED_EDGE('',*,*,#24696,.T.);
#32591=ORIENTED_EDGE('',*,*,#24697,.T.);
#32592=ORIENTED_EDGE('',*,*,#24698,.T.);
#32593=ORIENTED_EDGE('',*,*,#24699,.T.);
#32594=ORIENTED_EDGE('',*,*,#24700,.T.);
#32595=ORIENTED_EDGE('',*,*,#24701,.T.);
#32596=ORIENTED_EDGE('',*,*,#24702,.T.);
#32597=ORIENTED_EDGE('',*,*,#24703,.T.);
#32598=ORIENTED_EDGE('',*,*,#24704,.T.);
#32599=ORIENTED_EDGE('',*,*,#24705,.T.);
#32600=ORIENTED_EDGE('',*,*,#24706,.T.);
#32601=ORIENTED_EDGE('',*,*,#24707,.T.);
#32602=ORIENTED_EDGE('',*,*,#24708,.T.);
#32603=ORIENTED_EDGE('',*,*,#24709,.T.);
#32604=ORIENTED_EDGE('',*,*,#24710,.T.);
#32605=ORIENTED_EDGE('',*,*,#24711,.T.);
#32606=ORIENTED_EDGE('',*,*,#24712,.T.);
#32607=ORIENTED_EDGE('',*,*,#24713,.T.);
#32608=ORIENTED_EDGE('',*,*,#24714,.T.);
#32609=ORIENTED_EDGE('',*,*,#24715,.T.);
#32610=ORIENTED_EDGE('',*,*,#24716,.T.);
#32611=ORIENTED_EDGE('',*,*,#24717,.T.);
#32612=ORIENTED_EDGE('',*,*,#24718,.T.);
#32613=ORIENTED_EDGE('',*,*,#24719,.T.);
#32614=ORIENTED_EDGE('',*,*,#24720,.T.);
#32615=ORIENTED_EDGE('',*,*,#24721,.T.);
#32616=ORIENTED_EDGE('',*,*,#24722,.T.);
#32617=ORIENTED_EDGE('',*,*,#24723,.T.);
#32618=ORIENTED_EDGE('',*,*,#24724,.T.);
#32619=ORIENTED_EDGE('',*,*,#24725,.T.);
#32620=ORIENTED_EDGE('',*,*,#24726,.T.);
#32621=ORIENTED_EDGE('',*,*,#24727,.T.);
#32622=ORIENTED_EDGE('',*,*,#24728,.T.);
#32623=ORIENTED_EDGE('',*,*,#24729,.T.);
#32624=ORIENTED_EDGE('',*,*,#24730,.T.);
#32625=ORIENTED_EDGE('',*,*,#24731,.T.);
#32626=ORIENTED_EDGE('',*,*,#24732,.T.);
#32627=ORIENTED_EDGE('',*,*,#24733,.T.);
#32628=ORIENTED_EDGE('',*,*,#24734,.T.);
#32629=ORIENTED_EDGE('',*,*,#24735,.T.);
#32630=ORIENTED_EDGE('',*,*,#24736,.T.);
#32631=ORIENTED_EDGE('',*,*,#24737,.T.);
#32632=ORIENTED_EDGE('',*,*,#24738,.T.);
#32633=ORIENTED_EDGE('',*,*,#24739,.T.);
#32634=ORIENTED_EDGE('',*,*,#24740,.T.);
#32635=ORIENTED_EDGE('',*,*,#24741,.T.);
#32636=ORIENTED_EDGE('',*,*,#24742,.T.);
#32637=ORIENTED_EDGE('',*,*,#24743,.T.);
#32638=ORIENTED_EDGE('',*,*,#24744,.T.);
#32639=ORIENTED_EDGE('',*,*,#24745,.T.);
#32640=ORIENTED_EDGE('',*,*,#24746,.T.);
#32641=ORIENTED_EDGE('',*,*,#24747,.T.);
#32642=ORIENTED_EDGE('',*,*,#24748,.T.);
#32643=ORIENTED_EDGE('',*,*,#24749,.T.);
#32644=ORIENTED_EDGE('',*,*,#24750,.T.);
#32645=ORIENTED_EDGE('',*,*,#24751,.T.);
#32646=ORIENTED_EDGE('',*,*,#24752,.T.);
#32647=ORIENTED_EDGE('',*,*,#24753,.T.);
#32648=ORIENTED_EDGE('',*,*,#24754,.T.);
#32649=ORIENTED_EDGE('',*,*,#24755,.T.);
#32650=ORIENTED_EDGE('',*,*,#24756,.T.);
#32651=ORIENTED_EDGE('',*,*,#24757,.T.);
#32652=ORIENTED_EDGE('',*,*,#24758,.T.);
#32653=ORIENTED_EDGE('',*,*,#24759,.T.);
#32654=ORIENTED_EDGE('',*,*,#24760,.T.);
#32655=ORIENTED_EDGE('',*,*,#24761,.T.);
#32656=ORIENTED_EDGE('',*,*,#24762,.T.);
#32657=ORIENTED_EDGE('',*,*,#24763,.T.);
#32658=ORIENTED_EDGE('',*,*,#24764,.T.);
#32659=ORIENTED_EDGE('',*,*,#24765,.T.);
#32660=ORIENTED_EDGE('',*,*,#24766,.T.);
#32661=ORIENTED_EDGE('',*,*,#24767,.T.);
#32662=ORIENTED_EDGE('',*,*,#24768,.T.);
#32663=ORIENTED_EDGE('',*,*,#24769,.T.);
#32664=ORIENTED_EDGE('',*,*,#24770,.T.);
#32665=ORIENTED_EDGE('',*,*,#24771,.T.);
#32666=ORIENTED_EDGE('',*,*,#24772,.T.);
#32667=ORIENTED_EDGE('',*,*,#24773,.T.);
#32668=ORIENTED_EDGE('',*,*,#24774,.T.);
#32669=ORIENTED_EDGE('',*,*,#24775,.T.);
#32670=ORIENTED_EDGE('',*,*,#24776,.T.);
#32671=ORIENTED_EDGE('',*,*,#24777,.T.);
#32672=ORIENTED_EDGE('',*,*,#24778,.T.);
#32673=ORIENTED_EDGE('',*,*,#24779,.T.);
#32674=ORIENTED_EDGE('',*,*,#24780,.T.);
#32675=ORIENTED_EDGE('',*,*,#24781,.T.);
#32676=ORIENTED_EDGE('',*,*,#24782,.T.);
#32677=ORIENTED_EDGE('',*,*,#24783,.T.);
#32678=ORIENTED_EDGE('',*,*,#24784,.T.);
#32679=ORIENTED_EDGE('',*,*,#24785,.T.);
#32680=ORIENTED_EDGE('',*,*,#24786,.T.);
#32681=ORIENTED_EDGE('',*,*,#24787,.T.);
#32682=ORIENTED_EDGE('',*,*,#24788,.T.);
#32683=ORIENTED_EDGE('',*,*,#24789,.T.);
#32684=ORIENTED_EDGE('',*,*,#24790,.T.);
#32685=ORIENTED_EDGE('',*,*,#24791,.T.);
#32686=ORIENTED_EDGE('',*,*,#24792,.T.);
#32687=ORIENTED_EDGE('',*,*,#24793,.T.);
#32688=ORIENTED_EDGE('',*,*,#24794,.T.);
#32689=ORIENTED_EDGE('',*,*,#24795,.T.);
#32690=ORIENTED_EDGE('',*,*,#24796,.T.);
#32691=ORIENTED_EDGE('',*,*,#24797,.T.);
#32692=ORIENTED_EDGE('',*,*,#24798,.T.);
#32693=ORIENTED_EDGE('',*,*,#24799,.T.);
#32694=ORIENTED_EDGE('',*,*,#24800,.T.);
#32695=ORIENTED_EDGE('',*,*,#24801,.T.);
#32696=ORIENTED_EDGE('',*,*,#24802,.T.);
#32697=ORIENTED_EDGE('',*,*,#24803,.T.);
#32698=ORIENTED_EDGE('',*,*,#24804,.T.);
#32699=ORIENTED_EDGE('',*,*,#24805,.T.);
#32700=ORIENTED_EDGE('',*,*,#24806,.T.);
#32701=ORIENTED_EDGE('',*,*,#24807,.T.);
#32702=ORIENTED_EDGE('',*,*,#24808,.T.);
#32703=ORIENTED_EDGE('',*,*,#24809,.T.);
#32704=ORIENTED_EDGE('',*,*,#24810,.T.);
#32705=ORIENTED_EDGE('',*,*,#24811,.T.);
#32706=ORIENTED_EDGE('',*,*,#24812,.T.);
#32707=ORIENTED_EDGE('',*,*,#24813,.T.);
#32708=ORIENTED_EDGE('',*,*,#24814,.T.);
#32709=ORIENTED_EDGE('',*,*,#24815,.T.);
#32710=ORIENTED_EDGE('',*,*,#24816,.T.);
#32711=ORIENTED_EDGE('',*,*,#24817,.T.);
#32712=ORIENTED_EDGE('',*,*,#24818,.T.);
#32713=ORIENTED_EDGE('',*,*,#24819,.T.);
#32714=ORIENTED_EDGE('',*,*,#24820,.T.);
#32715=ORIENTED_EDGE('',*,*,#24821,.T.);
#32716=ORIENTED_EDGE('',*,*,#24822,.T.);
#32717=ORIENTED_EDGE('',*,*,#24823,.T.);
#32718=ORIENTED_EDGE('',*,*,#24824,.T.);
#32719=ORIENTED_EDGE('',*,*,#24825,.T.);
#32720=ORIENTED_EDGE('',*,*,#24826,.T.);
#32721=ORIENTED_EDGE('',*,*,#24827,.T.);
#32722=ORIENTED_EDGE('',*,*,#24828,.T.);
#32723=ORIENTED_EDGE('',*,*,#24829,.T.);
#32724=ORIENTED_EDGE('',*,*,#24830,.T.);
#32725=ORIENTED_EDGE('',*,*,#24831,.T.);
#32726=ORIENTED_EDGE('',*,*,#24832,.T.);
#32727=ORIENTED_EDGE('',*,*,#24833,.T.);
#32728=ORIENTED_EDGE('',*,*,#24834,.T.);
#32729=ORIENTED_EDGE('',*,*,#24835,.T.);
#32730=ORIENTED_EDGE('',*,*,#24836,.T.);
#32731=ORIENTED_EDGE('',*,*,#24837,.T.);
#32732=ORIENTED_EDGE('',*,*,#24838,.T.);
#32733=ORIENTED_EDGE('',*,*,#24839,.T.);
#32734=ORIENTED_EDGE('',*,*,#24840,.T.);
#32735=ORIENTED_EDGE('',*,*,#24841,.T.);
#32736=ORIENTED_EDGE('',*,*,#24842,.T.);
#32737=ORIENTED_EDGE('',*,*,#24843,.T.);
#32738=ORIENTED_EDGE('',*,*,#24844,.T.);
#32739=ORIENTED_EDGE('',*,*,#24845,.T.);
#32740=ORIENTED_EDGE('',*,*,#24846,.T.);
#32741=ORIENTED_EDGE('',*,*,#24847,.T.);
#32742=ORIENTED_EDGE('',*,*,#24848,.T.);
#32743=ORIENTED_EDGE('',*,*,#24849,.T.);
#32744=ORIENTED_EDGE('',*,*,#24850,.T.);
#32745=ORIENTED_EDGE('',*,*,#24851,.T.);
#32746=ORIENTED_EDGE('',*,*,#24852,.T.);
#32747=ORIENTED_EDGE('',*,*,#24853,.T.);
#32748=ORIENTED_EDGE('',*,*,#24854,.T.);
#32749=ORIENTED_EDGE('',*,*,#24855,.T.);
#32750=ORIENTED_EDGE('',*,*,#24856,.T.);
#32751=ORIENTED_EDGE('',*,*,#24857,.T.);
#32752=ORIENTED_EDGE('',*,*,#24858,.T.);
#32753=ORIENTED_EDGE('',*,*,#24859,.T.);
#32754=ORIENTED_EDGE('',*,*,#24860,.T.);
#32755=ORIENTED_EDGE('',*,*,#24861,.T.);
#32756=ORIENTED_EDGE('',*,*,#24862,.T.);
#32757=ORIENTED_EDGE('',*,*,#24863,.T.);
#32758=ORIENTED_EDGE('',*,*,#24864,.T.);
#32759=ORIENTED_EDGE('',*,*,#24865,.T.);
#32760=ORIENTED_EDGE('',*,*,#24866,.T.);
#32761=ORIENTED_EDGE('',*,*,#24867,.T.);
#32762=ORIENTED_EDGE('',*,*,#24868,.T.);
#32763=ORIENTED_EDGE('',*,*,#24869,.T.);
#32764=ORIENTED_EDGE('',*,*,#24870,.T.);
#32765=ORIENTED_EDGE('',*,*,#24871,.T.);
#32766=ORIENTED_EDGE('',*,*,#24872,.T.);
#32767=ORIENTED_EDGE('',*,*,#24873,.T.);
#32768=ORIENTED_EDGE('',*,*,#24874,.T.);
#32769=ORIENTED_EDGE('',*,*,#24875,.T.);
#32770=ORIENTED_EDGE('',*,*,#24876,.T.);
#32771=ORIENTED_EDGE('',*,*,#24877,.T.);
#32772=ORIENTED_EDGE('',*,*,#24878,.T.);
#32773=ORIENTED_EDGE('',*,*,#24879,.T.);
#32774=ORIENTED_EDGE('',*,*,#24880,.T.);
#32775=ORIENTED_EDGE('',*,*,#24881,.T.);
#32776=ORIENTED_EDGE('',*,*,#24882,.T.);
#32777=ORIENTED_EDGE('',*,*,#24883,.T.);
#32778=ORIENTED_EDGE('',*,*,#24884,.T.);
#32779=ORIENTED_EDGE('',*,*,#24885,.T.);
#32780=ORIENTED_EDGE('',*,*,#24886,.T.);
#32781=ORIENTED_EDGE('',*,*,#24887,.T.);
#32782=ORIENTED_EDGE('',*,*,#24888,.T.);
#32783=ORIENTED_EDGE('',*,*,#24889,.T.);
#32784=ORIENTED_EDGE('',*,*,#24890,.T.);
#32785=ORIENTED_EDGE('',*,*,#24891,.T.);
#32786=ORIENTED_EDGE('',*,*,#24892,.T.);
#32787=ORIENTED_EDGE('',*,*,#24893,.T.);
#32788=ORIENTED_EDGE('',*,*,#24894,.T.);
#32789=ORIENTED_EDGE('',*,*,#24895,.T.);
#32790=ORIENTED_EDGE('',*,*,#24896,.T.);
#32791=ORIENTED_EDGE('',*,*,#24897,.T.);
#32792=ORIENTED_EDGE('',*,*,#24898,.T.);
#32793=ORIENTED_EDGE('',*,*,#24899,.T.);
#32794=ORIENTED_EDGE('',*,*,#24900,.T.);
#32795=ORIENTED_EDGE('',*,*,#24901,.T.);
#32796=ORIENTED_EDGE('',*,*,#24902,.T.);
#32797=ORIENTED_EDGE('',*,*,#24903,.T.);
#32798=ORIENTED_EDGE('',*,*,#24904,.T.);
#32799=ORIENTED_EDGE('',*,*,#24905,.T.);
#32800=ORIENTED_EDGE('',*,*,#24906,.T.);
#32801=ORIENTED_EDGE('',*,*,#24907,.T.);
#32802=ORIENTED_EDGE('',*,*,#24908,.T.);
#32803=ORIENTED_EDGE('',*,*,#24909,.T.);
#32804=ORIENTED_EDGE('',*,*,#24910,.T.);
#32805=ORIENTED_EDGE('',*,*,#24911,.T.);
#32806=ORIENTED_EDGE('',*,*,#24912,.T.);
#32807=ORIENTED_EDGE('',*,*,#24913,.T.);
#32808=ORIENTED_EDGE('',*,*,#24914,.T.);
#32809=ORIENTED_EDGE('',*,*,#24915,.T.);
#32810=ORIENTED_EDGE('',*,*,#24916,.T.);
#32811=ORIENTED_EDGE('',*,*,#24917,.T.);
#32812=ORIENTED_EDGE('',*,*,#24918,.T.);
#32813=ORIENTED_EDGE('',*,*,#24919,.T.);
#32814=ORIENTED_EDGE('',*,*,#24920,.T.);
#32815=ORIENTED_EDGE('',*,*,#24921,.T.);
#32816=ORIENTED_EDGE('',*,*,#24922,.T.);
#32817=ORIENTED_EDGE('',*,*,#24923,.T.);
#32818=ORIENTED_EDGE('',*,*,#24924,.T.);
#32819=ORIENTED_EDGE('',*,*,#24925,.T.);
#32820=ORIENTED_EDGE('',*,*,#24926,.T.);
#32821=ORIENTED_EDGE('',*,*,#24927,.T.);
#32822=ORIENTED_EDGE('',*,*,#24928,.T.);
#32823=ORIENTED_EDGE('',*,*,#24929,.T.);
#32824=ORIENTED_EDGE('',*,*,#24930,.T.);
#32825=ORIENTED_EDGE('',*,*,#24931,.T.);
#32826=ORIENTED_EDGE('',*,*,#24932,.T.);
#32827=ORIENTED_EDGE('',*,*,#24933,.T.);
#32828=ORIENTED_EDGE('',*,*,#24934,.T.);
#32829=ORIENTED_EDGE('',*,*,#24935,.T.);
#32830=ORIENTED_EDGE('',*,*,#24936,.T.);
#32831=ORIENTED_EDGE('',*,*,#24937,.T.);
#32832=ORIENTED_EDGE('',*,*,#24938,.T.);
#32833=ORIENTED_EDGE('',*,*,#24939,.T.);
#32834=ORIENTED_EDGE('',*,*,#24940,.T.);
#32835=ORIENTED_EDGE('',*,*,#24941,.T.);
#32836=ORIENTED_EDGE('',*,*,#24942,.T.);
#32837=ORIENTED_EDGE('',*,*,#24943,.T.);
#32838=ORIENTED_EDGE('',*,*,#24944,.T.);
#32839=ORIENTED_EDGE('',*,*,#24945,.T.);
#32840=ORIENTED_EDGE('',*,*,#24946,.T.);
#32841=ORIENTED_EDGE('',*,*,#24947,.T.);
#32842=ORIENTED_EDGE('',*,*,#24948,.T.);
#32843=ORIENTED_EDGE('',*,*,#24949,.T.);
#32844=ORIENTED_EDGE('',*,*,#24950,.T.);
#32845=ORIENTED_EDGE('',*,*,#24951,.T.);
#32846=ORIENTED_EDGE('',*,*,#24952,.T.);
#32847=ORIENTED_EDGE('',*,*,#24953,.T.);
#32848=ORIENTED_EDGE('',*,*,#24954,.T.);
#32849=ORIENTED_EDGE('',*,*,#24955,.T.);
#32850=ORIENTED_EDGE('',*,*,#24956,.T.);
#32851=ORIENTED_EDGE('',*,*,#24957,.T.);
#32852=ORIENTED_EDGE('',*,*,#24958,.T.);
#32853=ORIENTED_EDGE('',*,*,#24959,.T.);
#32854=ORIENTED_EDGE('',*,*,#24960,.T.);
#32855=ORIENTED_EDGE('',*,*,#24961,.T.);
#32856=ORIENTED_EDGE('',*,*,#24962,.T.);
#32857=ORIENTED_EDGE('',*,*,#24963,.T.);
#32858=ORIENTED_EDGE('',*,*,#24964,.T.);
#32859=ORIENTED_EDGE('',*,*,#24965,.T.);
#32860=ORIENTED_EDGE('',*,*,#24966,.T.);
#32861=ORIENTED_EDGE('',*,*,#24967,.T.);
#32862=ORIENTED_EDGE('',*,*,#24968,.T.);
#32863=ORIENTED_EDGE('',*,*,#24969,.T.);
#32864=ORIENTED_EDGE('',*,*,#24970,.T.);
#32865=ORIENTED_EDGE('',*,*,#24971,.T.);
#32866=ORIENTED_EDGE('',*,*,#24972,.T.);
#32867=ORIENTED_EDGE('',*,*,#24973,.T.);
#32868=ORIENTED_EDGE('',*,*,#24974,.T.);
#32869=ORIENTED_EDGE('',*,*,#24975,.T.);
#32870=ORIENTED_EDGE('',*,*,#24976,.T.);
#32871=ORIENTED_EDGE('',*,*,#24977,.T.);
#32872=ORIENTED_EDGE('',*,*,#24978,.T.);
#32873=ORIENTED_EDGE('',*,*,#24979,.T.);
#32874=ORIENTED_EDGE('',*,*,#24980,.T.);
#32875=ORIENTED_EDGE('',*,*,#24981,.T.);
#32876=ORIENTED_EDGE('',*,*,#24982,.T.);
#32877=ORIENTED_EDGE('',*,*,#24983,.T.);
#32878=ORIENTED_EDGE('',*,*,#24984,.T.);
#32879=ORIENTED_EDGE('',*,*,#24985,.T.);
#32880=ORIENTED_EDGE('',*,*,#24986,.T.);
#32881=ORIENTED_EDGE('',*,*,#24987,.T.);
#32882=ORIENTED_EDGE('',*,*,#24988,.T.);
#32883=ORIENTED_EDGE('',*,*,#24989,.T.);
#32884=ORIENTED_EDGE('',*,*,#24990,.T.);
#32885=ORIENTED_EDGE('',*,*,#24991,.T.);
#32886=ORIENTED_EDGE('',*,*,#24992,.T.);
#32887=ORIENTED_EDGE('',*,*,#24993,.T.);
#32888=ORIENTED_EDGE('',*,*,#24994,.T.);
#32889=ORIENTED_EDGE('',*,*,#24995,.T.);
#32890=ORIENTED_EDGE('',*,*,#24996,.T.);
#32891=ORIENTED_EDGE('',*,*,#24997,.T.);
#32892=ORIENTED_EDGE('',*,*,#24998,.T.);
#32893=ORIENTED_EDGE('',*,*,#24999,.T.);
#32894=ORIENTED_EDGE('',*,*,#25000,.T.);
#32895=ORIENTED_EDGE('',*,*,#25001,.T.);
#32896=ORIENTED_EDGE('',*,*,#25002,.T.);
#32897=ORIENTED_EDGE('',*,*,#25003,.T.);
#32898=ORIENTED_EDGE('',*,*,#25004,.T.);
#32899=ORIENTED_EDGE('',*,*,#25005,.T.);
#32900=ORIENTED_EDGE('',*,*,#25006,.T.);
#32901=ORIENTED_EDGE('',*,*,#25007,.T.);
#32902=ORIENTED_EDGE('',*,*,#25008,.T.);
#32903=ORIENTED_EDGE('',*,*,#25009,.T.);
#32904=ORIENTED_EDGE('',*,*,#25010,.T.);
#32905=ORIENTED_EDGE('',*,*,#25011,.T.);
#32906=ORIENTED_EDGE('',*,*,#25012,.T.);
#32907=ORIENTED_EDGE('',*,*,#25013,.T.);
#32908=ORIENTED_EDGE('',*,*,#25014,.T.);
#32909=ORIENTED_EDGE('',*,*,#25015,.T.);
#32910=ORIENTED_EDGE('',*,*,#25016,.T.);
#32911=ORIENTED_EDGE('',*,*,#25017,.T.);
#32912=ORIENTED_EDGE('',*,*,#25018,.T.);
#32913=ORIENTED_EDGE('',*,*,#25019,.T.);
#32914=ORIENTED_EDGE('',*,*,#25020,.T.);
#32915=ORIENTED_EDGE('',*,*,#25021,.T.);
#32916=ORIENTED_EDGE('',*,*,#25022,.T.);
#32917=ORIENTED_EDGE('',*,*,#25023,.T.);
#32918=ORIENTED_EDGE('',*,*,#25024,.T.);
#32919=ORIENTED_EDGE('',*,*,#25025,.T.);
#32920=ORIENTED_EDGE('',*,*,#25026,.T.);
#32921=ORIENTED_EDGE('',*,*,#25027,.T.);
#32922=ORIENTED_EDGE('',*,*,#25028,.T.);
#32923=ORIENTED_EDGE('',*,*,#25029,.T.);
#32924=ORIENTED_EDGE('',*,*,#25030,.T.);
#32925=ORIENTED_EDGE('',*,*,#25031,.T.);
#32926=ORIENTED_EDGE('',*,*,#25032,.T.);
#32927=ORIENTED_EDGE('',*,*,#25033,.T.);
#32928=ORIENTED_EDGE('',*,*,#25034,.T.);
#32929=ORIENTED_EDGE('',*,*,#25035,.T.);
#32930=ORIENTED_EDGE('',*,*,#25036,.T.);
#32931=ORIENTED_EDGE('',*,*,#25037,.T.);
#32932=ORIENTED_EDGE('',*,*,#25038,.T.);
#32933=ORIENTED_EDGE('',*,*,#25039,.T.);
#32934=ORIENTED_EDGE('',*,*,#25040,.T.);
#32935=ORIENTED_EDGE('',*,*,#25041,.T.);
#32936=ORIENTED_EDGE('',*,*,#25042,.T.);
#32937=ORIENTED_EDGE('',*,*,#25043,.T.);
#32938=ORIENTED_EDGE('',*,*,#25044,.T.);
#32939=ORIENTED_EDGE('',*,*,#25045,.T.);
#32940=ORIENTED_EDGE('',*,*,#25046,.T.);
#32941=ORIENTED_EDGE('',*,*,#25047,.T.);
#32942=ORIENTED_EDGE('',*,*,#25048,.T.);
#32943=ORIENTED_EDGE('',*,*,#25049,.T.);
#32944=ORIENTED_EDGE('',*,*,#25050,.T.);
#32945=ORIENTED_EDGE('',*,*,#25051,.T.);
#32946=ORIENTED_EDGE('',*,*,#25052,.T.);
#32947=ORIENTED_EDGE('',*,*,#25053,.T.);
#32948=ORIENTED_EDGE('',*,*,#25054,.T.);
#32949=ORIENTED_EDGE('',*,*,#25055,.T.);
#32950=ORIENTED_EDGE('',*,*,#25056,.T.);
#32951=ORIENTED_EDGE('',*,*,#25057,.T.);
#32952=ORIENTED_EDGE('',*,*,#25058,.T.);
#32953=ORIENTED_EDGE('',*,*,#25059,.T.);
#32954=ORIENTED_EDGE('',*,*,#25060,.T.);
#32955=ORIENTED_EDGE('',*,*,#25061,.T.);
#32956=ORIENTED_EDGE('',*,*,#25062,.T.);
#32957=ORIENTED_EDGE('',*,*,#25063,.T.);
#32958=ORIENTED_EDGE('',*,*,#25064,.T.);
#32959=ORIENTED_EDGE('',*,*,#25065,.T.);
#32960=ORIENTED_EDGE('',*,*,#25066,.T.);
#32961=ORIENTED_EDGE('',*,*,#25067,.T.);
#32962=ORIENTED_EDGE('',*,*,#25068,.T.);
#32963=ORIENTED_EDGE('',*,*,#25069,.T.);
#32964=ORIENTED_EDGE('',*,*,#25070,.T.);
#32965=ORIENTED_EDGE('',*,*,#25071,.T.);
#32966=ORIENTED_EDGE('',*,*,#25072,.T.);
#32967=ORIENTED_EDGE('',*,*,#25073,.T.);
#32968=ORIENTED_EDGE('',*,*,#25074,.T.);
#32969=ORIENTED_EDGE('',*,*,#25075,.T.);
#32970=ORIENTED_EDGE('',*,*,#25076,.T.);
#32971=ORIENTED_EDGE('',*,*,#25077,.T.);
#32972=ORIENTED_EDGE('',*,*,#25078,.T.);
#32973=ORIENTED_EDGE('',*,*,#25079,.T.);
#32974=ORIENTED_EDGE('',*,*,#25080,.T.);
#32975=ORIENTED_EDGE('',*,*,#25081,.T.);
#32976=ORIENTED_EDGE('',*,*,#25082,.T.);
#32977=ORIENTED_EDGE('',*,*,#25083,.T.);
#32978=ORIENTED_EDGE('',*,*,#25084,.T.);
#32979=ORIENTED_EDGE('',*,*,#25085,.T.);
#32980=ORIENTED_EDGE('',*,*,#25086,.T.);
#32981=ORIENTED_EDGE('',*,*,#25087,.T.);
#32982=ORIENTED_EDGE('',*,*,#25088,.T.);
#32983=ORIENTED_EDGE('',*,*,#25089,.T.);
#32984=ORIENTED_EDGE('',*,*,#25090,.T.);
#32985=ORIENTED_EDGE('',*,*,#25091,.T.);
#32986=ORIENTED_EDGE('',*,*,#25092,.T.);
#32987=ORIENTED_EDGE('',*,*,#25093,.T.);
#32988=ORIENTED_EDGE('',*,*,#25094,.T.);
#32989=ORIENTED_EDGE('',*,*,#25095,.T.);
#32990=ORIENTED_EDGE('',*,*,#25096,.T.);
#32991=ORIENTED_EDGE('',*,*,#25097,.T.);
#32992=ORIENTED_EDGE('',*,*,#25098,.T.);
#32993=ORIENTED_EDGE('',*,*,#25099,.T.);
#32994=ORIENTED_EDGE('',*,*,#25100,.T.);
#32995=ORIENTED_EDGE('',*,*,#25101,.T.);
#32996=ORIENTED_EDGE('',*,*,#25102,.T.);
#32997=ORIENTED_EDGE('',*,*,#25103,.T.);
#32998=ORIENTED_EDGE('',*,*,#25104,.T.);
#32999=ORIENTED_EDGE('',*,*,#25105,.T.);
#33000=ORIENTED_EDGE('',*,*,#25106,.T.);
#33001=ORIENTED_EDGE('',*,*,#25107,.T.);
#33002=ORIENTED_EDGE('',*,*,#25108,.T.);
#33003=ORIENTED_EDGE('',*,*,#25109,.T.);
#33004=ORIENTED_EDGE('',*,*,#25110,.T.);
#33005=ORIENTED_EDGE('',*,*,#25111,.T.);
#33006=ORIENTED_EDGE('',*,*,#25112,.T.);
#33007=ORIENTED_EDGE('',*,*,#25113,.T.);
#33008=ORIENTED_EDGE('',*,*,#25114,.T.);
#33009=ORIENTED_EDGE('',*,*,#25115,.T.);
#33010=ORIENTED_EDGE('',*,*,#25116,.T.);
#33011=ORIENTED_EDGE('',*,*,#25117,.T.);
#33012=ORIENTED_EDGE('',*,*,#25118,.T.);
#33013=ORIENTED_EDGE('',*,*,#25119,.T.);
#33014=ORIENTED_EDGE('',*,*,#25120,.T.);
#33015=ORIENTED_EDGE('',*,*,#25121,.T.);
#33016=ORIENTED_EDGE('',*,*,#25122,.T.);
#33017=ORIENTED_EDGE('',*,*,#25123,.T.);
#33018=ORIENTED_EDGE('',*,*,#25124,.T.);
#33019=ORIENTED_EDGE('',*,*,#25125,.T.);
#33020=ORIENTED_EDGE('',*,*,#25126,.T.);
#33021=ORIENTED_EDGE('',*,*,#25127,.T.);
#33022=ORIENTED_EDGE('',*,*,#25128,.T.);
#33023=ORIENTED_EDGE('',*,*,#25129,.T.);
#33024=ORIENTED_EDGE('',*,*,#25130,.T.);
#33025=ORIENTED_EDGE('',*,*,#25131,.T.);
#33026=ORIENTED_EDGE('',*,*,#25132,.T.);
#33027=ORIENTED_EDGE('',*,*,#25133,.T.);
#33028=ORIENTED_EDGE('',*,*,#25134,.T.);
#33029=ORIENTED_EDGE('',*,*,#25135,.T.);
#33030=ORIENTED_EDGE('',*,*,#25136,.T.);
#33031=ORIENTED_EDGE('',*,*,#25137,.T.);
#33032=ORIENTED_EDGE('',*,*,#25138,.T.);
#33033=ORIENTED_EDGE('',*,*,#25139,.T.);
#33034=ORIENTED_EDGE('',*,*,#25140,.T.);
#33035=ORIENTED_EDGE('',*,*,#25141,.T.);
#33036=ORIENTED_EDGE('',*,*,#25142,.T.);
#33037=ORIENTED_EDGE('',*,*,#25143,.T.);
#33038=ORIENTED_EDGE('',*,*,#25144,.T.);
#33039=ORIENTED_EDGE('',*,*,#25145,.T.);
#33040=ORIENTED_EDGE('',*,*,#25146,.T.);
#33041=ORIENTED_EDGE('',*,*,#25147,.T.);
#33042=ORIENTED_EDGE('',*,*,#25148,.T.);
#33043=ORIENTED_EDGE('',*,*,#25149,.T.);
#33044=ORIENTED_EDGE('',*,*,#25150,.T.);
#33045=ORIENTED_EDGE('',*,*,#25151,.T.);
#33046=ORIENTED_EDGE('',*,*,#25152,.T.);
#33047=ORIENTED_EDGE('',*,*,#25153,.T.);
#33048=ORIENTED_EDGE('',*,*,#25154,.T.);
#33049=ORIENTED_EDGE('',*,*,#25155,.T.);
#33050=ORIENTED_EDGE('',*,*,#25156,.T.);
#33051=ORIENTED_EDGE('',*,*,#25157,.T.);
#33052=ORIENTED_EDGE('',*,*,#25158,.T.);
#33053=ORIENTED_EDGE('',*,*,#25159,.T.);
#33054=ORIENTED_EDGE('',*,*,#25160,.T.);
#33055=ORIENTED_EDGE('',*,*,#25161,.T.);
#33056=ORIENTED_EDGE('',*,*,#25162,.T.);
#33057=ORIENTED_EDGE('',*,*,#25163,.T.);
#33058=ORIENTED_EDGE('',*,*,#25164,.T.);
#33059=ORIENTED_EDGE('',*,*,#25165,.T.);
#33060=ORIENTED_EDGE('',*,*,#25166,.T.);
#33061=ORIENTED_EDGE('',*,*,#25167,.T.);
#33062=ORIENTED_EDGE('',*,*,#25168,.T.);
#33063=ORIENTED_EDGE('',*,*,#25169,.T.);
#33064=ORIENTED_EDGE('',*,*,#25170,.T.);
#33065=ORIENTED_EDGE('',*,*,#25171,.T.);
#33066=ORIENTED_EDGE('',*,*,#25172,.T.);
#33067=ORIENTED_EDGE('',*,*,#25173,.T.);
#33068=ORIENTED_EDGE('',*,*,#25174,.T.);
#33069=ORIENTED_EDGE('',*,*,#25175,.T.);
#33070=ORIENTED_EDGE('',*,*,#25176,.T.);
#33071=ORIENTED_EDGE('',*,*,#25177,.T.);
#33072=ORIENTED_EDGE('',*,*,#25178,.T.);
#33073=ORIENTED_EDGE('',*,*,#25179,.T.);
#33074=ORIENTED_EDGE('',*,*,#25180,.T.);
#33075=ORIENTED_EDGE('',*,*,#25181,.T.);
#33076=ORIENTED_EDGE('',*,*,#25182,.T.);
#33077=ORIENTED_EDGE('',*,*,#25183,.T.);
#33078=ORIENTED_EDGE('',*,*,#25184,.T.);
#33079=ORIENTED_EDGE('',*,*,#25185,.T.);
#33080=ORIENTED_EDGE('',*,*,#25186,.T.);
#33081=ORIENTED_EDGE('',*,*,#25187,.T.);
#33082=ORIENTED_EDGE('',*,*,#25188,.T.);
#33083=ORIENTED_EDGE('',*,*,#25189,.T.);
#33084=ORIENTED_EDGE('',*,*,#25190,.T.);
#33085=ORIENTED_EDGE('',*,*,#25191,.T.);
#33086=ORIENTED_EDGE('',*,*,#25192,.T.);
#33087=ORIENTED_EDGE('',*,*,#25193,.T.);
#33088=ORIENTED_EDGE('',*,*,#25194,.T.);
#33089=ORIENTED_EDGE('',*,*,#25195,.T.);
#33090=ORIENTED_EDGE('',*,*,#25196,.T.);
#33091=ORIENTED_EDGE('',*,*,#25197,.T.);
#33092=ORIENTED_EDGE('',*,*,#25198,.T.);
#33093=ORIENTED_EDGE('',*,*,#25199,.T.);
#33094=ORIENTED_EDGE('',*,*,#25200,.T.);
#33095=ORIENTED_EDGE('',*,*,#25201,.T.);
#33096=ORIENTED_EDGE('',*,*,#25202,.T.);
#33097=ORIENTED_EDGE('',*,*,#25203,.T.);
#33098=ORIENTED_EDGE('',*,*,#25204,.T.);
#33099=ORIENTED_EDGE('',*,*,#25205,.T.);
#33100=ORIENTED_EDGE('',*,*,#25206,.T.);
#33101=ORIENTED_EDGE('',*,*,#25207,.T.);
#33102=ORIENTED_EDGE('',*,*,#25208,.T.);
#33103=ORIENTED_EDGE('',*,*,#25209,.T.);
#33104=ORIENTED_EDGE('',*,*,#25210,.T.);
#33105=ORIENTED_EDGE('',*,*,#25211,.T.);
#33106=ORIENTED_EDGE('',*,*,#25212,.T.);
#33107=ORIENTED_EDGE('',*,*,#25213,.T.);
#33108=ORIENTED_EDGE('',*,*,#25214,.T.);
#33109=ORIENTED_EDGE('',*,*,#25215,.T.);
#33110=ORIENTED_EDGE('',*,*,#25216,.T.);
#33111=ORIENTED_EDGE('',*,*,#25217,.T.);
#33112=ORIENTED_EDGE('',*,*,#25218,.T.);
#33113=ORIENTED_EDGE('',*,*,#25219,.T.);
#33114=ORIENTED_EDGE('',*,*,#25220,.T.);
#33115=ORIENTED_EDGE('',*,*,#25221,.T.);
#33116=ORIENTED_EDGE('',*,*,#25222,.T.);
#33117=ORIENTED_EDGE('',*,*,#25223,.T.);
#33118=ORIENTED_EDGE('',*,*,#25224,.T.);
#33119=ORIENTED_EDGE('',*,*,#25225,.T.);
#33120=ORIENTED_EDGE('',*,*,#25226,.T.);
#33121=ORIENTED_EDGE('',*,*,#25227,.T.);
#33122=ORIENTED_EDGE('',*,*,#25228,.T.);
#33123=ORIENTED_EDGE('',*,*,#25229,.T.);
#33124=ORIENTED_EDGE('',*,*,#25230,.T.);
#33125=ORIENTED_EDGE('',*,*,#25231,.T.);
#33126=ORIENTED_EDGE('',*,*,#25232,.T.);
#33127=ORIENTED_EDGE('',*,*,#25233,.T.);
#33128=ORIENTED_EDGE('',*,*,#25234,.T.);
#33129=ORIENTED_EDGE('',*,*,#25235,.T.);
#33130=ORIENTED_EDGE('',*,*,#25236,.T.);
#33131=ORIENTED_EDGE('',*,*,#25237,.T.);
#33132=ORIENTED_EDGE('',*,*,#25238,.T.);
#33133=ORIENTED_EDGE('',*,*,#25239,.T.);
#33134=ORIENTED_EDGE('',*,*,#25240,.T.);
#33135=ORIENTED_EDGE('',*,*,#25241,.T.);
#33136=ORIENTED_EDGE('',*,*,#25242,.T.);
#33137=ORIENTED_EDGE('',*,*,#25243,.T.);
#33138=ORIENTED_EDGE('',*,*,#25244,.T.);
#33139=ORIENTED_EDGE('',*,*,#25245,.T.);
#33140=ORIENTED_EDGE('',*,*,#25246,.T.);
#33141=ORIENTED_EDGE('',*,*,#25247,.T.);
#33142=ORIENTED_EDGE('',*,*,#25248,.T.);
#33143=ORIENTED_EDGE('',*,*,#25249,.T.);
#33144=ORIENTED_EDGE('',*,*,#25250,.T.);
#33145=ORIENTED_EDGE('',*,*,#25251,.T.);
#33146=ORIENTED_EDGE('',*,*,#25252,.T.);
#33147=ORIENTED_EDGE('',*,*,#25253,.T.);
#33148=ORIENTED_EDGE('',*,*,#25254,.T.);
#33149=ORIENTED_EDGE('',*,*,#25255,.T.);
#33150=ORIENTED_EDGE('',*,*,#25256,.T.);
#33151=ORIENTED_EDGE('',*,*,#25257,.T.);
#33152=ORIENTED_EDGE('',*,*,#25258,.T.);
#33153=ORIENTED_EDGE('',*,*,#25259,.T.);
#33154=ORIENTED_EDGE('',*,*,#25260,.T.);
#33155=ORIENTED_EDGE('',*,*,#25261,.T.);
#33156=ORIENTED_EDGE('',*,*,#25262,.T.);
#33157=ORIENTED_EDGE('',*,*,#25263,.T.);
#33158=ORIENTED_EDGE('',*,*,#25264,.T.);
#33159=ORIENTED_EDGE('',*,*,#25265,.T.);
#33160=ORIENTED_EDGE('',*,*,#25266,.T.);
#33161=ORIENTED_EDGE('',*,*,#25267,.T.);
#33162=ORIENTED_EDGE('',*,*,#25268,.T.);
#33163=ORIENTED_EDGE('',*,*,#25269,.T.);
#33164=ORIENTED_EDGE('',*,*,#25270,.T.);
#33165=ORIENTED_EDGE('',*,*,#25271,.T.);
#33166=ORIENTED_EDGE('',*,*,#25272,.T.);
#33167=ORIENTED_EDGE('',*,*,#25273,.T.);
#33168=ORIENTED_EDGE('',*,*,#25274,.T.);
#33169=ORIENTED_EDGE('',*,*,#25275,.T.);
#33170=ORIENTED_EDGE('',*,*,#25276,.T.);
#33171=ORIENTED_EDGE('',*,*,#25277,.T.);
#33172=ORIENTED_EDGE('',*,*,#25278,.T.);
#33173=ORIENTED_EDGE('',*,*,#25279,.T.);
#33174=ORIENTED_EDGE('',*,*,#25280,.T.);
#33175=ORIENTED_EDGE('',*,*,#25281,.T.);
#33176=ORIENTED_EDGE('',*,*,#25282,.T.);
#33177=ORIENTED_EDGE('',*,*,#25283,.T.);
#33178=ORIENTED_EDGE('',*,*,#25284,.T.);
#33179=ORIENTED_EDGE('',*,*,#25285,.T.);
#33180=ORIENTED_EDGE('',*,*,#25286,.T.);
#33181=ORIENTED_EDGE('',*,*,#25287,.T.);
#33182=ORIENTED_EDGE('',*,*,#25288,.T.);
#33183=ORIENTED_EDGE('',*,*,#25289,.T.);
#33184=ORIENTED_EDGE('',*,*,#25290,.T.);
#33185=ORIENTED_EDGE('',*,*,#25291,.T.);
#33186=ORIENTED_EDGE('',*,*,#25292,.T.);
#33187=ORIENTED_EDGE('',*,*,#25293,.T.);
#33188=ORIENTED_EDGE('',*,*,#25294,.T.);
#33189=ORIENTED_EDGE('',*,*,#25295,.T.);
#33190=ORIENTED_EDGE('',*,*,#25296,.T.);
#33191=ORIENTED_EDGE('',*,*,#25297,.T.);
#33192=ORIENTED_EDGE('',*,*,#25298,.T.);
#33193=ORIENTED_EDGE('',*,*,#25299,.T.);
#33194=ORIENTED_EDGE('',*,*,#25300,.T.);
#33195=ORIENTED_EDGE('',*,*,#25301,.T.);
#33196=ORIENTED_EDGE('',*,*,#25302,.T.);
#33197=ORIENTED_EDGE('',*,*,#25303,.T.);
#33198=ORIENTED_EDGE('',*,*,#25304,.T.);
#33199=ORIENTED_EDGE('',*,*,#25305,.T.);
#33200=ORIENTED_EDGE('',*,*,#25306,.T.);
#33201=ORIENTED_EDGE('',*,*,#25307,.T.);
#33202=ORIENTED_EDGE('',*,*,#25308,.T.);
#33203=ORIENTED_EDGE('',*,*,#25309,.T.);
#33204=ORIENTED_EDGE('',*,*,#25310,.T.);
#33205=ORIENTED_EDGE('',*,*,#25311,.T.);
#33206=ORIENTED_EDGE('',*,*,#25312,.T.);
#33207=ORIENTED_EDGE('',*,*,#25313,.T.);
#33208=ORIENTED_EDGE('',*,*,#25314,.T.);
#33209=ORIENTED_EDGE('',*,*,#25315,.T.);
#33210=ORIENTED_EDGE('',*,*,#25316,.T.);
#33211=ORIENTED_EDGE('',*,*,#25317,.T.);
#33212=ORIENTED_EDGE('',*,*,#25318,.T.);
#33213=ORIENTED_EDGE('',*,*,#25319,.T.);
#33214=ORIENTED_EDGE('',*,*,#25320,.T.);
#33215=ORIENTED_EDGE('',*,*,#25321,.T.);
#33216=ORIENTED_EDGE('',*,*,#25322,.T.);
#33217=ORIENTED_EDGE('',*,*,#25323,.T.);
#33218=ORIENTED_EDGE('',*,*,#25324,.T.);
#33219=ORIENTED_EDGE('',*,*,#25325,.T.);
#33220=ORIENTED_EDGE('',*,*,#25326,.T.);
#33221=ORIENTED_EDGE('',*,*,#25327,.T.);
#33222=ORIENTED_EDGE('',*,*,#25328,.T.);
#33223=ORIENTED_EDGE('',*,*,#25329,.T.);
#33224=ORIENTED_EDGE('',*,*,#25330,.T.);
#33225=ORIENTED_EDGE('',*,*,#25331,.T.);
#33226=ORIENTED_EDGE('',*,*,#25332,.T.);
#33227=ORIENTED_EDGE('',*,*,#25333,.T.);
#33228=ORIENTED_EDGE('',*,*,#25334,.T.);
#33229=ORIENTED_EDGE('',*,*,#25335,.T.);
#33230=ORIENTED_EDGE('',*,*,#25336,.T.);
#33231=ORIENTED_EDGE('',*,*,#25337,.T.);
#33232=ORIENTED_EDGE('',*,*,#25338,.T.);
#33233=ORIENTED_EDGE('',*,*,#25339,.T.);
#33234=ORIENTED_EDGE('',*,*,#25340,.T.);
#33235=ORIENTED_EDGE('',*,*,#25341,.T.);
#33236=ORIENTED_EDGE('',*,*,#25342,.T.);
#33237=ORIENTED_EDGE('',*,*,#25343,.T.);
#33238=ORIENTED_EDGE('',*,*,#25344,.T.);
#33239=ORIENTED_EDGE('',*,*,#25345,.T.);
#33240=ORIENTED_EDGE('',*,*,#25346,.T.);
#33241=ORIENTED_EDGE('',*,*,#25347,.T.);
#33242=ORIENTED_EDGE('',*,*,#25348,.T.);
#33243=ORIENTED_EDGE('',*,*,#25349,.T.);
#33244=ORIENTED_EDGE('',*,*,#25350,.T.);
#33245=ORIENTED_EDGE('',*,*,#25351,.T.);
#33246=ORIENTED_EDGE('',*,*,#25352,.T.);
#33247=ORIENTED_EDGE('',*,*,#25353,.T.);
#33248=ORIENTED_EDGE('',*,*,#25354,.T.);
#33249=ORIENTED_EDGE('',*,*,#25355,.T.);
#33250=ORIENTED_EDGE('',*,*,#25356,.T.);
#33251=ORIENTED_EDGE('',*,*,#25357,.T.);
#33252=ORIENTED_EDGE('',*,*,#25358,.T.);
#33253=ORIENTED_EDGE('',*,*,#25359,.T.);
#33254=ORIENTED_EDGE('',*,*,#25360,.T.);
#33255=ORIENTED_EDGE('',*,*,#25361,.T.);
#33256=ORIENTED_EDGE('',*,*,#24239,.T.);
#33257=ORIENTED_EDGE('',*,*,#25362,.F.);
#33258=ORIENTED_EDGE('',*,*,#25356,.F.);
#33259=ORIENTED_EDGE('',*,*,#25363,.T.);
#33260=ORIENTED_EDGE('',*,*,#24240,.T.);
#33261=ORIENTED_EDGE('',*,*,#25361,.F.);
#33262=ORIENTED_EDGE('',*,*,#25355,.F.);
#33263=ORIENTED_EDGE('',*,*,#25364,.T.);
#33264=ORIENTED_EDGE('',*,*,#24241,.T.);
#33265=ORIENTED_EDGE('',*,*,#25363,.F.);
#33266=ORIENTED_EDGE('',*,*,#25360,.F.);
#33267=ORIENTED_EDGE('',*,*,#25365,.T.);
#33268=ORIENTED_EDGE('',*,*,#24242,.T.);
#33269=ORIENTED_EDGE('',*,*,#25364,.F.);
#33270=ORIENTED_EDGE('',*,*,#25359,.F.);
#33271=ORIENTED_EDGE('',*,*,#25366,.T.);
#33272=ORIENTED_EDGE('',*,*,#24243,.T.);
#33273=ORIENTED_EDGE('',*,*,#25365,.F.);
#33274=ORIENTED_EDGE('',*,*,#25358,.F.);
#33275=ORIENTED_EDGE('',*,*,#25362,.T.);
#33276=ORIENTED_EDGE('',*,*,#24244,.T.);
#33277=ORIENTED_EDGE('',*,*,#25366,.F.);
#33278=ORIENTED_EDGE('',*,*,#25357,.F.);
#33279=ORIENTED_EDGE('',*,*,#25367,.T.);
#33280=ORIENTED_EDGE('',*,*,#24233,.T.);
#33281=ORIENTED_EDGE('',*,*,#25368,.F.);
#33282=ORIENTED_EDGE('',*,*,#25350,.F.);
#33283=ORIENTED_EDGE('',*,*,#25369,.T.);
#33284=ORIENTED_EDGE('',*,*,#24234,.T.);
#33285=ORIENTED_EDGE('',*,*,#25367,.F.);
#33286=ORIENTED_EDGE('',*,*,#25349,.F.);
#33287=ORIENTED_EDGE('',*,*,#25370,.T.);
#33288=ORIENTED_EDGE('',*,*,#24235,.T.);
#33289=ORIENTED_EDGE('',*,*,#25369,.F.);
#33290=ORIENTED_EDGE('',*,*,#25354,.F.);
#33291=ORIENTED_EDGE('',*,*,#25371,.T.);
#33292=ORIENTED_EDGE('',*,*,#24236,.T.);
#33293=ORIENTED_EDGE('',*,*,#25370,.F.);
#33294=ORIENTED_EDGE('',*,*,#25353,.F.);
#33295=ORIENTED_EDGE('',*,*,#25372,.T.);
#33296=ORIENTED_EDGE('',*,*,#24237,.T.);
#33297=ORIENTED_EDGE('',*,*,#25371,.F.);
#33298=ORIENTED_EDGE('',*,*,#25352,.F.);
#33299=ORIENTED_EDGE('',*,*,#25368,.T.);
#33300=ORIENTED_EDGE('',*,*,#24238,.T.);
#33301=ORIENTED_EDGE('',*,*,#25372,.F.);
#33302=ORIENTED_EDGE('',*,*,#25351,.F.);
#33303=ORIENTED_EDGE('',*,*,#25373,.T.);
#33304=ORIENTED_EDGE('',*,*,#24227,.T.);
#33305=ORIENTED_EDGE('',*,*,#25374,.F.);
#33306=ORIENTED_EDGE('',*,*,#25344,.F.);
#33307=ORIENTED_EDGE('',*,*,#25375,.T.);
#33308=ORIENTED_EDGE('',*,*,#24228,.T.);
#33309=ORIENTED_EDGE('',*,*,#25373,.F.);
#33310=ORIENTED_EDGE('',*,*,#25343,.F.);
#33311=ORIENTED_EDGE('',*,*,#25376,.T.);
#33312=ORIENTED_EDGE('',*,*,#24229,.T.);
#33313=ORIENTED_EDGE('',*,*,#25375,.F.);
#33314=ORIENTED_EDGE('',*,*,#25348,.F.);
#33315=ORIENTED_EDGE('',*,*,#25377,.T.);
#33316=ORIENTED_EDGE('',*,*,#24230,.T.);
#33317=ORIENTED_EDGE('',*,*,#25376,.F.);
#33318=ORIENTED_EDGE('',*,*,#25347,.F.);
#33319=ORIENTED_EDGE('',*,*,#25378,.T.);
#33320=ORIENTED_EDGE('',*,*,#24231,.T.);
#33321=ORIENTED_EDGE('',*,*,#25377,.F.);
#33322=ORIENTED_EDGE('',*,*,#25346,.F.);
#33323=ORIENTED_EDGE('',*,*,#25374,.T.);
#33324=ORIENTED_EDGE('',*,*,#24232,.T.);
#33325=ORIENTED_EDGE('',*,*,#25378,.F.);
#33326=ORIENTED_EDGE('',*,*,#25345,.F.);
#33327=ORIENTED_EDGE('',*,*,#25379,.T.);
#33328=ORIENTED_EDGE('',*,*,#24221,.T.);
#33329=ORIENTED_EDGE('',*,*,#25380,.F.);
#33330=ORIENTED_EDGE('',*,*,#25338,.F.);
#33331=ORIENTED_EDGE('',*,*,#25381,.T.);
#33332=ORIENTED_EDGE('',*,*,#24222,.T.);
#33333=ORIENTED_EDGE('',*,*,#25379,.F.);
#33334=ORIENTED_EDGE('',*,*,#25337,.F.);
#33335=ORIENTED_EDGE('',*,*,#25382,.T.);
#33336=ORIENTED_EDGE('',*,*,#24223,.T.);
#33337=ORIENTED_EDGE('',*,*,#25381,.F.);
#33338=ORIENTED_EDGE('',*,*,#25342,.F.);
#33339=ORIENTED_EDGE('',*,*,#25383,.T.);
#33340=ORIENTED_EDGE('',*,*,#24224,.T.);
#33341=ORIENTED_EDGE('',*,*,#25382,.F.);
#33342=ORIENTED_EDGE('',*,*,#25341,.F.);
#33343=ORIENTED_EDGE('',*,*,#25384,.T.);
#33344=ORIENTED_EDGE('',*,*,#24225,.T.);
#33345=ORIENTED_EDGE('',*,*,#25383,.F.);
#33346=ORIENTED_EDGE('',*,*,#25340,.F.);
#33347=ORIENTED_EDGE('',*,*,#25380,.T.);
#33348=ORIENTED_EDGE('',*,*,#24226,.T.);
#33349=ORIENTED_EDGE('',*,*,#25384,.F.);
#33350=ORIENTED_EDGE('',*,*,#25339,.F.);
#33351=ORIENTED_EDGE('',*,*,#25385,.T.);
#33352=ORIENTED_EDGE('',*,*,#24215,.T.);
#33353=ORIENTED_EDGE('',*,*,#25386,.F.);
#33354=ORIENTED_EDGE('',*,*,#25332,.F.);
#33355=ORIENTED_EDGE('',*,*,#25387,.T.);
#33356=ORIENTED_EDGE('',*,*,#24216,.T.);
#33357=ORIENTED_EDGE('',*,*,#25385,.F.);
#33358=ORIENTED_EDGE('',*,*,#25331,.F.);
#33359=ORIENTED_EDGE('',*,*,#25388,.T.);
#33360=ORIENTED_EDGE('',*,*,#24217,.T.);
#33361=ORIENTED_EDGE('',*,*,#25387,.F.);
#33362=ORIENTED_EDGE('',*,*,#25336,.F.);
#33363=ORIENTED_EDGE('',*,*,#25389,.T.);
#33364=ORIENTED_EDGE('',*,*,#24218,.T.);
#33365=ORIENTED_EDGE('',*,*,#25388,.F.);
#33366=ORIENTED_EDGE('',*,*,#25335,.F.);
#33367=ORIENTED_EDGE('',*,*,#25390,.T.);
#33368=ORIENTED_EDGE('',*,*,#24219,.T.);
#33369=ORIENTED_EDGE('',*,*,#25389,.F.);
#33370=ORIENTED_EDGE('',*,*,#25334,.F.);
#33371=ORIENTED_EDGE('',*,*,#25386,.T.);
#33372=ORIENTED_EDGE('',*,*,#24220,.T.);
#33373=ORIENTED_EDGE('',*,*,#25390,.F.);
#33374=ORIENTED_EDGE('',*,*,#25333,.F.);
#33375=ORIENTED_EDGE('',*,*,#25391,.T.);
#33376=ORIENTED_EDGE('',*,*,#24209,.T.);
#33377=ORIENTED_EDGE('',*,*,#25392,.F.);
#33378=ORIENTED_EDGE('',*,*,#25326,.F.);
#33379=ORIENTED_EDGE('',*,*,#25393,.T.);
#33380=ORIENTED_EDGE('',*,*,#24210,.T.);
#33381=ORIENTED_EDGE('',*,*,#25391,.F.);
#33382=ORIENTED_EDGE('',*,*,#25325,.F.);
#33383=ORIENTED_EDGE('',*,*,#25394,.T.);
#33384=ORIENTED_EDGE('',*,*,#24211,.T.);
#33385=ORIENTED_EDGE('',*,*,#25393,.F.);
#33386=ORIENTED_EDGE('',*,*,#25330,.F.);
#33387=ORIENTED_EDGE('',*,*,#25395,.T.);
#33388=ORIENTED_EDGE('',*,*,#24212,.T.);
#33389=ORIENTED_EDGE('',*,*,#25394,.F.);
#33390=ORIENTED_EDGE('',*,*,#25329,.F.);
#33391=ORIENTED_EDGE('',*,*,#25396,.T.);
#33392=ORIENTED_EDGE('',*,*,#24213,.T.);
#33393=ORIENTED_EDGE('',*,*,#25395,.F.);
#33394=ORIENTED_EDGE('',*,*,#25328,.F.);
#33395=ORIENTED_EDGE('',*,*,#25392,.T.);
#33396=ORIENTED_EDGE('',*,*,#24214,.T.);
#33397=ORIENTED_EDGE('',*,*,#25396,.F.);
#33398=ORIENTED_EDGE('',*,*,#25327,.F.);
#33399=ORIENTED_EDGE('',*,*,#25397,.T.);
#33400=ORIENTED_EDGE('',*,*,#24203,.T.);
#33401=ORIENTED_EDGE('',*,*,#25398,.F.);
#33402=ORIENTED_EDGE('',*,*,#25320,.F.);
#33403=ORIENTED_EDGE('',*,*,#25399,.T.);
#33404=ORIENTED_EDGE('',*,*,#24204,.T.);
#33405=ORIENTED_EDGE('',*,*,#25397,.F.);
#33406=ORIENTED_EDGE('',*,*,#25319,.F.);
#33407=ORIENTED_EDGE('',*,*,#25400,.T.);
#33408=ORIENTED_EDGE('',*,*,#24205,.T.);
#33409=ORIENTED_EDGE('',*,*,#25399,.F.);
#33410=ORIENTED_EDGE('',*,*,#25324,.F.);
#33411=ORIENTED_EDGE('',*,*,#25401,.T.);
#33412=ORIENTED_EDGE('',*,*,#24206,.T.);
#33413=ORIENTED_EDGE('',*,*,#25400,.F.);
#33414=ORIENTED_EDGE('',*,*,#25323,.F.);
#33415=ORIENTED_EDGE('',*,*,#25402,.T.);
#33416=ORIENTED_EDGE('',*,*,#24207,.T.);
#33417=ORIENTED_EDGE('',*,*,#25401,.F.);
#33418=ORIENTED_EDGE('',*,*,#25322,.F.);
#33419=ORIENTED_EDGE('',*,*,#25398,.T.);
#33420=ORIENTED_EDGE('',*,*,#24208,.T.);
#33421=ORIENTED_EDGE('',*,*,#25402,.F.);
#33422=ORIENTED_EDGE('',*,*,#25321,.F.);
#33423=ORIENTED_EDGE('',*,*,#25403,.T.);
#33424=ORIENTED_EDGE('',*,*,#24197,.T.);
#33425=ORIENTED_EDGE('',*,*,#25404,.F.);
#33426=ORIENTED_EDGE('',*,*,#25314,.F.);
#33427=ORIENTED_EDGE('',*,*,#25405,.T.);
#33428=ORIENTED_EDGE('',*,*,#24198,.T.);
#33429=ORIENTED_EDGE('',*,*,#25403,.F.);
#33430=ORIENTED_EDGE('',*,*,#25313,.F.);
#33431=ORIENTED_EDGE('',*,*,#25406,.T.);
#33432=ORIENTED_EDGE('',*,*,#24199,.T.);
#33433=ORIENTED_EDGE('',*,*,#25405,.F.);
#33434=ORIENTED_EDGE('',*,*,#25318,.F.);
#33435=ORIENTED_EDGE('',*,*,#25407,.T.);
#33436=ORIENTED_EDGE('',*,*,#24200,.T.);
#33437=ORIENTED_EDGE('',*,*,#25406,.F.);
#33438=ORIENTED_EDGE('',*,*,#25317,.F.);
#33439=ORIENTED_EDGE('',*,*,#25408,.T.);
#33440=ORIENTED_EDGE('',*,*,#24201,.T.);
#33441=ORIENTED_EDGE('',*,*,#25407,.F.);
#33442=ORIENTED_EDGE('',*,*,#25316,.F.);
#33443=ORIENTED_EDGE('',*,*,#25404,.T.);
#33444=ORIENTED_EDGE('',*,*,#24202,.T.);
#33445=ORIENTED_EDGE('',*,*,#25408,.F.);
#33446=ORIENTED_EDGE('',*,*,#25315,.F.);
#33447=ORIENTED_EDGE('',*,*,#25409,.T.);
#33448=ORIENTED_EDGE('',*,*,#24191,.T.);
#33449=ORIENTED_EDGE('',*,*,#25410,.F.);
#33450=ORIENTED_EDGE('',*,*,#25308,.F.);
#33451=ORIENTED_EDGE('',*,*,#25411,.T.);
#33452=ORIENTED_EDGE('',*,*,#24192,.T.);
#33453=ORIENTED_EDGE('',*,*,#25409,.F.);
#33454=ORIENTED_EDGE('',*,*,#25307,.F.);
#33455=ORIENTED_EDGE('',*,*,#25412,.T.);
#33456=ORIENTED_EDGE('',*,*,#24193,.T.);
#33457=ORIENTED_EDGE('',*,*,#25411,.F.);
#33458=ORIENTED_EDGE('',*,*,#25312,.F.);
#33459=ORIENTED_EDGE('',*,*,#25413,.T.);
#33460=ORIENTED_EDGE('',*,*,#24194,.T.);
#33461=ORIENTED_EDGE('',*,*,#25412,.F.);
#33462=ORIENTED_EDGE('',*,*,#25311,.F.);
#33463=ORIENTED_EDGE('',*,*,#25414,.T.);
#33464=ORIENTED_EDGE('',*,*,#24195,.T.);
#33465=ORIENTED_EDGE('',*,*,#25413,.F.);
#33466=ORIENTED_EDGE('',*,*,#25310,.F.);
#33467=ORIENTED_EDGE('',*,*,#25410,.T.);
#33468=ORIENTED_EDGE('',*,*,#24196,.T.);
#33469=ORIENTED_EDGE('',*,*,#25414,.F.);
#33470=ORIENTED_EDGE('',*,*,#25309,.F.);
#33471=ORIENTED_EDGE('',*,*,#25415,.T.);
#33472=ORIENTED_EDGE('',*,*,#24185,.T.);
#33473=ORIENTED_EDGE('',*,*,#25416,.F.);
#33474=ORIENTED_EDGE('',*,*,#25302,.F.);
#33475=ORIENTED_EDGE('',*,*,#25417,.T.);
#33476=ORIENTED_EDGE('',*,*,#24186,.T.);
#33477=ORIENTED_EDGE('',*,*,#25415,.F.);
#33478=ORIENTED_EDGE('',*,*,#25301,.F.);
#33479=ORIENTED_EDGE('',*,*,#25418,.T.);
#33480=ORIENTED_EDGE('',*,*,#24187,.T.);
#33481=ORIENTED_EDGE('',*,*,#25417,.F.);
#33482=ORIENTED_EDGE('',*,*,#25306,.F.);
#33483=ORIENTED_EDGE('',*,*,#25419,.T.);
#33484=ORIENTED_EDGE('',*,*,#24188,.T.);
#33485=ORIENTED_EDGE('',*,*,#25418,.F.);
#33486=ORIENTED_EDGE('',*,*,#25305,.F.);
#33487=ORIENTED_EDGE('',*,*,#25420,.T.);
#33488=ORIENTED_EDGE('',*,*,#24189,.T.);
#33489=ORIENTED_EDGE('',*,*,#25419,.F.);
#33490=ORIENTED_EDGE('',*,*,#25304,.F.);
#33491=ORIENTED_EDGE('',*,*,#25416,.T.);
#33492=ORIENTED_EDGE('',*,*,#24190,.T.);
#33493=ORIENTED_EDGE('',*,*,#25420,.F.);
#33494=ORIENTED_EDGE('',*,*,#25303,.F.);
#33495=ORIENTED_EDGE('',*,*,#25421,.T.);
#33496=ORIENTED_EDGE('',*,*,#24179,.T.);
#33497=ORIENTED_EDGE('',*,*,#25422,.F.);
#33498=ORIENTED_EDGE('',*,*,#25296,.F.);
#33499=ORIENTED_EDGE('',*,*,#25423,.T.);
#33500=ORIENTED_EDGE('',*,*,#24180,.T.);
#33501=ORIENTED_EDGE('',*,*,#25421,.F.);
#33502=ORIENTED_EDGE('',*,*,#25295,.F.);
#33503=ORIENTED_EDGE('',*,*,#25424,.T.);
#33504=ORIENTED_EDGE('',*,*,#24181,.T.);
#33505=ORIENTED_EDGE('',*,*,#25423,.F.);
#33506=ORIENTED_EDGE('',*,*,#25300,.F.);
#33507=ORIENTED_EDGE('',*,*,#25425,.T.);
#33508=ORIENTED_EDGE('',*,*,#24182,.T.);
#33509=ORIENTED_EDGE('',*,*,#25424,.F.);
#33510=ORIENTED_EDGE('',*,*,#25299,.F.);
#33511=ORIENTED_EDGE('',*,*,#25426,.T.);
#33512=ORIENTED_EDGE('',*,*,#24183,.T.);
#33513=ORIENTED_EDGE('',*,*,#25425,.F.);
#33514=ORIENTED_EDGE('',*,*,#25298,.F.);
#33515=ORIENTED_EDGE('',*,*,#25422,.T.);
#33516=ORIENTED_EDGE('',*,*,#24184,.T.);
#33517=ORIENTED_EDGE('',*,*,#25426,.F.);
#33518=ORIENTED_EDGE('',*,*,#25297,.F.);
#33519=ORIENTED_EDGE('',*,*,#25427,.T.);
#33520=ORIENTED_EDGE('',*,*,#24173,.T.);
#33521=ORIENTED_EDGE('',*,*,#25428,.F.);
#33522=ORIENTED_EDGE('',*,*,#25290,.F.);
#33523=ORIENTED_EDGE('',*,*,#25429,.T.);
#33524=ORIENTED_EDGE('',*,*,#24174,.T.);
#33525=ORIENTED_EDGE('',*,*,#25427,.F.);
#33526=ORIENTED_EDGE('',*,*,#25289,.F.);
#33527=ORIENTED_EDGE('',*,*,#25430,.T.);
#33528=ORIENTED_EDGE('',*,*,#24175,.T.);
#33529=ORIENTED_EDGE('',*,*,#25429,.F.);
#33530=ORIENTED_EDGE('',*,*,#25294,.F.);
#33531=ORIENTED_EDGE('',*,*,#25431,.T.);
#33532=ORIENTED_EDGE('',*,*,#24176,.T.);
#33533=ORIENTED_EDGE('',*,*,#25430,.F.);
#33534=ORIENTED_EDGE('',*,*,#25293,.F.);
#33535=ORIENTED_EDGE('',*,*,#25432,.T.);
#33536=ORIENTED_EDGE('',*,*,#24177,.T.);
#33537=ORIENTED_EDGE('',*,*,#25431,.F.);
#33538=ORIENTED_EDGE('',*,*,#25292,.F.);
#33539=ORIENTED_EDGE('',*,*,#25428,.T.);
#33540=ORIENTED_EDGE('',*,*,#24178,.T.);
#33541=ORIENTED_EDGE('',*,*,#25432,.F.);
#33542=ORIENTED_EDGE('',*,*,#25291,.F.);
#33543=ORIENTED_EDGE('',*,*,#25433,.T.);
#33544=ORIENTED_EDGE('',*,*,#24167,.T.);
#33545=ORIENTED_EDGE('',*,*,#25434,.F.);
#33546=ORIENTED_EDGE('',*,*,#25284,.F.);
#33547=ORIENTED_EDGE('',*,*,#25435,.T.);
#33548=ORIENTED_EDGE('',*,*,#24168,.T.);
#33549=ORIENTED_EDGE('',*,*,#25433,.F.);
#33550=ORIENTED_EDGE('',*,*,#25283,.F.);
#33551=ORIENTED_EDGE('',*,*,#25436,.T.);
#33552=ORIENTED_EDGE('',*,*,#24169,.T.);
#33553=ORIENTED_EDGE('',*,*,#25435,.F.);
#33554=ORIENTED_EDGE('',*,*,#25288,.F.);
#33555=ORIENTED_EDGE('',*,*,#25437,.T.);
#33556=ORIENTED_EDGE('',*,*,#24170,.T.);
#33557=ORIENTED_EDGE('',*,*,#25436,.F.);
#33558=ORIENTED_EDGE('',*,*,#25287,.F.);
#33559=ORIENTED_EDGE('',*,*,#25438,.T.);
#33560=ORIENTED_EDGE('',*,*,#24171,.T.);
#33561=ORIENTED_EDGE('',*,*,#25437,.F.);
#33562=ORIENTED_EDGE('',*,*,#25286,.F.);
#33563=ORIENTED_EDGE('',*,*,#25434,.T.);
#33564=ORIENTED_EDGE('',*,*,#24172,.T.);
#33565=ORIENTED_EDGE('',*,*,#25438,.F.);
#33566=ORIENTED_EDGE('',*,*,#25285,.F.);
#33567=ORIENTED_EDGE('',*,*,#25439,.T.);
#33568=ORIENTED_EDGE('',*,*,#24161,.T.);
#33569=ORIENTED_EDGE('',*,*,#25440,.F.);
#33570=ORIENTED_EDGE('',*,*,#25278,.F.);
#33571=ORIENTED_EDGE('',*,*,#25441,.T.);
#33572=ORIENTED_EDGE('',*,*,#24162,.T.);
#33573=ORIENTED_EDGE('',*,*,#25439,.F.);
#33574=ORIENTED_EDGE('',*,*,#25277,.F.);
#33575=ORIENTED_EDGE('',*,*,#25442,.T.);
#33576=ORIENTED_EDGE('',*,*,#24163,.T.);
#33577=ORIENTED_EDGE('',*,*,#25441,.F.);
#33578=ORIENTED_EDGE('',*,*,#25282,.F.);
#33579=ORIENTED_EDGE('',*,*,#25443,.T.);
#33580=ORIENTED_EDGE('',*,*,#24164,.T.);
#33581=ORIENTED_EDGE('',*,*,#25442,.F.);
#33582=ORIENTED_EDGE('',*,*,#25281,.F.);
#33583=ORIENTED_EDGE('',*,*,#25444,.T.);
#33584=ORIENTED_EDGE('',*,*,#24165,.T.);
#33585=ORIENTED_EDGE('',*,*,#25443,.F.);
#33586=ORIENTED_EDGE('',*,*,#25280,.F.);
#33587=ORIENTED_EDGE('',*,*,#25440,.T.);
#33588=ORIENTED_EDGE('',*,*,#24166,.T.);
#33589=ORIENTED_EDGE('',*,*,#25444,.F.);
#33590=ORIENTED_EDGE('',*,*,#25279,.F.);
#33591=ORIENTED_EDGE('',*,*,#25445,.T.);
#33592=ORIENTED_EDGE('',*,*,#24155,.T.);
#33593=ORIENTED_EDGE('',*,*,#25446,.F.);
#33594=ORIENTED_EDGE('',*,*,#25272,.F.);
#33595=ORIENTED_EDGE('',*,*,#25447,.T.);
#33596=ORIENTED_EDGE('',*,*,#24156,.T.);
#33597=ORIENTED_EDGE('',*,*,#25445,.F.);
#33598=ORIENTED_EDGE('',*,*,#25271,.F.);
#33599=ORIENTED_EDGE('',*,*,#25448,.T.);
#33600=ORIENTED_EDGE('',*,*,#24157,.T.);
#33601=ORIENTED_EDGE('',*,*,#25447,.F.);
#33602=ORIENTED_EDGE('',*,*,#25276,.F.);
#33603=ORIENTED_EDGE('',*,*,#25449,.T.);
#33604=ORIENTED_EDGE('',*,*,#24158,.T.);
#33605=ORIENTED_EDGE('',*,*,#25448,.F.);
#33606=ORIENTED_EDGE('',*,*,#25275,.F.);
#33607=ORIENTED_EDGE('',*,*,#25450,.T.);
#33608=ORIENTED_EDGE('',*,*,#24159,.T.);
#33609=ORIENTED_EDGE('',*,*,#25449,.F.);
#33610=ORIENTED_EDGE('',*,*,#25274,.F.);
#33611=ORIENTED_EDGE('',*,*,#25446,.T.);
#33612=ORIENTED_EDGE('',*,*,#24160,.T.);
#33613=ORIENTED_EDGE('',*,*,#25450,.F.);
#33614=ORIENTED_EDGE('',*,*,#25273,.F.);
#33615=ORIENTED_EDGE('',*,*,#25451,.T.);
#33616=ORIENTED_EDGE('',*,*,#24149,.T.);
#33617=ORIENTED_EDGE('',*,*,#25452,.F.);
#33618=ORIENTED_EDGE('',*,*,#25266,.F.);
#33619=ORIENTED_EDGE('',*,*,#25453,.T.);
#33620=ORIENTED_EDGE('',*,*,#24150,.T.);
#33621=ORIENTED_EDGE('',*,*,#25451,.F.);
#33622=ORIENTED_EDGE('',*,*,#25265,.F.);
#33623=ORIENTED_EDGE('',*,*,#25454,.T.);
#33624=ORIENTED_EDGE('',*,*,#24151,.T.);
#33625=ORIENTED_EDGE('',*,*,#25453,.F.);
#33626=ORIENTED_EDGE('',*,*,#25270,.F.);
#33627=ORIENTED_EDGE('',*,*,#25455,.T.);
#33628=ORIENTED_EDGE('',*,*,#24152,.T.);
#33629=ORIENTED_EDGE('',*,*,#25454,.F.);
#33630=ORIENTED_EDGE('',*,*,#25269,.F.);
#33631=ORIENTED_EDGE('',*,*,#25456,.T.);
#33632=ORIENTED_EDGE('',*,*,#24153,.T.);
#33633=ORIENTED_EDGE('',*,*,#25455,.F.);
#33634=ORIENTED_EDGE('',*,*,#25268,.F.);
#33635=ORIENTED_EDGE('',*,*,#25452,.T.);
#33636=ORIENTED_EDGE('',*,*,#24154,.T.);
#33637=ORIENTED_EDGE('',*,*,#25456,.F.);
#33638=ORIENTED_EDGE('',*,*,#25267,.F.);
#33639=ORIENTED_EDGE('',*,*,#25457,.T.);
#33640=ORIENTED_EDGE('',*,*,#24143,.T.);
#33641=ORIENTED_EDGE('',*,*,#25458,.F.);
#33642=ORIENTED_EDGE('',*,*,#25260,.F.);
#33643=ORIENTED_EDGE('',*,*,#25459,.T.);
#33644=ORIENTED_EDGE('',*,*,#24144,.T.);
#33645=ORIENTED_EDGE('',*,*,#25457,.F.);
#33646=ORIENTED_EDGE('',*,*,#25259,.F.);
#33647=ORIENTED_EDGE('',*,*,#25460,.T.);
#33648=ORIENTED_EDGE('',*,*,#24145,.T.);
#33649=ORIENTED_EDGE('',*,*,#25459,.F.);
#33650=ORIENTED_EDGE('',*,*,#25264,.F.);
#33651=ORIENTED_EDGE('',*,*,#25461,.T.);
#33652=ORIENTED_EDGE('',*,*,#24146,.T.);
#33653=ORIENTED_EDGE('',*,*,#25460,.F.);
#33654=ORIENTED_EDGE('',*,*,#25263,.F.);
#33655=ORIENTED_EDGE('',*,*,#25462,.T.);
#33656=ORIENTED_EDGE('',*,*,#24147,.T.);
#33657=ORIENTED_EDGE('',*,*,#25461,.F.);
#33658=ORIENTED_EDGE('',*,*,#25262,.F.);
#33659=ORIENTED_EDGE('',*,*,#25458,.T.);
#33660=ORIENTED_EDGE('',*,*,#24148,.T.);
#33661=ORIENTED_EDGE('',*,*,#25462,.F.);
#33662=ORIENTED_EDGE('',*,*,#25261,.F.);
#33663=ORIENTED_EDGE('',*,*,#25463,.T.);
#33664=ORIENTED_EDGE('',*,*,#24137,.T.);
#33665=ORIENTED_EDGE('',*,*,#25464,.F.);
#33666=ORIENTED_EDGE('',*,*,#25254,.F.);
#33667=ORIENTED_EDGE('',*,*,#25465,.T.);
#33668=ORIENTED_EDGE('',*,*,#24138,.T.);
#33669=ORIENTED_EDGE('',*,*,#25463,.F.);
#33670=ORIENTED_EDGE('',*,*,#25253,.F.);
#33671=ORIENTED_EDGE('',*,*,#25466,.T.);
#33672=ORIENTED_EDGE('',*,*,#24139,.T.);
#33673=ORIENTED_EDGE('',*,*,#25465,.F.);
#33674=ORIENTED_EDGE('',*,*,#25258,.F.);
#33675=ORIENTED_EDGE('',*,*,#25467,.T.);
#33676=ORIENTED_EDGE('',*,*,#24140,.T.);
#33677=ORIENTED_EDGE('',*,*,#25466,.F.);
#33678=ORIENTED_EDGE('',*,*,#25257,.F.);
#33679=ORIENTED_EDGE('',*,*,#25468,.T.);
#33680=ORIENTED_EDGE('',*,*,#24141,.T.);
#33681=ORIENTED_EDGE('',*,*,#25467,.F.);
#33682=ORIENTED_EDGE('',*,*,#25256,.F.);
#33683=ORIENTED_EDGE('',*,*,#25464,.T.);
#33684=ORIENTED_EDGE('',*,*,#24142,.T.);
#33685=ORIENTED_EDGE('',*,*,#25468,.F.);
#33686=ORIENTED_EDGE('',*,*,#25255,.F.);
#33687=ORIENTED_EDGE('',*,*,#25469,.T.);
#33688=ORIENTED_EDGE('',*,*,#24131,.T.);
#33689=ORIENTED_EDGE('',*,*,#25470,.F.);
#33690=ORIENTED_EDGE('',*,*,#25248,.F.);
#33691=ORIENTED_EDGE('',*,*,#25471,.T.);
#33692=ORIENTED_EDGE('',*,*,#24132,.T.);
#33693=ORIENTED_EDGE('',*,*,#25469,.F.);
#33694=ORIENTED_EDGE('',*,*,#25247,.F.);
#33695=ORIENTED_EDGE('',*,*,#25472,.T.);
#33696=ORIENTED_EDGE('',*,*,#24133,.T.);
#33697=ORIENTED_EDGE('',*,*,#25471,.F.);
#33698=ORIENTED_EDGE('',*,*,#25252,.F.);
#33699=ORIENTED_EDGE('',*,*,#25473,.T.);
#33700=ORIENTED_EDGE('',*,*,#24134,.T.);
#33701=ORIENTED_EDGE('',*,*,#25472,.F.);
#33702=ORIENTED_EDGE('',*,*,#25251,.F.);
#33703=ORIENTED_EDGE('',*,*,#25474,.T.);
#33704=ORIENTED_EDGE('',*,*,#24135,.T.);
#33705=ORIENTED_EDGE('',*,*,#25473,.F.);
#33706=ORIENTED_EDGE('',*,*,#25250,.F.);
#33707=ORIENTED_EDGE('',*,*,#25470,.T.);
#33708=ORIENTED_EDGE('',*,*,#24136,.T.);
#33709=ORIENTED_EDGE('',*,*,#25474,.F.);
#33710=ORIENTED_EDGE('',*,*,#25249,.F.);
#33711=ORIENTED_EDGE('',*,*,#25475,.T.);
#33712=ORIENTED_EDGE('',*,*,#24125,.T.);
#33713=ORIENTED_EDGE('',*,*,#25476,.F.);
#33714=ORIENTED_EDGE('',*,*,#25242,.F.);
#33715=ORIENTED_EDGE('',*,*,#25477,.T.);
#33716=ORIENTED_EDGE('',*,*,#24126,.T.);
#33717=ORIENTED_EDGE('',*,*,#25475,.F.);
#33718=ORIENTED_EDGE('',*,*,#25241,.F.);
#33719=ORIENTED_EDGE('',*,*,#25478,.T.);
#33720=ORIENTED_EDGE('',*,*,#24127,.T.);
#33721=ORIENTED_EDGE('',*,*,#25477,.F.);
#33722=ORIENTED_EDGE('',*,*,#25246,.F.);
#33723=ORIENTED_EDGE('',*,*,#25479,.T.);
#33724=ORIENTED_EDGE('',*,*,#24128,.T.);
#33725=ORIENTED_EDGE('',*,*,#25478,.F.);
#33726=ORIENTED_EDGE('',*,*,#25245,.F.);
#33727=ORIENTED_EDGE('',*,*,#25480,.T.);
#33728=ORIENTED_EDGE('',*,*,#24129,.T.);
#33729=ORIENTED_EDGE('',*,*,#25479,.F.);
#33730=ORIENTED_EDGE('',*,*,#25244,.F.);
#33731=ORIENTED_EDGE('',*,*,#25476,.T.);
#33732=ORIENTED_EDGE('',*,*,#24130,.T.);
#33733=ORIENTED_EDGE('',*,*,#25480,.F.);
#33734=ORIENTED_EDGE('',*,*,#25243,.F.);
#33735=ORIENTED_EDGE('',*,*,#25481,.T.);
#33736=ORIENTED_EDGE('',*,*,#24119,.T.);
#33737=ORIENTED_EDGE('',*,*,#25482,.F.);
#33738=ORIENTED_EDGE('',*,*,#25236,.F.);
#33739=ORIENTED_EDGE('',*,*,#25483,.T.);
#33740=ORIENTED_EDGE('',*,*,#24120,.T.);
#33741=ORIENTED_EDGE('',*,*,#25481,.F.);
#33742=ORIENTED_EDGE('',*,*,#25235,.F.);
#33743=ORIENTED_EDGE('',*,*,#25484,.T.);
#33744=ORIENTED_EDGE('',*,*,#24121,.T.);
#33745=ORIENTED_EDGE('',*,*,#25483,.F.);
#33746=ORIENTED_EDGE('',*,*,#25240,.F.);
#33747=ORIENTED_EDGE('',*,*,#25485,.T.);
#33748=ORIENTED_EDGE('',*,*,#24122,.T.);
#33749=ORIENTED_EDGE('',*,*,#25484,.F.);
#33750=ORIENTED_EDGE('',*,*,#25239,.F.);
#33751=ORIENTED_EDGE('',*,*,#25486,.T.);
#33752=ORIENTED_EDGE('',*,*,#24123,.T.);
#33753=ORIENTED_EDGE('',*,*,#25485,.F.);
#33754=ORIENTED_EDGE('',*,*,#25238,.F.);
#33755=ORIENTED_EDGE('',*,*,#25482,.T.);
#33756=ORIENTED_EDGE('',*,*,#24124,.T.);
#33757=ORIENTED_EDGE('',*,*,#25486,.F.);
#33758=ORIENTED_EDGE('',*,*,#25237,.F.);
#33759=ORIENTED_EDGE('',*,*,#25487,.T.);
#33760=ORIENTED_EDGE('',*,*,#24113,.T.);
#33761=ORIENTED_EDGE('',*,*,#25488,.F.);
#33762=ORIENTED_EDGE('',*,*,#25230,.F.);
#33763=ORIENTED_EDGE('',*,*,#25489,.T.);
#33764=ORIENTED_EDGE('',*,*,#24114,.T.);
#33765=ORIENTED_EDGE('',*,*,#25487,.F.);
#33766=ORIENTED_EDGE('',*,*,#25229,.F.);
#33767=ORIENTED_EDGE('',*,*,#25490,.T.);
#33768=ORIENTED_EDGE('',*,*,#24115,.T.);
#33769=ORIENTED_EDGE('',*,*,#25489,.F.);
#33770=ORIENTED_EDGE('',*,*,#25234,.F.);
#33771=ORIENTED_EDGE('',*,*,#25491,.T.);
#33772=ORIENTED_EDGE('',*,*,#24116,.T.);
#33773=ORIENTED_EDGE('',*,*,#25490,.F.);
#33774=ORIENTED_EDGE('',*,*,#25233,.F.);
#33775=ORIENTED_EDGE('',*,*,#25492,.T.);
#33776=ORIENTED_EDGE('',*,*,#24117,.T.);
#33777=ORIENTED_EDGE('',*,*,#25491,.F.);
#33778=ORIENTED_EDGE('',*,*,#25232,.F.);
#33779=ORIENTED_EDGE('',*,*,#25488,.T.);
#33780=ORIENTED_EDGE('',*,*,#24118,.T.);
#33781=ORIENTED_EDGE('',*,*,#25492,.F.);
#33782=ORIENTED_EDGE('',*,*,#25231,.F.);
#33783=ORIENTED_EDGE('',*,*,#25493,.T.);
#33784=ORIENTED_EDGE('',*,*,#24107,.T.);
#33785=ORIENTED_EDGE('',*,*,#25494,.F.);
#33786=ORIENTED_EDGE('',*,*,#25224,.F.);
#33787=ORIENTED_EDGE('',*,*,#25495,.T.);
#33788=ORIENTED_EDGE('',*,*,#24108,.T.);
#33789=ORIENTED_EDGE('',*,*,#25493,.F.);
#33790=ORIENTED_EDGE('',*,*,#25223,.F.);
#33791=ORIENTED_EDGE('',*,*,#25496,.T.);
#33792=ORIENTED_EDGE('',*,*,#24109,.T.);
#33793=ORIENTED_EDGE('',*,*,#25495,.F.);
#33794=ORIENTED_EDGE('',*,*,#25228,.F.);
#33795=ORIENTED_EDGE('',*,*,#25497,.T.);
#33796=ORIENTED_EDGE('',*,*,#24110,.T.);
#33797=ORIENTED_EDGE('',*,*,#25496,.F.);
#33798=ORIENTED_EDGE('',*,*,#25227,.F.);
#33799=ORIENTED_EDGE('',*,*,#25498,.T.);
#33800=ORIENTED_EDGE('',*,*,#24111,.T.);
#33801=ORIENTED_EDGE('',*,*,#25497,.F.);
#33802=ORIENTED_EDGE('',*,*,#25226,.F.);
#33803=ORIENTED_EDGE('',*,*,#25494,.T.);
#33804=ORIENTED_EDGE('',*,*,#24112,.T.);
#33805=ORIENTED_EDGE('',*,*,#25498,.F.);
#33806=ORIENTED_EDGE('',*,*,#25225,.F.);
#33807=ORIENTED_EDGE('',*,*,#25499,.T.);
#33808=ORIENTED_EDGE('',*,*,#24101,.T.);
#33809=ORIENTED_EDGE('',*,*,#25500,.F.);
#33810=ORIENTED_EDGE('',*,*,#25218,.F.);
#33811=ORIENTED_EDGE('',*,*,#25501,.T.);
#33812=ORIENTED_EDGE('',*,*,#24102,.T.);
#33813=ORIENTED_EDGE('',*,*,#25499,.F.);
#33814=ORIENTED_EDGE('',*,*,#25217,.F.);
#33815=ORIENTED_EDGE('',*,*,#25502,.T.);
#33816=ORIENTED_EDGE('',*,*,#24103,.T.);
#33817=ORIENTED_EDGE('',*,*,#25501,.F.);
#33818=ORIENTED_EDGE('',*,*,#25222,.F.);
#33819=ORIENTED_EDGE('',*,*,#25503,.T.);
#33820=ORIENTED_EDGE('',*,*,#24104,.T.);
#33821=ORIENTED_EDGE('',*,*,#25502,.F.);
#33822=ORIENTED_EDGE('',*,*,#25221,.F.);
#33823=ORIENTED_EDGE('',*,*,#25504,.T.);
#33824=ORIENTED_EDGE('',*,*,#24105,.T.);
#33825=ORIENTED_EDGE('',*,*,#25503,.F.);
#33826=ORIENTED_EDGE('',*,*,#25220,.F.);
#33827=ORIENTED_EDGE('',*,*,#25500,.T.);
#33828=ORIENTED_EDGE('',*,*,#24106,.T.);
#33829=ORIENTED_EDGE('',*,*,#25504,.F.);
#33830=ORIENTED_EDGE('',*,*,#25219,.F.);
#33831=ORIENTED_EDGE('',*,*,#25505,.T.);
#33832=ORIENTED_EDGE('',*,*,#24095,.T.);
#33833=ORIENTED_EDGE('',*,*,#25506,.F.);
#33834=ORIENTED_EDGE('',*,*,#25212,.F.);
#33835=ORIENTED_EDGE('',*,*,#25507,.T.);
#33836=ORIENTED_EDGE('',*,*,#24096,.T.);
#33837=ORIENTED_EDGE('',*,*,#25505,.F.);
#33838=ORIENTED_EDGE('',*,*,#25211,.F.);
#33839=ORIENTED_EDGE('',*,*,#25508,.T.);
#33840=ORIENTED_EDGE('',*,*,#24097,.T.);
#33841=ORIENTED_EDGE('',*,*,#25507,.F.);
#33842=ORIENTED_EDGE('',*,*,#25216,.F.);
#33843=ORIENTED_EDGE('',*,*,#25509,.T.);
#33844=ORIENTED_EDGE('',*,*,#24098,.T.);
#33845=ORIENTED_EDGE('',*,*,#25508,.F.);
#33846=ORIENTED_EDGE('',*,*,#25215,.F.);
#33847=ORIENTED_EDGE('',*,*,#25510,.T.);
#33848=ORIENTED_EDGE('',*,*,#24099,.T.);
#33849=ORIENTED_EDGE('',*,*,#25509,.F.);
#33850=ORIENTED_EDGE('',*,*,#25214,.F.);
#33851=ORIENTED_EDGE('',*,*,#25506,.T.);
#33852=ORIENTED_EDGE('',*,*,#24100,.T.);
#33853=ORIENTED_EDGE('',*,*,#25510,.F.);
#33854=ORIENTED_EDGE('',*,*,#25213,.F.);
#33855=ORIENTED_EDGE('',*,*,#25511,.T.);
#33856=ORIENTED_EDGE('',*,*,#24089,.T.);
#33857=ORIENTED_EDGE('',*,*,#25512,.F.);
#33858=ORIENTED_EDGE('',*,*,#25206,.F.);
#33859=ORIENTED_EDGE('',*,*,#25513,.T.);
#33860=ORIENTED_EDGE('',*,*,#24090,.T.);
#33861=ORIENTED_EDGE('',*,*,#25511,.F.);
#33862=ORIENTED_EDGE('',*,*,#25205,.F.);
#33863=ORIENTED_EDGE('',*,*,#25514,.T.);
#33864=ORIENTED_EDGE('',*,*,#24091,.T.);
#33865=ORIENTED_EDGE('',*,*,#25513,.F.);
#33866=ORIENTED_EDGE('',*,*,#25210,.F.);
#33867=ORIENTED_EDGE('',*,*,#25515,.T.);
#33868=ORIENTED_EDGE('',*,*,#24092,.T.);
#33869=ORIENTED_EDGE('',*,*,#25514,.F.);
#33870=ORIENTED_EDGE('',*,*,#25209,.F.);
#33871=ORIENTED_EDGE('',*,*,#25516,.T.);
#33872=ORIENTED_EDGE('',*,*,#24093,.T.);
#33873=ORIENTED_EDGE('',*,*,#25515,.F.);
#33874=ORIENTED_EDGE('',*,*,#25208,.F.);
#33875=ORIENTED_EDGE('',*,*,#25512,.T.);
#33876=ORIENTED_EDGE('',*,*,#24094,.T.);
#33877=ORIENTED_EDGE('',*,*,#25516,.F.);
#33878=ORIENTED_EDGE('',*,*,#25207,.F.);
#33879=ORIENTED_EDGE('',*,*,#25517,.T.);
#33880=ORIENTED_EDGE('',*,*,#24083,.T.);
#33881=ORIENTED_EDGE('',*,*,#25518,.F.);
#33882=ORIENTED_EDGE('',*,*,#25200,.F.);
#33883=ORIENTED_EDGE('',*,*,#25519,.T.);
#33884=ORIENTED_EDGE('',*,*,#24084,.T.);
#33885=ORIENTED_EDGE('',*,*,#25517,.F.);
#33886=ORIENTED_EDGE('',*,*,#25199,.F.);
#33887=ORIENTED_EDGE('',*,*,#25520,.T.);
#33888=ORIENTED_EDGE('',*,*,#24085,.T.);
#33889=ORIENTED_EDGE('',*,*,#25519,.F.);
#33890=ORIENTED_EDGE('',*,*,#25204,.F.);
#33891=ORIENTED_EDGE('',*,*,#25521,.T.);
#33892=ORIENTED_EDGE('',*,*,#24086,.T.);
#33893=ORIENTED_EDGE('',*,*,#25520,.F.);
#33894=ORIENTED_EDGE('',*,*,#25203,.F.);
#33895=ORIENTED_EDGE('',*,*,#25522,.T.);
#33896=ORIENTED_EDGE('',*,*,#24087,.T.);
#33897=ORIENTED_EDGE('',*,*,#25521,.F.);
#33898=ORIENTED_EDGE('',*,*,#25202,.F.);
#33899=ORIENTED_EDGE('',*,*,#25518,.T.);
#33900=ORIENTED_EDGE('',*,*,#24088,.T.);
#33901=ORIENTED_EDGE('',*,*,#25522,.F.);
#33902=ORIENTED_EDGE('',*,*,#25201,.F.);
#33903=ORIENTED_EDGE('',*,*,#25523,.T.);
#33904=ORIENTED_EDGE('',*,*,#24077,.T.);
#33905=ORIENTED_EDGE('',*,*,#25524,.F.);
#33906=ORIENTED_EDGE('',*,*,#25194,.F.);
#33907=ORIENTED_EDGE('',*,*,#25525,.T.);
#33908=ORIENTED_EDGE('',*,*,#24078,.T.);
#33909=ORIENTED_EDGE('',*,*,#25523,.F.);
#33910=ORIENTED_EDGE('',*,*,#25193,.F.);
#33911=ORIENTED_EDGE('',*,*,#25526,.T.);
#33912=ORIENTED_EDGE('',*,*,#24079,.T.);
#33913=ORIENTED_EDGE('',*,*,#25525,.F.);
#33914=ORIENTED_EDGE('',*,*,#25198,.F.);
#33915=ORIENTED_EDGE('',*,*,#25527,.T.);
#33916=ORIENTED_EDGE('',*,*,#24080,.T.);
#33917=ORIENTED_EDGE('',*,*,#25526,.F.);
#33918=ORIENTED_EDGE('',*,*,#25197,.F.);
#33919=ORIENTED_EDGE('',*,*,#25528,.T.);
#33920=ORIENTED_EDGE('',*,*,#24081,.T.);
#33921=ORIENTED_EDGE('',*,*,#25527,.F.);
#33922=ORIENTED_EDGE('',*,*,#25196,.F.);
#33923=ORIENTED_EDGE('',*,*,#25524,.T.);
#33924=ORIENTED_EDGE('',*,*,#24082,.T.);
#33925=ORIENTED_EDGE('',*,*,#25528,.F.);
#33926=ORIENTED_EDGE('',*,*,#25195,.F.);
#33927=ORIENTED_EDGE('',*,*,#25529,.T.);
#33928=ORIENTED_EDGE('',*,*,#24071,.T.);
#33929=ORIENTED_EDGE('',*,*,#25530,.F.);
#33930=ORIENTED_EDGE('',*,*,#25188,.F.);
#33931=ORIENTED_EDGE('',*,*,#25531,.T.);
#33932=ORIENTED_EDGE('',*,*,#24072,.T.);
#33933=ORIENTED_EDGE('',*,*,#25529,.F.);
#33934=ORIENTED_EDGE('',*,*,#25187,.F.);
#33935=ORIENTED_EDGE('',*,*,#25532,.T.);
#33936=ORIENTED_EDGE('',*,*,#24073,.T.);
#33937=ORIENTED_EDGE('',*,*,#25531,.F.);
#33938=ORIENTED_EDGE('',*,*,#25192,.F.);
#33939=ORIENTED_EDGE('',*,*,#25533,.T.);
#33940=ORIENTED_EDGE('',*,*,#24074,.T.);
#33941=ORIENTED_EDGE('',*,*,#25532,.F.);
#33942=ORIENTED_EDGE('',*,*,#25191,.F.);
#33943=ORIENTED_EDGE('',*,*,#25534,.T.);
#33944=ORIENTED_EDGE('',*,*,#24075,.T.);
#33945=ORIENTED_EDGE('',*,*,#25533,.F.);
#33946=ORIENTED_EDGE('',*,*,#25190,.F.);
#33947=ORIENTED_EDGE('',*,*,#25530,.T.);
#33948=ORIENTED_EDGE('',*,*,#24076,.T.);
#33949=ORIENTED_EDGE('',*,*,#25534,.F.);
#33950=ORIENTED_EDGE('',*,*,#25189,.F.);
#33951=ORIENTED_EDGE('',*,*,#25535,.T.);
#33952=ORIENTED_EDGE('',*,*,#24065,.T.);
#33953=ORIENTED_EDGE('',*,*,#25536,.F.);
#33954=ORIENTED_EDGE('',*,*,#25182,.F.);
#33955=ORIENTED_EDGE('',*,*,#25537,.T.);
#33956=ORIENTED_EDGE('',*,*,#24066,.T.);
#33957=ORIENTED_EDGE('',*,*,#25535,.F.);
#33958=ORIENTED_EDGE('',*,*,#25181,.F.);
#33959=ORIENTED_EDGE('',*,*,#25538,.T.);
#33960=ORIENTED_EDGE('',*,*,#24067,.T.);
#33961=ORIENTED_EDGE('',*,*,#25537,.F.);
#33962=ORIENTED_EDGE('',*,*,#25186,.F.);
#33963=ORIENTED_EDGE('',*,*,#25539,.T.);
#33964=ORIENTED_EDGE('',*,*,#24068,.T.);
#33965=ORIENTED_EDGE('',*,*,#25538,.F.);
#33966=ORIENTED_EDGE('',*,*,#25185,.F.);
#33967=ORIENTED_EDGE('',*,*,#25540,.T.);
#33968=ORIENTED_EDGE('',*,*,#24069,.T.);
#33969=ORIENTED_EDGE('',*,*,#25539,.F.);
#33970=ORIENTED_EDGE('',*,*,#25184,.F.);
#33971=ORIENTED_EDGE('',*,*,#25536,.T.);
#33972=ORIENTED_EDGE('',*,*,#24070,.T.);
#33973=ORIENTED_EDGE('',*,*,#25540,.F.);
#33974=ORIENTED_EDGE('',*,*,#25183,.F.);
#33975=ORIENTED_EDGE('',*,*,#25541,.T.);
#33976=ORIENTED_EDGE('',*,*,#24059,.T.);
#33977=ORIENTED_EDGE('',*,*,#25542,.F.);
#33978=ORIENTED_EDGE('',*,*,#25176,.F.);
#33979=ORIENTED_EDGE('',*,*,#25543,.T.);
#33980=ORIENTED_EDGE('',*,*,#24060,.T.);
#33981=ORIENTED_EDGE('',*,*,#25541,.F.);
#33982=ORIENTED_EDGE('',*,*,#25175,.F.);
#33983=ORIENTED_EDGE('',*,*,#25544,.T.);
#33984=ORIENTED_EDGE('',*,*,#24061,.T.);
#33985=ORIENTED_EDGE('',*,*,#25543,.F.);
#33986=ORIENTED_EDGE('',*,*,#25180,.F.);
#33987=ORIENTED_EDGE('',*,*,#25545,.T.);
#33988=ORIENTED_EDGE('',*,*,#24062,.T.);
#33989=ORIENTED_EDGE('',*,*,#25544,.F.);
#33990=ORIENTED_EDGE('',*,*,#25179,.F.);
#33991=ORIENTED_EDGE('',*,*,#25546,.T.);
#33992=ORIENTED_EDGE('',*,*,#24063,.T.);
#33993=ORIENTED_EDGE('',*,*,#25545,.F.);
#33994=ORIENTED_EDGE('',*,*,#25178,.F.);
#33995=ORIENTED_EDGE('',*,*,#25542,.T.);
#33996=ORIENTED_EDGE('',*,*,#24064,.T.);
#33997=ORIENTED_EDGE('',*,*,#25546,.F.);
#33998=ORIENTED_EDGE('',*,*,#25177,.F.);
#33999=ORIENTED_EDGE('',*,*,#25547,.T.);
#34000=ORIENTED_EDGE('',*,*,#24053,.T.);
#34001=ORIENTED_EDGE('',*,*,#25548,.F.);
#34002=ORIENTED_EDGE('',*,*,#25170,.F.);
#34003=ORIENTED_EDGE('',*,*,#25549,.T.);
#34004=ORIENTED_EDGE('',*,*,#24054,.T.);
#34005=ORIENTED_EDGE('',*,*,#25547,.F.);
#34006=ORIENTED_EDGE('',*,*,#25169,.F.);
#34007=ORIENTED_EDGE('',*,*,#25550,.T.);
#34008=ORIENTED_EDGE('',*,*,#24055,.T.);
#34009=ORIENTED_EDGE('',*,*,#25549,.F.);
#34010=ORIENTED_EDGE('',*,*,#25174,.F.);
#34011=ORIENTED_EDGE('',*,*,#25551,.T.);
#34012=ORIENTED_EDGE('',*,*,#24056,.T.);
#34013=ORIENTED_EDGE('',*,*,#25550,.F.);
#34014=ORIENTED_EDGE('',*,*,#25173,.F.);
#34015=ORIENTED_EDGE('',*,*,#25552,.T.);
#34016=ORIENTED_EDGE('',*,*,#24057,.T.);
#34017=ORIENTED_EDGE('',*,*,#25551,.F.);
#34018=ORIENTED_EDGE('',*,*,#25172,.F.);
#34019=ORIENTED_EDGE('',*,*,#25548,.T.);
#34020=ORIENTED_EDGE('',*,*,#24058,.T.);
#34021=ORIENTED_EDGE('',*,*,#25552,.F.);
#34022=ORIENTED_EDGE('',*,*,#25171,.F.);
#34023=ORIENTED_EDGE('',*,*,#25553,.T.);
#34024=ORIENTED_EDGE('',*,*,#24047,.T.);
#34025=ORIENTED_EDGE('',*,*,#25554,.F.);
#34026=ORIENTED_EDGE('',*,*,#25164,.F.);
#34027=ORIENTED_EDGE('',*,*,#25555,.T.);
#34028=ORIENTED_EDGE('',*,*,#24048,.T.);
#34029=ORIENTED_EDGE('',*,*,#25553,.F.);
#34030=ORIENTED_EDGE('',*,*,#25163,.F.);
#34031=ORIENTED_EDGE('',*,*,#25556,.T.);
#34032=ORIENTED_EDGE('',*,*,#24049,.T.);
#34033=ORIENTED_EDGE('',*,*,#25555,.F.);
#34034=ORIENTED_EDGE('',*,*,#25168,.F.);
#34035=ORIENTED_EDGE('',*,*,#25557,.T.);
#34036=ORIENTED_EDGE('',*,*,#24050,.T.);
#34037=ORIENTED_EDGE('',*,*,#25556,.F.);
#34038=ORIENTED_EDGE('',*,*,#25167,.F.);
#34039=ORIENTED_EDGE('',*,*,#25558,.T.);
#34040=ORIENTED_EDGE('',*,*,#24051,.T.);
#34041=ORIENTED_EDGE('',*,*,#25557,.F.);
#34042=ORIENTED_EDGE('',*,*,#25166,.F.);
#34043=ORIENTED_EDGE('',*,*,#25554,.T.);
#34044=ORIENTED_EDGE('',*,*,#24052,.T.);
#34045=ORIENTED_EDGE('',*,*,#25558,.F.);
#34046=ORIENTED_EDGE('',*,*,#25165,.F.);
#34047=ORIENTED_EDGE('',*,*,#25559,.T.);
#34048=ORIENTED_EDGE('',*,*,#24041,.T.);
#34049=ORIENTED_EDGE('',*,*,#25560,.F.);
#34050=ORIENTED_EDGE('',*,*,#25158,.F.);
#34051=ORIENTED_EDGE('',*,*,#25561,.T.);
#34052=ORIENTED_EDGE('',*,*,#24042,.T.);
#34053=ORIENTED_EDGE('',*,*,#25559,.F.);
#34054=ORIENTED_EDGE('',*,*,#25157,.F.);
#34055=ORIENTED_EDGE('',*,*,#25562,.T.);
#34056=ORIENTED_EDGE('',*,*,#24043,.T.);
#34057=ORIENTED_EDGE('',*,*,#25561,.F.);
#34058=ORIENTED_EDGE('',*,*,#25162,.F.);
#34059=ORIENTED_EDGE('',*,*,#25563,.T.);
#34060=ORIENTED_EDGE('',*,*,#24044,.T.);
#34061=ORIENTED_EDGE('',*,*,#25562,.F.);
#34062=ORIENTED_EDGE('',*,*,#25161,.F.);
#34063=ORIENTED_EDGE('',*,*,#25564,.T.);
#34064=ORIENTED_EDGE('',*,*,#24045,.T.);
#34065=ORIENTED_EDGE('',*,*,#25563,.F.);
#34066=ORIENTED_EDGE('',*,*,#25160,.F.);
#34067=ORIENTED_EDGE('',*,*,#25560,.T.);
#34068=ORIENTED_EDGE('',*,*,#24046,.T.);
#34069=ORIENTED_EDGE('',*,*,#25564,.F.);
#34070=ORIENTED_EDGE('',*,*,#25159,.F.);
#34071=ORIENTED_EDGE('',*,*,#25565,.T.);
#34072=ORIENTED_EDGE('',*,*,#24035,.T.);
#34073=ORIENTED_EDGE('',*,*,#25566,.F.);
#34074=ORIENTED_EDGE('',*,*,#25152,.F.);
#34075=ORIENTED_EDGE('',*,*,#25567,.T.);
#34076=ORIENTED_EDGE('',*,*,#24036,.T.);
#34077=ORIENTED_EDGE('',*,*,#25565,.F.);
#34078=ORIENTED_EDGE('',*,*,#25151,.F.);
#34079=ORIENTED_EDGE('',*,*,#25568,.T.);
#34080=ORIENTED_EDGE('',*,*,#24037,.T.);
#34081=ORIENTED_EDGE('',*,*,#25567,.F.);
#34082=ORIENTED_EDGE('',*,*,#25156,.F.);
#34083=ORIENTED_EDGE('',*,*,#25569,.T.);
#34084=ORIENTED_EDGE('',*,*,#24038,.T.);
#34085=ORIENTED_EDGE('',*,*,#25568,.F.);
#34086=ORIENTED_EDGE('',*,*,#25155,.F.);
#34087=ORIENTED_EDGE('',*,*,#25570,.T.);
#34088=ORIENTED_EDGE('',*,*,#24039,.T.);
#34089=ORIENTED_EDGE('',*,*,#25569,.F.);
#34090=ORIENTED_EDGE('',*,*,#25154,.F.);
#34091=ORIENTED_EDGE('',*,*,#25566,.T.);
#34092=ORIENTED_EDGE('',*,*,#24040,.T.);
#34093=ORIENTED_EDGE('',*,*,#25570,.F.);
#34094=ORIENTED_EDGE('',*,*,#25153,.F.);
#34095=ORIENTED_EDGE('',*,*,#25571,.T.);
#34096=ORIENTED_EDGE('',*,*,#24029,.T.);
#34097=ORIENTED_EDGE('',*,*,#25572,.F.);
#34098=ORIENTED_EDGE('',*,*,#25146,.F.);
#34099=ORIENTED_EDGE('',*,*,#25573,.T.);
#34100=ORIENTED_EDGE('',*,*,#24030,.T.);
#34101=ORIENTED_EDGE('',*,*,#25571,.F.);
#34102=ORIENTED_EDGE('',*,*,#25145,.F.);
#34103=ORIENTED_EDGE('',*,*,#25574,.T.);
#34104=ORIENTED_EDGE('',*,*,#24031,.T.);
#34105=ORIENTED_EDGE('',*,*,#25573,.F.);
#34106=ORIENTED_EDGE('',*,*,#25150,.F.);
#34107=ORIENTED_EDGE('',*,*,#25575,.T.);
#34108=ORIENTED_EDGE('',*,*,#24032,.T.);
#34109=ORIENTED_EDGE('',*,*,#25574,.F.);
#34110=ORIENTED_EDGE('',*,*,#25149,.F.);
#34111=ORIENTED_EDGE('',*,*,#25576,.T.);
#34112=ORIENTED_EDGE('',*,*,#24033,.T.);
#34113=ORIENTED_EDGE('',*,*,#25575,.F.);
#34114=ORIENTED_EDGE('',*,*,#25148,.F.);
#34115=ORIENTED_EDGE('',*,*,#25572,.T.);
#34116=ORIENTED_EDGE('',*,*,#24034,.T.);
#34117=ORIENTED_EDGE('',*,*,#25576,.F.);
#34118=ORIENTED_EDGE('',*,*,#25147,.F.);
#34119=ORIENTED_EDGE('',*,*,#25577,.T.);
#34120=ORIENTED_EDGE('',*,*,#24023,.T.);
#34121=ORIENTED_EDGE('',*,*,#25578,.F.);
#34122=ORIENTED_EDGE('',*,*,#25140,.F.);
#34123=ORIENTED_EDGE('',*,*,#25579,.T.);
#34124=ORIENTED_EDGE('',*,*,#24024,.T.);
#34125=ORIENTED_EDGE('',*,*,#25577,.F.);
#34126=ORIENTED_EDGE('',*,*,#25139,.F.);
#34127=ORIENTED_EDGE('',*,*,#25580,.T.);
#34128=ORIENTED_EDGE('',*,*,#24025,.T.);
#34129=ORIENTED_EDGE('',*,*,#25579,.F.);
#34130=ORIENTED_EDGE('',*,*,#25144,.F.);
#34131=ORIENTED_EDGE('',*,*,#25581,.T.);
#34132=ORIENTED_EDGE('',*,*,#24026,.T.);
#34133=ORIENTED_EDGE('',*,*,#25580,.F.);
#34134=ORIENTED_EDGE('',*,*,#25143,.F.);
#34135=ORIENTED_EDGE('',*,*,#25582,.T.);
#34136=ORIENTED_EDGE('',*,*,#24027,.T.);
#34137=ORIENTED_EDGE('',*,*,#25581,.F.);
#34138=ORIENTED_EDGE('',*,*,#25142,.F.);
#34139=ORIENTED_EDGE('',*,*,#25578,.T.);
#34140=ORIENTED_EDGE('',*,*,#24028,.T.);
#34141=ORIENTED_EDGE('',*,*,#25582,.F.);
#34142=ORIENTED_EDGE('',*,*,#25141,.F.);
#34143=ORIENTED_EDGE('',*,*,#25583,.T.);
#34144=ORIENTED_EDGE('',*,*,#24017,.T.);
#34145=ORIENTED_EDGE('',*,*,#25584,.F.);
#34146=ORIENTED_EDGE('',*,*,#25134,.F.);
#34147=ORIENTED_EDGE('',*,*,#25585,.T.);
#34148=ORIENTED_EDGE('',*,*,#24018,.T.);
#34149=ORIENTED_EDGE('',*,*,#25583,.F.);
#34150=ORIENTED_EDGE('',*,*,#25133,.F.);
#34151=ORIENTED_EDGE('',*,*,#25586,.T.);
#34152=ORIENTED_EDGE('',*,*,#24019,.T.);
#34153=ORIENTED_EDGE('',*,*,#25585,.F.);
#34154=ORIENTED_EDGE('',*,*,#25138,.F.);
#34155=ORIENTED_EDGE('',*,*,#25587,.T.);
#34156=ORIENTED_EDGE('',*,*,#24020,.T.);
#34157=ORIENTED_EDGE('',*,*,#25586,.F.);
#34158=ORIENTED_EDGE('',*,*,#25137,.F.);
#34159=ORIENTED_EDGE('',*,*,#25588,.T.);
#34160=ORIENTED_EDGE('',*,*,#24021,.T.);
#34161=ORIENTED_EDGE('',*,*,#25587,.F.);
#34162=ORIENTED_EDGE('',*,*,#25136,.F.);
#34163=ORIENTED_EDGE('',*,*,#25584,.T.);
#34164=ORIENTED_EDGE('',*,*,#24022,.T.);
#34165=ORIENTED_EDGE('',*,*,#25588,.F.);
#34166=ORIENTED_EDGE('',*,*,#25135,.F.);
#34167=ORIENTED_EDGE('',*,*,#25589,.T.);
#34168=ORIENTED_EDGE('',*,*,#24011,.T.);
#34169=ORIENTED_EDGE('',*,*,#25590,.F.);
#34170=ORIENTED_EDGE('',*,*,#25128,.F.);
#34171=ORIENTED_EDGE('',*,*,#25591,.T.);
#34172=ORIENTED_EDGE('',*,*,#24012,.T.);
#34173=ORIENTED_EDGE('',*,*,#25589,.F.);
#34174=ORIENTED_EDGE('',*,*,#25127,.F.);
#34175=ORIENTED_EDGE('',*,*,#25592,.T.);
#34176=ORIENTED_EDGE('',*,*,#24013,.T.);
#34177=ORIENTED_EDGE('',*,*,#25591,.F.);
#34178=ORIENTED_EDGE('',*,*,#25132,.F.);
#34179=ORIENTED_EDGE('',*,*,#25593,.T.);
#34180=ORIENTED_EDGE('',*,*,#24014,.T.);
#34181=ORIENTED_EDGE('',*,*,#25592,.F.);
#34182=ORIENTED_EDGE('',*,*,#25131,.F.);
#34183=ORIENTED_EDGE('',*,*,#25594,.T.);
#34184=ORIENTED_EDGE('',*,*,#24015,.T.);
#34185=ORIENTED_EDGE('',*,*,#25593,.F.);
#34186=ORIENTED_EDGE('',*,*,#25130,.F.);
#34187=ORIENTED_EDGE('',*,*,#25590,.T.);
#34188=ORIENTED_EDGE('',*,*,#24016,.T.);
#34189=ORIENTED_EDGE('',*,*,#25594,.F.);
#34190=ORIENTED_EDGE('',*,*,#25129,.F.);
#34191=ORIENTED_EDGE('',*,*,#25595,.T.);
#34192=ORIENTED_EDGE('',*,*,#24005,.T.);
#34193=ORIENTED_EDGE('',*,*,#25596,.F.);
#34194=ORIENTED_EDGE('',*,*,#25122,.F.);
#34195=ORIENTED_EDGE('',*,*,#25597,.T.);
#34196=ORIENTED_EDGE('',*,*,#24006,.T.);
#34197=ORIENTED_EDGE('',*,*,#25595,.F.);
#34198=ORIENTED_EDGE('',*,*,#25121,.F.);
#34199=ORIENTED_EDGE('',*,*,#25598,.T.);
#34200=ORIENTED_EDGE('',*,*,#24007,.T.);
#34201=ORIENTED_EDGE('',*,*,#25597,.F.);
#34202=ORIENTED_EDGE('',*,*,#25126,.F.);
#34203=ORIENTED_EDGE('',*,*,#25599,.T.);
#34204=ORIENTED_EDGE('',*,*,#24008,.T.);
#34205=ORIENTED_EDGE('',*,*,#25598,.F.);
#34206=ORIENTED_EDGE('',*,*,#25125,.F.);
#34207=ORIENTED_EDGE('',*,*,#25600,.T.);
#34208=ORIENTED_EDGE('',*,*,#24009,.T.);
#34209=ORIENTED_EDGE('',*,*,#25599,.F.);
#34210=ORIENTED_EDGE('',*,*,#25124,.F.);
#34211=ORIENTED_EDGE('',*,*,#25596,.T.);
#34212=ORIENTED_EDGE('',*,*,#24010,.T.);
#34213=ORIENTED_EDGE('',*,*,#25600,.F.);
#34214=ORIENTED_EDGE('',*,*,#25123,.F.);
#34215=ORIENTED_EDGE('',*,*,#25601,.T.);
#34216=ORIENTED_EDGE('',*,*,#23999,.T.);
#34217=ORIENTED_EDGE('',*,*,#25602,.F.);
#34218=ORIENTED_EDGE('',*,*,#25116,.F.);
#34219=ORIENTED_EDGE('',*,*,#25603,.T.);
#34220=ORIENTED_EDGE('',*,*,#24000,.T.);
#34221=ORIENTED_EDGE('',*,*,#25601,.F.);
#34222=ORIENTED_EDGE('',*,*,#25115,.F.);
#34223=ORIENTED_EDGE('',*,*,#25604,.T.);
#34224=ORIENTED_EDGE('',*,*,#24001,.T.);
#34225=ORIENTED_EDGE('',*,*,#25603,.F.);
#34226=ORIENTED_EDGE('',*,*,#25120,.F.);
#34227=ORIENTED_EDGE('',*,*,#25605,.T.);
#34228=ORIENTED_EDGE('',*,*,#24002,.T.);
#34229=ORIENTED_EDGE('',*,*,#25604,.F.);
#34230=ORIENTED_EDGE('',*,*,#25119,.F.);
#34231=ORIENTED_EDGE('',*,*,#25606,.T.);
#34232=ORIENTED_EDGE('',*,*,#24003,.T.);
#34233=ORIENTED_EDGE('',*,*,#25605,.F.);
#34234=ORIENTED_EDGE('',*,*,#25118,.F.);
#34235=ORIENTED_EDGE('',*,*,#25602,.T.);
#34236=ORIENTED_EDGE('',*,*,#24004,.T.);
#34237=ORIENTED_EDGE('',*,*,#25606,.F.);
#34238=ORIENTED_EDGE('',*,*,#25117,.F.);
#34239=ORIENTED_EDGE('',*,*,#25607,.T.);
#34240=ORIENTED_EDGE('',*,*,#23993,.T.);
#34241=ORIENTED_EDGE('',*,*,#25608,.F.);
#34242=ORIENTED_EDGE('',*,*,#25110,.F.);
#34243=ORIENTED_EDGE('',*,*,#25609,.T.);
#34244=ORIENTED_EDGE('',*,*,#23994,.T.);
#34245=ORIENTED_EDGE('',*,*,#25607,.F.);
#34246=ORIENTED_EDGE('',*,*,#25109,.F.);
#34247=ORIENTED_EDGE('',*,*,#25610,.T.);
#34248=ORIENTED_EDGE('',*,*,#23995,.T.);
#34249=ORIENTED_EDGE('',*,*,#25609,.F.);
#34250=ORIENTED_EDGE('',*,*,#25114,.F.);
#34251=ORIENTED_EDGE('',*,*,#25611,.T.);
#34252=ORIENTED_EDGE('',*,*,#23996,.T.);
#34253=ORIENTED_EDGE('',*,*,#25610,.F.);
#34254=ORIENTED_EDGE('',*,*,#25113,.F.);
#34255=ORIENTED_EDGE('',*,*,#25612,.T.);
#34256=ORIENTED_EDGE('',*,*,#23997,.T.);
#34257=ORIENTED_EDGE('',*,*,#25611,.F.);
#34258=ORIENTED_EDGE('',*,*,#25112,.F.);
#34259=ORIENTED_EDGE('',*,*,#25608,.T.);
#34260=ORIENTED_EDGE('',*,*,#23998,.T.);
#34261=ORIENTED_EDGE('',*,*,#25612,.F.);
#34262=ORIENTED_EDGE('',*,*,#25111,.F.);
#34263=ORIENTED_EDGE('',*,*,#25613,.T.);
#34264=ORIENTED_EDGE('',*,*,#23987,.T.);
#34265=ORIENTED_EDGE('',*,*,#25614,.F.);
#34266=ORIENTED_EDGE('',*,*,#25104,.F.);
#34267=ORIENTED_EDGE('',*,*,#25615,.T.);
#34268=ORIENTED_EDGE('',*,*,#23988,.T.);
#34269=ORIENTED_EDGE('',*,*,#25613,.F.);
#34270=ORIENTED_EDGE('',*,*,#25103,.F.);
#34271=ORIENTED_EDGE('',*,*,#25616,.T.);
#34272=ORIENTED_EDGE('',*,*,#23989,.T.);
#34273=ORIENTED_EDGE('',*,*,#25615,.F.);
#34274=ORIENTED_EDGE('',*,*,#25108,.F.);
#34275=ORIENTED_EDGE('',*,*,#25617,.T.);
#34276=ORIENTED_EDGE('',*,*,#23990,.T.);
#34277=ORIENTED_EDGE('',*,*,#25616,.F.);
#34278=ORIENTED_EDGE('',*,*,#25107,.F.);
#34279=ORIENTED_EDGE('',*,*,#25618,.T.);
#34280=ORIENTED_EDGE('',*,*,#23991,.T.);
#34281=ORIENTED_EDGE('',*,*,#25617,.F.);
#34282=ORIENTED_EDGE('',*,*,#25106,.F.);
#34283=ORIENTED_EDGE('',*,*,#25614,.T.);
#34284=ORIENTED_EDGE('',*,*,#23992,.T.);
#34285=ORIENTED_EDGE('',*,*,#25618,.F.);
#34286=ORIENTED_EDGE('',*,*,#25105,.F.);
#34287=ORIENTED_EDGE('',*,*,#25619,.T.);
#34288=ORIENTED_EDGE('',*,*,#23981,.T.);
#34289=ORIENTED_EDGE('',*,*,#25620,.F.);
#34290=ORIENTED_EDGE('',*,*,#25098,.F.);
#34291=ORIENTED_EDGE('',*,*,#25621,.T.);
#34292=ORIENTED_EDGE('',*,*,#23982,.T.);
#34293=ORIENTED_EDGE('',*,*,#25619,.F.);
#34294=ORIENTED_EDGE('',*,*,#25097,.F.);
#34295=ORIENTED_EDGE('',*,*,#25622,.T.);
#34296=ORIENTED_EDGE('',*,*,#23983,.T.);
#34297=ORIENTED_EDGE('',*,*,#25621,.F.);
#34298=ORIENTED_EDGE('',*,*,#25102,.F.);
#34299=ORIENTED_EDGE('',*,*,#25623,.T.);
#34300=ORIENTED_EDGE('',*,*,#23984,.T.);
#34301=ORIENTED_EDGE('',*,*,#25622,.F.);
#34302=ORIENTED_EDGE('',*,*,#25101,.F.);
#34303=ORIENTED_EDGE('',*,*,#25624,.T.);
#34304=ORIENTED_EDGE('',*,*,#23985,.T.);
#34305=ORIENTED_EDGE('',*,*,#25623,.F.);
#34306=ORIENTED_EDGE('',*,*,#25100,.F.);
#34307=ORIENTED_EDGE('',*,*,#25620,.T.);
#34308=ORIENTED_EDGE('',*,*,#23986,.T.);
#34309=ORIENTED_EDGE('',*,*,#25624,.F.);
#34310=ORIENTED_EDGE('',*,*,#25099,.F.);
#34311=ORIENTED_EDGE('',*,*,#25625,.T.);
#34312=ORIENTED_EDGE('',*,*,#23975,.T.);
#34313=ORIENTED_EDGE('',*,*,#25626,.F.);
#34314=ORIENTED_EDGE('',*,*,#25092,.F.);
#34315=ORIENTED_EDGE('',*,*,#25627,.T.);
#34316=ORIENTED_EDGE('',*,*,#23976,.T.);
#34317=ORIENTED_EDGE('',*,*,#25625,.F.);
#34318=ORIENTED_EDGE('',*,*,#25091,.F.);
#34319=ORIENTED_EDGE('',*,*,#25628,.T.);
#34320=ORIENTED_EDGE('',*,*,#23977,.T.);
#34321=ORIENTED_EDGE('',*,*,#25627,.F.);
#34322=ORIENTED_EDGE('',*,*,#25096,.F.);
#34323=ORIENTED_EDGE('',*,*,#25629,.T.);
#34324=ORIENTED_EDGE('',*,*,#23978,.T.);
#34325=ORIENTED_EDGE('',*,*,#25628,.F.);
#34326=ORIENTED_EDGE('',*,*,#25095,.F.);
#34327=ORIENTED_EDGE('',*,*,#25630,.T.);
#34328=ORIENTED_EDGE('',*,*,#23979,.T.);
#34329=ORIENTED_EDGE('',*,*,#25629,.F.);
#34330=ORIENTED_EDGE('',*,*,#25094,.F.);
#34331=ORIENTED_EDGE('',*,*,#25626,.T.);
#34332=ORIENTED_EDGE('',*,*,#23980,.T.);
#34333=ORIENTED_EDGE('',*,*,#25630,.F.);
#34334=ORIENTED_EDGE('',*,*,#25093,.F.);
#34335=ORIENTED_EDGE('',*,*,#25631,.T.);
#34336=ORIENTED_EDGE('',*,*,#23969,.T.);
#34337=ORIENTED_EDGE('',*,*,#25632,.F.);
#34338=ORIENTED_EDGE('',*,*,#25086,.F.);
#34339=ORIENTED_EDGE('',*,*,#25633,.T.);
#34340=ORIENTED_EDGE('',*,*,#23970,.T.);
#34341=ORIENTED_EDGE('',*,*,#25631,.F.);
#34342=ORIENTED_EDGE('',*,*,#25085,.F.);
#34343=ORIENTED_EDGE('',*,*,#25634,.T.);
#34344=ORIENTED_EDGE('',*,*,#23971,.T.);
#34345=ORIENTED_EDGE('',*,*,#25633,.F.);
#34346=ORIENTED_EDGE('',*,*,#25090,.F.);
#34347=ORIENTED_EDGE('',*,*,#25635,.T.);
#34348=ORIENTED_EDGE('',*,*,#23972,.T.);
#34349=ORIENTED_EDGE('',*,*,#25634,.F.);
#34350=ORIENTED_EDGE('',*,*,#25089,.F.);
#34351=ORIENTED_EDGE('',*,*,#25636,.T.);
#34352=ORIENTED_EDGE('',*,*,#23973,.T.);
#34353=ORIENTED_EDGE('',*,*,#25635,.F.);
#34354=ORIENTED_EDGE('',*,*,#25088,.F.);
#34355=ORIENTED_EDGE('',*,*,#25632,.T.);
#34356=ORIENTED_EDGE('',*,*,#23974,.T.);
#34357=ORIENTED_EDGE('',*,*,#25636,.F.);
#34358=ORIENTED_EDGE('',*,*,#25087,.F.);
#34359=ORIENTED_EDGE('',*,*,#25637,.T.);
#34360=ORIENTED_EDGE('',*,*,#23963,.T.);
#34361=ORIENTED_EDGE('',*,*,#25638,.F.);
#34362=ORIENTED_EDGE('',*,*,#25080,.F.);
#34363=ORIENTED_EDGE('',*,*,#25639,.T.);
#34364=ORIENTED_EDGE('',*,*,#23964,.T.);
#34365=ORIENTED_EDGE('',*,*,#25637,.F.);
#34366=ORIENTED_EDGE('',*,*,#25079,.F.);
#34367=ORIENTED_EDGE('',*,*,#25640,.T.);
#34368=ORIENTED_EDGE('',*,*,#23965,.T.);
#34369=ORIENTED_EDGE('',*,*,#25639,.F.);
#34370=ORIENTED_EDGE('',*,*,#25084,.F.);
#34371=ORIENTED_EDGE('',*,*,#25641,.T.);
#34372=ORIENTED_EDGE('',*,*,#23966,.T.);
#34373=ORIENTED_EDGE('',*,*,#25640,.F.);
#34374=ORIENTED_EDGE('',*,*,#25083,.F.);
#34375=ORIENTED_EDGE('',*,*,#25642,.T.);
#34376=ORIENTED_EDGE('',*,*,#23967,.T.);
#34377=ORIENTED_EDGE('',*,*,#25641,.F.);
#34378=ORIENTED_EDGE('',*,*,#25082,.F.);
#34379=ORIENTED_EDGE('',*,*,#25638,.T.);
#34380=ORIENTED_EDGE('',*,*,#23968,.T.);
#34381=ORIENTED_EDGE('',*,*,#25642,.F.);
#34382=ORIENTED_EDGE('',*,*,#25081,.F.);
#34383=ORIENTED_EDGE('',*,*,#25643,.T.);
#34384=ORIENTED_EDGE('',*,*,#23957,.T.);
#34385=ORIENTED_EDGE('',*,*,#25644,.F.);
#34386=ORIENTED_EDGE('',*,*,#25074,.F.);
#34387=ORIENTED_EDGE('',*,*,#25645,.T.);
#34388=ORIENTED_EDGE('',*,*,#23958,.T.);
#34389=ORIENTED_EDGE('',*,*,#25643,.F.);
#34390=ORIENTED_EDGE('',*,*,#25073,.F.);
#34391=ORIENTED_EDGE('',*,*,#25646,.T.);
#34392=ORIENTED_EDGE('',*,*,#23959,.T.);
#34393=ORIENTED_EDGE('',*,*,#25645,.F.);
#34394=ORIENTED_EDGE('',*,*,#25078,.F.);
#34395=ORIENTED_EDGE('',*,*,#25647,.T.);
#34396=ORIENTED_EDGE('',*,*,#23960,.T.);
#34397=ORIENTED_EDGE('',*,*,#25646,.F.);
#34398=ORIENTED_EDGE('',*,*,#25077,.F.);
#34399=ORIENTED_EDGE('',*,*,#25648,.T.);
#34400=ORIENTED_EDGE('',*,*,#23961,.T.);
#34401=ORIENTED_EDGE('',*,*,#25647,.F.);
#34402=ORIENTED_EDGE('',*,*,#25076,.F.);
#34403=ORIENTED_EDGE('',*,*,#25644,.T.);
#34404=ORIENTED_EDGE('',*,*,#23962,.T.);
#34405=ORIENTED_EDGE('',*,*,#25648,.F.);
#34406=ORIENTED_EDGE('',*,*,#25075,.F.);
#34407=ORIENTED_EDGE('',*,*,#25649,.T.);
#34408=ORIENTED_EDGE('',*,*,#23951,.T.);
#34409=ORIENTED_EDGE('',*,*,#25650,.F.);
#34410=ORIENTED_EDGE('',*,*,#25068,.F.);
#34411=ORIENTED_EDGE('',*,*,#25651,.T.);
#34412=ORIENTED_EDGE('',*,*,#23952,.T.);
#34413=ORIENTED_EDGE('',*,*,#25649,.F.);
#34414=ORIENTED_EDGE('',*,*,#25067,.F.);
#34415=ORIENTED_EDGE('',*,*,#25652,.T.);
#34416=ORIENTED_EDGE('',*,*,#23953,.T.);
#34417=ORIENTED_EDGE('',*,*,#25651,.F.);
#34418=ORIENTED_EDGE('',*,*,#25072,.F.);
#34419=ORIENTED_EDGE('',*,*,#25653,.T.);
#34420=ORIENTED_EDGE('',*,*,#23954,.T.);
#34421=ORIENTED_EDGE('',*,*,#25652,.F.);
#34422=ORIENTED_EDGE('',*,*,#25071,.F.);
#34423=ORIENTED_EDGE('',*,*,#25654,.T.);
#34424=ORIENTED_EDGE('',*,*,#23955,.T.);
#34425=ORIENTED_EDGE('',*,*,#25653,.F.);
#34426=ORIENTED_EDGE('',*,*,#25070,.F.);
#34427=ORIENTED_EDGE('',*,*,#25650,.T.);
#34428=ORIENTED_EDGE('',*,*,#23956,.T.);
#34429=ORIENTED_EDGE('',*,*,#25654,.F.);
#34430=ORIENTED_EDGE('',*,*,#25069,.F.);
#34431=ORIENTED_EDGE('',*,*,#25655,.T.);
#34432=ORIENTED_EDGE('',*,*,#23945,.T.);
#34433=ORIENTED_EDGE('',*,*,#25656,.F.);
#34434=ORIENTED_EDGE('',*,*,#25062,.F.);
#34435=ORIENTED_EDGE('',*,*,#25657,.T.);
#34436=ORIENTED_EDGE('',*,*,#23946,.T.);
#34437=ORIENTED_EDGE('',*,*,#25655,.F.);
#34438=ORIENTED_EDGE('',*,*,#25061,.F.);
#34439=ORIENTED_EDGE('',*,*,#25658,.T.);
#34440=ORIENTED_EDGE('',*,*,#23947,.T.);
#34441=ORIENTED_EDGE('',*,*,#25657,.F.);
#34442=ORIENTED_EDGE('',*,*,#25066,.F.);
#34443=ORIENTED_EDGE('',*,*,#25659,.T.);
#34444=ORIENTED_EDGE('',*,*,#23948,.T.);
#34445=ORIENTED_EDGE('',*,*,#25658,.F.);
#34446=ORIENTED_EDGE('',*,*,#25065,.F.);
#34447=ORIENTED_EDGE('',*,*,#25660,.T.);
#34448=ORIENTED_EDGE('',*,*,#23949,.T.);
#34449=ORIENTED_EDGE('',*,*,#25659,.F.);
#34450=ORIENTED_EDGE('',*,*,#25064,.F.);
#34451=ORIENTED_EDGE('',*,*,#25656,.T.);
#34452=ORIENTED_EDGE('',*,*,#23950,.T.);
#34453=ORIENTED_EDGE('',*,*,#25660,.F.);
#34454=ORIENTED_EDGE('',*,*,#25063,.F.);
#34455=ORIENTED_EDGE('',*,*,#25661,.T.);
#34456=ORIENTED_EDGE('',*,*,#23939,.T.);
#34457=ORIENTED_EDGE('',*,*,#25662,.F.);
#34458=ORIENTED_EDGE('',*,*,#25056,.F.);
#34459=ORIENTED_EDGE('',*,*,#25663,.T.);
#34460=ORIENTED_EDGE('',*,*,#23940,.T.);
#34461=ORIENTED_EDGE('',*,*,#25661,.F.);
#34462=ORIENTED_EDGE('',*,*,#25055,.F.);
#34463=ORIENTED_EDGE('',*,*,#25664,.T.);
#34464=ORIENTED_EDGE('',*,*,#23941,.T.);
#34465=ORIENTED_EDGE('',*,*,#25663,.F.);
#34466=ORIENTED_EDGE('',*,*,#25060,.F.);
#34467=ORIENTED_EDGE('',*,*,#25665,.T.);
#34468=ORIENTED_EDGE('',*,*,#23942,.T.);
#34469=ORIENTED_EDGE('',*,*,#25664,.F.);
#34470=ORIENTED_EDGE('',*,*,#25059,.F.);
#34471=ORIENTED_EDGE('',*,*,#25666,.T.);
#34472=ORIENTED_EDGE('',*,*,#23943,.T.);
#34473=ORIENTED_EDGE('',*,*,#25665,.F.);
#34474=ORIENTED_EDGE('',*,*,#25058,.F.);
#34475=ORIENTED_EDGE('',*,*,#25662,.T.);
#34476=ORIENTED_EDGE('',*,*,#23944,.T.);
#34477=ORIENTED_EDGE('',*,*,#25666,.F.);
#34478=ORIENTED_EDGE('',*,*,#25057,.F.);
#34479=ORIENTED_EDGE('',*,*,#25667,.T.);
#34480=ORIENTED_EDGE('',*,*,#23933,.T.);
#34481=ORIENTED_EDGE('',*,*,#25668,.F.);
#34482=ORIENTED_EDGE('',*,*,#25050,.F.);
#34483=ORIENTED_EDGE('',*,*,#25669,.T.);
#34484=ORIENTED_EDGE('',*,*,#23934,.T.);
#34485=ORIENTED_EDGE('',*,*,#25667,.F.);
#34486=ORIENTED_EDGE('',*,*,#25049,.F.);
#34487=ORIENTED_EDGE('',*,*,#25670,.T.);
#34488=ORIENTED_EDGE('',*,*,#23935,.T.);
#34489=ORIENTED_EDGE('',*,*,#25669,.F.);
#34490=ORIENTED_EDGE('',*,*,#25054,.F.);
#34491=ORIENTED_EDGE('',*,*,#25671,.T.);
#34492=ORIENTED_EDGE('',*,*,#23936,.T.);
#34493=ORIENTED_EDGE('',*,*,#25670,.F.);
#34494=ORIENTED_EDGE('',*,*,#25053,.F.);
#34495=ORIENTED_EDGE('',*,*,#25672,.T.);
#34496=ORIENTED_EDGE('',*,*,#23937,.T.);
#34497=ORIENTED_EDGE('',*,*,#25671,.F.);
#34498=ORIENTED_EDGE('',*,*,#25052,.F.);
#34499=ORIENTED_EDGE('',*,*,#25668,.T.);
#34500=ORIENTED_EDGE('',*,*,#23938,.T.);
#34501=ORIENTED_EDGE('',*,*,#25672,.F.);
#34502=ORIENTED_EDGE('',*,*,#25051,.F.);
#34503=ORIENTED_EDGE('',*,*,#25673,.T.);
#34504=ORIENTED_EDGE('',*,*,#23927,.T.);
#34505=ORIENTED_EDGE('',*,*,#25674,.F.);
#34506=ORIENTED_EDGE('',*,*,#25044,.F.);
#34507=ORIENTED_EDGE('',*,*,#25675,.T.);
#34508=ORIENTED_EDGE('',*,*,#23928,.T.);
#34509=ORIENTED_EDGE('',*,*,#25673,.F.);
#34510=ORIENTED_EDGE('',*,*,#25043,.F.);
#34511=ORIENTED_EDGE('',*,*,#25676,.T.);
#34512=ORIENTED_EDGE('',*,*,#23929,.T.);
#34513=ORIENTED_EDGE('',*,*,#25675,.F.);
#34514=ORIENTED_EDGE('',*,*,#25048,.F.);
#34515=ORIENTED_EDGE('',*,*,#25677,.T.);
#34516=ORIENTED_EDGE('',*,*,#23930,.T.);
#34517=ORIENTED_EDGE('',*,*,#25676,.F.);
#34518=ORIENTED_EDGE('',*,*,#25047,.F.);
#34519=ORIENTED_EDGE('',*,*,#25678,.T.);
#34520=ORIENTED_EDGE('',*,*,#23931,.T.);
#34521=ORIENTED_EDGE('',*,*,#25677,.F.);
#34522=ORIENTED_EDGE('',*,*,#25046,.F.);
#34523=ORIENTED_EDGE('',*,*,#25674,.T.);
#34524=ORIENTED_EDGE('',*,*,#23932,.T.);
#34525=ORIENTED_EDGE('',*,*,#25678,.F.);
#34526=ORIENTED_EDGE('',*,*,#25045,.F.);
#34527=ORIENTED_EDGE('',*,*,#25679,.T.);
#34528=ORIENTED_EDGE('',*,*,#23921,.T.);
#34529=ORIENTED_EDGE('',*,*,#25680,.F.);
#34530=ORIENTED_EDGE('',*,*,#25038,.F.);
#34531=ORIENTED_EDGE('',*,*,#25681,.T.);
#34532=ORIENTED_EDGE('',*,*,#23922,.T.);
#34533=ORIENTED_EDGE('',*,*,#25679,.F.);
#34534=ORIENTED_EDGE('',*,*,#25037,.F.);
#34535=ORIENTED_EDGE('',*,*,#25682,.T.);
#34536=ORIENTED_EDGE('',*,*,#23923,.T.);
#34537=ORIENTED_EDGE('',*,*,#25681,.F.);
#34538=ORIENTED_EDGE('',*,*,#25042,.F.);
#34539=ORIENTED_EDGE('',*,*,#25683,.T.);
#34540=ORIENTED_EDGE('',*,*,#23924,.T.);
#34541=ORIENTED_EDGE('',*,*,#25682,.F.);
#34542=ORIENTED_EDGE('',*,*,#25041,.F.);
#34543=ORIENTED_EDGE('',*,*,#25684,.T.);
#34544=ORIENTED_EDGE('',*,*,#23925,.T.);
#34545=ORIENTED_EDGE('',*,*,#25683,.F.);
#34546=ORIENTED_EDGE('',*,*,#25040,.F.);
#34547=ORIENTED_EDGE('',*,*,#25680,.T.);
#34548=ORIENTED_EDGE('',*,*,#23926,.T.);
#34549=ORIENTED_EDGE('',*,*,#25684,.F.);
#34550=ORIENTED_EDGE('',*,*,#25039,.F.);
#34551=ORIENTED_EDGE('',*,*,#25685,.T.);
#34552=ORIENTED_EDGE('',*,*,#23915,.T.);
#34553=ORIENTED_EDGE('',*,*,#25686,.F.);
#34554=ORIENTED_EDGE('',*,*,#25032,.F.);
#34555=ORIENTED_EDGE('',*,*,#25687,.T.);
#34556=ORIENTED_EDGE('',*,*,#23916,.T.);
#34557=ORIENTED_EDGE('',*,*,#25685,.F.);
#34558=ORIENTED_EDGE('',*,*,#25031,.F.);
#34559=ORIENTED_EDGE('',*,*,#25688,.T.);
#34560=ORIENTED_EDGE('',*,*,#23917,.T.);
#34561=ORIENTED_EDGE('',*,*,#25687,.F.);
#34562=ORIENTED_EDGE('',*,*,#25036,.F.);
#34563=ORIENTED_EDGE('',*,*,#25689,.T.);
#34564=ORIENTED_EDGE('',*,*,#23918,.T.);
#34565=ORIENTED_EDGE('',*,*,#25688,.F.);
#34566=ORIENTED_EDGE('',*,*,#25035,.F.);
#34567=ORIENTED_EDGE('',*,*,#25690,.T.);
#34568=ORIENTED_EDGE('',*,*,#23919,.T.);
#34569=ORIENTED_EDGE('',*,*,#25689,.F.);
#34570=ORIENTED_EDGE('',*,*,#25034,.F.);
#34571=ORIENTED_EDGE('',*,*,#25686,.T.);
#34572=ORIENTED_EDGE('',*,*,#23920,.T.);
#34573=ORIENTED_EDGE('',*,*,#25690,.F.);
#34574=ORIENTED_EDGE('',*,*,#25033,.F.);
#34575=ORIENTED_EDGE('',*,*,#25691,.T.);
#34576=ORIENTED_EDGE('',*,*,#23909,.T.);
#34577=ORIENTED_EDGE('',*,*,#25692,.F.);
#34578=ORIENTED_EDGE('',*,*,#25026,.F.);
#34579=ORIENTED_EDGE('',*,*,#25693,.T.);
#34580=ORIENTED_EDGE('',*,*,#23910,.T.);
#34581=ORIENTED_EDGE('',*,*,#25691,.F.);
#34582=ORIENTED_EDGE('',*,*,#25025,.F.);
#34583=ORIENTED_EDGE('',*,*,#25694,.T.);
#34584=ORIENTED_EDGE('',*,*,#23911,.T.);
#34585=ORIENTED_EDGE('',*,*,#25693,.F.);
#34586=ORIENTED_EDGE('',*,*,#25030,.F.);
#34587=ORIENTED_EDGE('',*,*,#25695,.T.);
#34588=ORIENTED_EDGE('',*,*,#23912,.T.);
#34589=ORIENTED_EDGE('',*,*,#25694,.F.);
#34590=ORIENTED_EDGE('',*,*,#25029,.F.);
#34591=ORIENTED_EDGE('',*,*,#25696,.T.);
#34592=ORIENTED_EDGE('',*,*,#23913,.T.);
#34593=ORIENTED_EDGE('',*,*,#25695,.F.);
#34594=ORIENTED_EDGE('',*,*,#25028,.F.);
#34595=ORIENTED_EDGE('',*,*,#25692,.T.);
#34596=ORIENTED_EDGE('',*,*,#23914,.T.);
#34597=ORIENTED_EDGE('',*,*,#25696,.F.);
#34598=ORIENTED_EDGE('',*,*,#25027,.F.);
#34599=ORIENTED_EDGE('',*,*,#25697,.T.);
#34600=ORIENTED_EDGE('',*,*,#23903,.T.);
#34601=ORIENTED_EDGE('',*,*,#25698,.F.);
#34602=ORIENTED_EDGE('',*,*,#25020,.F.);
#34603=ORIENTED_EDGE('',*,*,#25699,.T.);
#34604=ORIENTED_EDGE('',*,*,#23904,.T.);
#34605=ORIENTED_EDGE('',*,*,#25697,.F.);
#34606=ORIENTED_EDGE('',*,*,#25019,.F.);
#34607=ORIENTED_EDGE('',*,*,#25700,.T.);
#34608=ORIENTED_EDGE('',*,*,#23905,.T.);
#34609=ORIENTED_EDGE('',*,*,#25699,.F.);
#34610=ORIENTED_EDGE('',*,*,#25024,.F.);
#34611=ORIENTED_EDGE('',*,*,#25701,.T.);
#34612=ORIENTED_EDGE('',*,*,#23906,.T.);
#34613=ORIENTED_EDGE('',*,*,#25700,.F.);
#34614=ORIENTED_EDGE('',*,*,#25023,.F.);
#34615=ORIENTED_EDGE('',*,*,#25702,.T.);
#34616=ORIENTED_EDGE('',*,*,#23907,.T.);
#34617=ORIENTED_EDGE('',*,*,#25701,.F.);
#34618=ORIENTED_EDGE('',*,*,#25022,.F.);
#34619=ORIENTED_EDGE('',*,*,#25698,.T.);
#34620=ORIENTED_EDGE('',*,*,#23908,.T.);
#34621=ORIENTED_EDGE('',*,*,#25702,.F.);
#34622=ORIENTED_EDGE('',*,*,#25021,.F.);
#34623=ORIENTED_EDGE('',*,*,#25703,.T.);
#34624=ORIENTED_EDGE('',*,*,#23897,.T.);
#34625=ORIENTED_EDGE('',*,*,#25704,.F.);
#34626=ORIENTED_EDGE('',*,*,#25014,.F.);
#34627=ORIENTED_EDGE('',*,*,#25705,.T.);
#34628=ORIENTED_EDGE('',*,*,#23898,.T.);
#34629=ORIENTED_EDGE('',*,*,#25703,.F.);
#34630=ORIENTED_EDGE('',*,*,#25013,.F.);
#34631=ORIENTED_EDGE('',*,*,#25706,.T.);
#34632=ORIENTED_EDGE('',*,*,#23899,.T.);
#34633=ORIENTED_EDGE('',*,*,#25705,.F.);
#34634=ORIENTED_EDGE('',*,*,#25018,.F.);
#34635=ORIENTED_EDGE('',*,*,#25707,.T.);
#34636=ORIENTED_EDGE('',*,*,#23900,.T.);
#34637=ORIENTED_EDGE('',*,*,#25706,.F.);
#34638=ORIENTED_EDGE('',*,*,#25017,.F.);
#34639=ORIENTED_EDGE('',*,*,#25708,.T.);
#34640=ORIENTED_EDGE('',*,*,#23901,.T.);
#34641=ORIENTED_EDGE('',*,*,#25707,.F.);
#34642=ORIENTED_EDGE('',*,*,#25016,.F.);
#34643=ORIENTED_EDGE('',*,*,#25704,.T.);
#34644=ORIENTED_EDGE('',*,*,#23902,.T.);
#34645=ORIENTED_EDGE('',*,*,#25708,.F.);
#34646=ORIENTED_EDGE('',*,*,#25015,.F.);
#34647=ORIENTED_EDGE('',*,*,#25709,.T.);
#34648=ORIENTED_EDGE('',*,*,#23891,.T.);
#34649=ORIENTED_EDGE('',*,*,#25710,.F.);
#34650=ORIENTED_EDGE('',*,*,#25008,.F.);
#34651=ORIENTED_EDGE('',*,*,#25711,.T.);
#34652=ORIENTED_EDGE('',*,*,#23892,.T.);
#34653=ORIENTED_EDGE('',*,*,#25709,.F.);
#34654=ORIENTED_EDGE('',*,*,#25007,.F.);
#34655=ORIENTED_EDGE('',*,*,#25712,.T.);
#34656=ORIENTED_EDGE('',*,*,#23893,.T.);
#34657=ORIENTED_EDGE('',*,*,#25711,.F.);
#34658=ORIENTED_EDGE('',*,*,#25012,.F.);
#34659=ORIENTED_EDGE('',*,*,#25713,.T.);
#34660=ORIENTED_EDGE('',*,*,#23894,.T.);
#34661=ORIENTED_EDGE('',*,*,#25712,.F.);
#34662=ORIENTED_EDGE('',*,*,#25011,.F.);
#34663=ORIENTED_EDGE('',*,*,#25714,.T.);
#34664=ORIENTED_EDGE('',*,*,#23895,.T.);
#34665=ORIENTED_EDGE('',*,*,#25713,.F.);
#34666=ORIENTED_EDGE('',*,*,#25010,.F.);
#34667=ORIENTED_EDGE('',*,*,#25710,.T.);
#34668=ORIENTED_EDGE('',*,*,#23896,.T.);
#34669=ORIENTED_EDGE('',*,*,#25714,.F.);
#34670=ORIENTED_EDGE('',*,*,#25009,.F.);
#34671=ORIENTED_EDGE('',*,*,#25715,.T.);
#34672=ORIENTED_EDGE('',*,*,#23885,.T.);
#34673=ORIENTED_EDGE('',*,*,#25716,.F.);
#34674=ORIENTED_EDGE('',*,*,#25002,.F.);
#34675=ORIENTED_EDGE('',*,*,#25717,.T.);
#34676=ORIENTED_EDGE('',*,*,#23886,.T.);
#34677=ORIENTED_EDGE('',*,*,#25715,.F.);
#34678=ORIENTED_EDGE('',*,*,#25001,.F.);
#34679=ORIENTED_EDGE('',*,*,#25718,.T.);
#34680=ORIENTED_EDGE('',*,*,#23887,.T.);
#34681=ORIENTED_EDGE('',*,*,#25717,.F.);
#34682=ORIENTED_EDGE('',*,*,#25006,.F.);
#34683=ORIENTED_EDGE('',*,*,#25719,.T.);
#34684=ORIENTED_EDGE('',*,*,#23888,.T.);
#34685=ORIENTED_EDGE('',*,*,#25718,.F.);
#34686=ORIENTED_EDGE('',*,*,#25005,.F.);
#34687=ORIENTED_EDGE('',*,*,#25720,.T.);
#34688=ORIENTED_EDGE('',*,*,#23889,.T.);
#34689=ORIENTED_EDGE('',*,*,#25719,.F.);
#34690=ORIENTED_EDGE('',*,*,#25004,.F.);
#34691=ORIENTED_EDGE('',*,*,#25716,.T.);
#34692=ORIENTED_EDGE('',*,*,#23890,.T.);
#34693=ORIENTED_EDGE('',*,*,#25720,.F.);
#34694=ORIENTED_EDGE('',*,*,#25003,.F.);
#34695=ORIENTED_EDGE('',*,*,#25721,.T.);
#34696=ORIENTED_EDGE('',*,*,#23879,.T.);
#34697=ORIENTED_EDGE('',*,*,#25722,.F.);
#34698=ORIENTED_EDGE('',*,*,#24996,.F.);
#34699=ORIENTED_EDGE('',*,*,#25723,.T.);
#34700=ORIENTED_EDGE('',*,*,#23880,.T.);
#34701=ORIENTED_EDGE('',*,*,#25721,.F.);
#34702=ORIENTED_EDGE('',*,*,#24995,.F.);
#34703=ORIENTED_EDGE('',*,*,#25724,.T.);
#34704=ORIENTED_EDGE('',*,*,#23881,.T.);
#34705=ORIENTED_EDGE('',*,*,#25723,.F.);
#34706=ORIENTED_EDGE('',*,*,#25000,.F.);
#34707=ORIENTED_EDGE('',*,*,#25725,.T.);
#34708=ORIENTED_EDGE('',*,*,#23882,.T.);
#34709=ORIENTED_EDGE('',*,*,#25724,.F.);
#34710=ORIENTED_EDGE('',*,*,#24999,.F.);
#34711=ORIENTED_EDGE('',*,*,#25726,.T.);
#34712=ORIENTED_EDGE('',*,*,#23883,.T.);
#34713=ORIENTED_EDGE('',*,*,#25725,.F.);
#34714=ORIENTED_EDGE('',*,*,#24998,.F.);
#34715=ORIENTED_EDGE('',*,*,#25722,.T.);
#34716=ORIENTED_EDGE('',*,*,#23884,.T.);
#34717=ORIENTED_EDGE('',*,*,#25726,.F.);
#34718=ORIENTED_EDGE('',*,*,#24997,.F.);
#34719=ORIENTED_EDGE('',*,*,#25727,.T.);
#34720=ORIENTED_EDGE('',*,*,#23873,.T.);
#34721=ORIENTED_EDGE('',*,*,#25728,.F.);
#34722=ORIENTED_EDGE('',*,*,#24990,.F.);
#34723=ORIENTED_EDGE('',*,*,#25729,.T.);
#34724=ORIENTED_EDGE('',*,*,#23874,.T.);
#34725=ORIENTED_EDGE('',*,*,#25727,.F.);
#34726=ORIENTED_EDGE('',*,*,#24989,.F.);
#34727=ORIENTED_EDGE('',*,*,#25730,.T.);
#34728=ORIENTED_EDGE('',*,*,#23875,.T.);
#34729=ORIENTED_EDGE('',*,*,#25729,.F.);
#34730=ORIENTED_EDGE('',*,*,#24994,.F.);
#34731=ORIENTED_EDGE('',*,*,#25731,.T.);
#34732=ORIENTED_EDGE('',*,*,#23876,.T.);
#34733=ORIENTED_EDGE('',*,*,#25730,.F.);
#34734=ORIENTED_EDGE('',*,*,#24993,.F.);
#34735=ORIENTED_EDGE('',*,*,#25732,.T.);
#34736=ORIENTED_EDGE('',*,*,#23877,.T.);
#34737=ORIENTED_EDGE('',*,*,#25731,.F.);
#34738=ORIENTED_EDGE('',*,*,#24992,.F.);
#34739=ORIENTED_EDGE('',*,*,#25728,.T.);
#34740=ORIENTED_EDGE('',*,*,#23878,.T.);
#34741=ORIENTED_EDGE('',*,*,#25732,.F.);
#34742=ORIENTED_EDGE('',*,*,#24991,.F.);
#34743=ORIENTED_EDGE('',*,*,#25733,.T.);
#34744=ORIENTED_EDGE('',*,*,#23867,.T.);
#34745=ORIENTED_EDGE('',*,*,#25734,.F.);
#34746=ORIENTED_EDGE('',*,*,#24984,.F.);
#34747=ORIENTED_EDGE('',*,*,#25735,.T.);
#34748=ORIENTED_EDGE('',*,*,#23868,.T.);
#34749=ORIENTED_EDGE('',*,*,#25733,.F.);
#34750=ORIENTED_EDGE('',*,*,#24983,.F.);
#34751=ORIENTED_EDGE('',*,*,#25736,.T.);
#34752=ORIENTED_EDGE('',*,*,#23869,.T.);
#34753=ORIENTED_EDGE('',*,*,#25735,.F.);
#34754=ORIENTED_EDGE('',*,*,#24988,.F.);
#34755=ORIENTED_EDGE('',*,*,#25737,.T.);
#34756=ORIENTED_EDGE('',*,*,#23870,.T.);
#34757=ORIENTED_EDGE('',*,*,#25736,.F.);
#34758=ORIENTED_EDGE('',*,*,#24987,.F.);
#34759=ORIENTED_EDGE('',*,*,#25738,.T.);
#34760=ORIENTED_EDGE('',*,*,#23871,.T.);
#34761=ORIENTED_EDGE('',*,*,#25737,.F.);
#34762=ORIENTED_EDGE('',*,*,#24986,.F.);
#34763=ORIENTED_EDGE('',*,*,#25734,.T.);
#34764=ORIENTED_EDGE('',*,*,#23872,.T.);
#34765=ORIENTED_EDGE('',*,*,#25738,.F.);
#34766=ORIENTED_EDGE('',*,*,#24985,.F.);
#34767=ORIENTED_EDGE('',*,*,#25739,.T.);
#34768=ORIENTED_EDGE('',*,*,#23861,.T.);
#34769=ORIENTED_EDGE('',*,*,#25740,.F.);
#34770=ORIENTED_EDGE('',*,*,#24978,.F.);
#34771=ORIENTED_EDGE('',*,*,#25741,.T.);
#34772=ORIENTED_EDGE('',*,*,#23862,.T.);
#34773=ORIENTED_EDGE('',*,*,#25739,.F.);
#34774=ORIENTED_EDGE('',*,*,#24977,.F.);
#34775=ORIENTED_EDGE('',*,*,#25742,.T.);
#34776=ORIENTED_EDGE('',*,*,#23863,.T.);
#34777=ORIENTED_EDGE('',*,*,#25741,.F.);
#34778=ORIENTED_EDGE('',*,*,#24982,.F.);
#34779=ORIENTED_EDGE('',*,*,#25743,.T.);
#34780=ORIENTED_EDGE('',*,*,#23864,.T.);
#34781=ORIENTED_EDGE('',*,*,#25742,.F.);
#34782=ORIENTED_EDGE('',*,*,#24981,.F.);
#34783=ORIENTED_EDGE('',*,*,#25744,.T.);
#34784=ORIENTED_EDGE('',*,*,#23865,.T.);
#34785=ORIENTED_EDGE('',*,*,#25743,.F.);
#34786=ORIENTED_EDGE('',*,*,#24980,.F.);
#34787=ORIENTED_EDGE('',*,*,#25740,.T.);
#34788=ORIENTED_EDGE('',*,*,#23866,.T.);
#34789=ORIENTED_EDGE('',*,*,#25744,.F.);
#34790=ORIENTED_EDGE('',*,*,#24979,.F.);
#34791=ORIENTED_EDGE('',*,*,#25745,.T.);
#34792=ORIENTED_EDGE('',*,*,#23855,.T.);
#34793=ORIENTED_EDGE('',*,*,#25746,.F.);
#34794=ORIENTED_EDGE('',*,*,#24972,.F.);
#34795=ORIENTED_EDGE('',*,*,#25747,.T.);
#34796=ORIENTED_EDGE('',*,*,#23856,.T.);
#34797=ORIENTED_EDGE('',*,*,#25745,.F.);
#34798=ORIENTED_EDGE('',*,*,#24971,.F.);
#34799=ORIENTED_EDGE('',*,*,#25748,.T.);
#34800=ORIENTED_EDGE('',*,*,#23857,.T.);
#34801=ORIENTED_EDGE('',*,*,#25747,.F.);
#34802=ORIENTED_EDGE('',*,*,#24976,.F.);
#34803=ORIENTED_EDGE('',*,*,#25749,.T.);
#34804=ORIENTED_EDGE('',*,*,#23858,.T.);
#34805=ORIENTED_EDGE('',*,*,#25748,.F.);
#34806=ORIENTED_EDGE('',*,*,#24975,.F.);
#34807=ORIENTED_EDGE('',*,*,#25750,.T.);
#34808=ORIENTED_EDGE('',*,*,#23859,.T.);
#34809=ORIENTED_EDGE('',*,*,#25749,.F.);
#34810=ORIENTED_EDGE('',*,*,#24974,.F.);
#34811=ORIENTED_EDGE('',*,*,#25746,.T.);
#34812=ORIENTED_EDGE('',*,*,#23860,.T.);
#34813=ORIENTED_EDGE('',*,*,#25750,.F.);
#34814=ORIENTED_EDGE('',*,*,#24973,.F.);
#34815=ORIENTED_EDGE('',*,*,#25751,.T.);
#34816=ORIENTED_EDGE('',*,*,#23849,.T.);
#34817=ORIENTED_EDGE('',*,*,#25752,.F.);
#34818=ORIENTED_EDGE('',*,*,#24966,.F.);
#34819=ORIENTED_EDGE('',*,*,#25753,.T.);
#34820=ORIENTED_EDGE('',*,*,#23850,.T.);
#34821=ORIENTED_EDGE('',*,*,#25751,.F.);
#34822=ORIENTED_EDGE('',*,*,#24965,.F.);
#34823=ORIENTED_EDGE('',*,*,#25754,.T.);
#34824=ORIENTED_EDGE('',*,*,#23851,.T.);
#34825=ORIENTED_EDGE('',*,*,#25753,.F.);
#34826=ORIENTED_EDGE('',*,*,#24970,.F.);
#34827=ORIENTED_EDGE('',*,*,#25755,.T.);
#34828=ORIENTED_EDGE('',*,*,#23852,.T.);
#34829=ORIENTED_EDGE('',*,*,#25754,.F.);
#34830=ORIENTED_EDGE('',*,*,#24969,.F.);
#34831=ORIENTED_EDGE('',*,*,#25756,.T.);
#34832=ORIENTED_EDGE('',*,*,#23853,.T.);
#34833=ORIENTED_EDGE('',*,*,#25755,.F.);
#34834=ORIENTED_EDGE('',*,*,#24968,.F.);
#34835=ORIENTED_EDGE('',*,*,#25752,.T.);
#34836=ORIENTED_EDGE('',*,*,#23854,.T.);
#34837=ORIENTED_EDGE('',*,*,#25756,.F.);
#34838=ORIENTED_EDGE('',*,*,#24967,.F.);
#34839=ORIENTED_EDGE('',*,*,#25757,.T.);
#34840=ORIENTED_EDGE('',*,*,#23843,.T.);
#34841=ORIENTED_EDGE('',*,*,#25758,.F.);
#34842=ORIENTED_EDGE('',*,*,#24960,.F.);
#34843=ORIENTED_EDGE('',*,*,#25759,.T.);
#34844=ORIENTED_EDGE('',*,*,#23844,.T.);
#34845=ORIENTED_EDGE('',*,*,#25757,.F.);
#34846=ORIENTED_EDGE('',*,*,#24959,.F.);
#34847=ORIENTED_EDGE('',*,*,#25760,.T.);
#34848=ORIENTED_EDGE('',*,*,#23845,.T.);
#34849=ORIENTED_EDGE('',*,*,#25759,.F.);
#34850=ORIENTED_EDGE('',*,*,#24964,.F.);
#34851=ORIENTED_EDGE('',*,*,#25761,.T.);
#34852=ORIENTED_EDGE('',*,*,#23846,.T.);
#34853=ORIENTED_EDGE('',*,*,#25760,.F.);
#34854=ORIENTED_EDGE('',*,*,#24963,.F.);
#34855=ORIENTED_EDGE('',*,*,#25762,.T.);
#34856=ORIENTED_EDGE('',*,*,#23847,.T.);
#34857=ORIENTED_EDGE('',*,*,#25761,.F.);
#34858=ORIENTED_EDGE('',*,*,#24962,.F.);
#34859=ORIENTED_EDGE('',*,*,#25758,.T.);
#34860=ORIENTED_EDGE('',*,*,#23848,.T.);
#34861=ORIENTED_EDGE('',*,*,#25762,.F.);
#34862=ORIENTED_EDGE('',*,*,#24961,.F.);
#34863=ORIENTED_EDGE('',*,*,#25763,.T.);
#34864=ORIENTED_EDGE('',*,*,#23837,.T.);
#34865=ORIENTED_EDGE('',*,*,#25764,.F.);
#34866=ORIENTED_EDGE('',*,*,#24954,.F.);
#34867=ORIENTED_EDGE('',*,*,#25765,.T.);
#34868=ORIENTED_EDGE('',*,*,#23838,.T.);
#34869=ORIENTED_EDGE('',*,*,#25763,.F.);
#34870=ORIENTED_EDGE('',*,*,#24953,.F.);
#34871=ORIENTED_EDGE('',*,*,#25766,.T.);
#34872=ORIENTED_EDGE('',*,*,#23839,.T.);
#34873=ORIENTED_EDGE('',*,*,#25765,.F.);
#34874=ORIENTED_EDGE('',*,*,#24958,.F.);
#34875=ORIENTED_EDGE('',*,*,#25767,.T.);
#34876=ORIENTED_EDGE('',*,*,#23840,.T.);
#34877=ORIENTED_EDGE('',*,*,#25766,.F.);
#34878=ORIENTED_EDGE('',*,*,#24957,.F.);
#34879=ORIENTED_EDGE('',*,*,#25768,.T.);
#34880=ORIENTED_EDGE('',*,*,#23841,.T.);
#34881=ORIENTED_EDGE('',*,*,#25767,.F.);
#34882=ORIENTED_EDGE('',*,*,#24956,.F.);
#34883=ORIENTED_EDGE('',*,*,#25764,.T.);
#34884=ORIENTED_EDGE('',*,*,#23842,.T.);
#34885=ORIENTED_EDGE('',*,*,#25768,.F.);
#34886=ORIENTED_EDGE('',*,*,#24955,.F.);
#34887=ORIENTED_EDGE('',*,*,#25769,.T.);
#34888=ORIENTED_EDGE('',*,*,#23831,.T.);
#34889=ORIENTED_EDGE('',*,*,#25770,.F.);
#34890=ORIENTED_EDGE('',*,*,#24948,.F.);
#34891=ORIENTED_EDGE('',*,*,#25771,.T.);
#34892=ORIENTED_EDGE('',*,*,#23832,.T.);
#34893=ORIENTED_EDGE('',*,*,#25769,.F.);
#34894=ORIENTED_EDGE('',*,*,#24947,.F.);
#34895=ORIENTED_EDGE('',*,*,#25772,.T.);
#34896=ORIENTED_EDGE('',*,*,#23833,.T.);
#34897=ORIENTED_EDGE('',*,*,#25771,.F.);
#34898=ORIENTED_EDGE('',*,*,#24952,.F.);
#34899=ORIENTED_EDGE('',*,*,#25773,.T.);
#34900=ORIENTED_EDGE('',*,*,#23834,.T.);
#34901=ORIENTED_EDGE('',*,*,#25772,.F.);
#34902=ORIENTED_EDGE('',*,*,#24951,.F.);
#34903=ORIENTED_EDGE('',*,*,#25774,.T.);
#34904=ORIENTED_EDGE('',*,*,#23835,.T.);
#34905=ORIENTED_EDGE('',*,*,#25773,.F.);
#34906=ORIENTED_EDGE('',*,*,#24950,.F.);
#34907=ORIENTED_EDGE('',*,*,#25770,.T.);
#34908=ORIENTED_EDGE('',*,*,#23836,.T.);
#34909=ORIENTED_EDGE('',*,*,#25774,.F.);
#34910=ORIENTED_EDGE('',*,*,#24949,.F.);
#34911=ORIENTED_EDGE('',*,*,#25775,.T.);
#34912=ORIENTED_EDGE('',*,*,#23825,.T.);
#34913=ORIENTED_EDGE('',*,*,#25776,.F.);
#34914=ORIENTED_EDGE('',*,*,#24942,.F.);
#34915=ORIENTED_EDGE('',*,*,#25777,.T.);
#34916=ORIENTED_EDGE('',*,*,#23826,.T.);
#34917=ORIENTED_EDGE('',*,*,#25775,.F.);
#34918=ORIENTED_EDGE('',*,*,#24941,.F.);
#34919=ORIENTED_EDGE('',*,*,#25778,.T.);
#34920=ORIENTED_EDGE('',*,*,#23827,.T.);
#34921=ORIENTED_EDGE('',*,*,#25777,.F.);
#34922=ORIENTED_EDGE('',*,*,#24946,.F.);
#34923=ORIENTED_EDGE('',*,*,#25779,.T.);
#34924=ORIENTED_EDGE('',*,*,#23828,.T.);
#34925=ORIENTED_EDGE('',*,*,#25778,.F.);
#34926=ORIENTED_EDGE('',*,*,#24945,.F.);
#34927=ORIENTED_EDGE('',*,*,#25780,.T.);
#34928=ORIENTED_EDGE('',*,*,#23829,.T.);
#34929=ORIENTED_EDGE('',*,*,#25779,.F.);
#34930=ORIENTED_EDGE('',*,*,#24944,.F.);
#34931=ORIENTED_EDGE('',*,*,#25776,.T.);
#34932=ORIENTED_EDGE('',*,*,#23830,.T.);
#34933=ORIENTED_EDGE('',*,*,#25780,.F.);
#34934=ORIENTED_EDGE('',*,*,#24943,.F.);
#34935=ORIENTED_EDGE('',*,*,#25781,.T.);
#34936=ORIENTED_EDGE('',*,*,#23819,.T.);
#34937=ORIENTED_EDGE('',*,*,#25782,.F.);
#34938=ORIENTED_EDGE('',*,*,#24936,.F.);
#34939=ORIENTED_EDGE('',*,*,#25783,.T.);
#34940=ORIENTED_EDGE('',*,*,#23820,.T.);
#34941=ORIENTED_EDGE('',*,*,#25781,.F.);
#34942=ORIENTED_EDGE('',*,*,#24935,.F.);
#34943=ORIENTED_EDGE('',*,*,#25784,.T.);
#34944=ORIENTED_EDGE('',*,*,#23821,.T.);
#34945=ORIENTED_EDGE('',*,*,#25783,.F.);
#34946=ORIENTED_EDGE('',*,*,#24940,.F.);
#34947=ORIENTED_EDGE('',*,*,#25785,.T.);
#34948=ORIENTED_EDGE('',*,*,#23822,.T.);
#34949=ORIENTED_EDGE('',*,*,#25784,.F.);
#34950=ORIENTED_EDGE('',*,*,#24939,.F.);
#34951=ORIENTED_EDGE('',*,*,#25786,.T.);
#34952=ORIENTED_EDGE('',*,*,#23823,.T.);
#34953=ORIENTED_EDGE('',*,*,#25785,.F.);
#34954=ORIENTED_EDGE('',*,*,#24938,.F.);
#34955=ORIENTED_EDGE('',*,*,#25782,.T.);
#34956=ORIENTED_EDGE('',*,*,#23824,.T.);
#34957=ORIENTED_EDGE('',*,*,#25786,.F.);
#34958=ORIENTED_EDGE('',*,*,#24937,.F.);
#34959=ORIENTED_EDGE('',*,*,#25787,.T.);
#34960=ORIENTED_EDGE('',*,*,#23813,.T.);
#34961=ORIENTED_EDGE('',*,*,#25788,.F.);
#34962=ORIENTED_EDGE('',*,*,#24930,.F.);
#34963=ORIENTED_EDGE('',*,*,#25789,.T.);
#34964=ORIENTED_EDGE('',*,*,#23814,.T.);
#34965=ORIENTED_EDGE('',*,*,#25787,.F.);
#34966=ORIENTED_EDGE('',*,*,#24929,.F.);
#34967=ORIENTED_EDGE('',*,*,#25790,.T.);
#34968=ORIENTED_EDGE('',*,*,#23815,.T.);
#34969=ORIENTED_EDGE('',*,*,#25789,.F.);
#34970=ORIENTED_EDGE('',*,*,#24934,.F.);
#34971=ORIENTED_EDGE('',*,*,#25791,.T.);
#34972=ORIENTED_EDGE('',*,*,#23816,.T.);
#34973=ORIENTED_EDGE('',*,*,#25790,.F.);
#34974=ORIENTED_EDGE('',*,*,#24933,.F.);
#34975=ORIENTED_EDGE('',*,*,#25792,.T.);
#34976=ORIENTED_EDGE('',*,*,#23817,.T.);
#34977=ORIENTED_EDGE('',*,*,#25791,.F.);
#34978=ORIENTED_EDGE('',*,*,#24932,.F.);
#34979=ORIENTED_EDGE('',*,*,#25788,.T.);
#34980=ORIENTED_EDGE('',*,*,#23818,.T.);
#34981=ORIENTED_EDGE('',*,*,#25792,.F.);
#34982=ORIENTED_EDGE('',*,*,#24931,.F.);
#34983=ORIENTED_EDGE('',*,*,#25793,.T.);
#34984=ORIENTED_EDGE('',*,*,#23807,.T.);
#34985=ORIENTED_EDGE('',*,*,#25794,.F.);
#34986=ORIENTED_EDGE('',*,*,#24924,.F.);
#34987=ORIENTED_EDGE('',*,*,#25795,.T.);
#34988=ORIENTED_EDGE('',*,*,#23808,.T.);
#34989=ORIENTED_EDGE('',*,*,#25793,.F.);
#34990=ORIENTED_EDGE('',*,*,#24923,.F.);
#34991=ORIENTED_EDGE('',*,*,#25796,.T.);
#34992=ORIENTED_EDGE('',*,*,#23809,.T.);
#34993=ORIENTED_EDGE('',*,*,#25795,.F.);
#34994=ORIENTED_EDGE('',*,*,#24928,.F.);
#34995=ORIENTED_EDGE('',*,*,#25797,.T.);
#34996=ORIENTED_EDGE('',*,*,#23810,.T.);
#34997=ORIENTED_EDGE('',*,*,#25796,.F.);
#34998=ORIENTED_EDGE('',*,*,#24927,.F.);
#34999=ORIENTED_EDGE('',*,*,#25798,.T.);
#35000=ORIENTED_EDGE('',*,*,#23811,.T.);
#35001=ORIENTED_EDGE('',*,*,#25797,.F.);
#35002=ORIENTED_EDGE('',*,*,#24926,.F.);
#35003=ORIENTED_EDGE('',*,*,#25794,.T.);
#35004=ORIENTED_EDGE('',*,*,#23812,.T.);
#35005=ORIENTED_EDGE('',*,*,#25798,.F.);
#35006=ORIENTED_EDGE('',*,*,#24925,.F.);
#35007=ORIENTED_EDGE('',*,*,#25799,.T.);
#35008=ORIENTED_EDGE('',*,*,#23801,.T.);
#35009=ORIENTED_EDGE('',*,*,#25800,.F.);
#35010=ORIENTED_EDGE('',*,*,#24918,.F.);
#35011=ORIENTED_EDGE('',*,*,#25801,.T.);
#35012=ORIENTED_EDGE('',*,*,#23802,.T.);
#35013=ORIENTED_EDGE('',*,*,#25799,.F.);
#35014=ORIENTED_EDGE('',*,*,#24917,.F.);
#35015=ORIENTED_EDGE('',*,*,#25802,.T.);
#35016=ORIENTED_EDGE('',*,*,#23803,.T.);
#35017=ORIENTED_EDGE('',*,*,#25801,.F.);
#35018=ORIENTED_EDGE('',*,*,#24922,.F.);
#35019=ORIENTED_EDGE('',*,*,#25803,.T.);
#35020=ORIENTED_EDGE('',*,*,#23804,.T.);
#35021=ORIENTED_EDGE('',*,*,#25802,.F.);
#35022=ORIENTED_EDGE('',*,*,#24921,.F.);
#35023=ORIENTED_EDGE('',*,*,#25804,.T.);
#35024=ORIENTED_EDGE('',*,*,#23805,.T.);
#35025=ORIENTED_EDGE('',*,*,#25803,.F.);
#35026=ORIENTED_EDGE('',*,*,#24920,.F.);
#35027=ORIENTED_EDGE('',*,*,#25800,.T.);
#35028=ORIENTED_EDGE('',*,*,#23806,.T.);
#35029=ORIENTED_EDGE('',*,*,#25804,.F.);
#35030=ORIENTED_EDGE('',*,*,#24919,.F.);
#35031=ORIENTED_EDGE('',*,*,#25805,.T.);
#35032=ORIENTED_EDGE('',*,*,#23795,.T.);
#35033=ORIENTED_EDGE('',*,*,#25806,.F.);
#35034=ORIENTED_EDGE('',*,*,#24912,.F.);
#35035=ORIENTED_EDGE('',*,*,#25807,.T.);
#35036=ORIENTED_EDGE('',*,*,#23796,.T.);
#35037=ORIENTED_EDGE('',*,*,#25805,.F.);
#35038=ORIENTED_EDGE('',*,*,#24911,.F.);
#35039=ORIENTED_EDGE('',*,*,#25808,.T.);
#35040=ORIENTED_EDGE('',*,*,#23797,.T.);
#35041=ORIENTED_EDGE('',*,*,#25807,.F.);
#35042=ORIENTED_EDGE('',*,*,#24916,.F.);
#35043=ORIENTED_EDGE('',*,*,#25809,.T.);
#35044=ORIENTED_EDGE('',*,*,#23798,.T.);
#35045=ORIENTED_EDGE('',*,*,#25808,.F.);
#35046=ORIENTED_EDGE('',*,*,#24915,.F.);
#35047=ORIENTED_EDGE('',*,*,#25810,.T.);
#35048=ORIENTED_EDGE('',*,*,#23799,.T.);
#35049=ORIENTED_EDGE('',*,*,#25809,.F.);
#35050=ORIENTED_EDGE('',*,*,#24914,.F.);
#35051=ORIENTED_EDGE('',*,*,#25806,.T.);
#35052=ORIENTED_EDGE('',*,*,#23800,.T.);
#35053=ORIENTED_EDGE('',*,*,#25810,.F.);
#35054=ORIENTED_EDGE('',*,*,#24913,.F.);
#35055=ORIENTED_EDGE('',*,*,#25811,.T.);
#35056=ORIENTED_EDGE('',*,*,#23789,.T.);
#35057=ORIENTED_EDGE('',*,*,#25812,.F.);
#35058=ORIENTED_EDGE('',*,*,#24906,.F.);
#35059=ORIENTED_EDGE('',*,*,#25813,.T.);
#35060=ORIENTED_EDGE('',*,*,#23790,.T.);
#35061=ORIENTED_EDGE('',*,*,#25811,.F.);
#35062=ORIENTED_EDGE('',*,*,#24905,.F.);
#35063=ORIENTED_EDGE('',*,*,#25814,.T.);
#35064=ORIENTED_EDGE('',*,*,#23791,.T.);
#35065=ORIENTED_EDGE('',*,*,#25813,.F.);
#35066=ORIENTED_EDGE('',*,*,#24910,.F.);
#35067=ORIENTED_EDGE('',*,*,#25815,.T.);
#35068=ORIENTED_EDGE('',*,*,#23792,.T.);
#35069=ORIENTED_EDGE('',*,*,#25814,.F.);
#35070=ORIENTED_EDGE('',*,*,#24909,.F.);
#35071=ORIENTED_EDGE('',*,*,#25816,.T.);
#35072=ORIENTED_EDGE('',*,*,#23793,.T.);
#35073=ORIENTED_EDGE('',*,*,#25815,.F.);
#35074=ORIENTED_EDGE('',*,*,#24908,.F.);
#35075=ORIENTED_EDGE('',*,*,#25812,.T.);
#35076=ORIENTED_EDGE('',*,*,#23794,.T.);
#35077=ORIENTED_EDGE('',*,*,#25816,.F.);
#35078=ORIENTED_EDGE('',*,*,#24907,.F.);
#35079=ORIENTED_EDGE('',*,*,#25817,.T.);
#35080=ORIENTED_EDGE('',*,*,#23783,.T.);
#35081=ORIENTED_EDGE('',*,*,#25818,.F.);
#35082=ORIENTED_EDGE('',*,*,#24900,.F.);
#35083=ORIENTED_EDGE('',*,*,#25819,.T.);
#35084=ORIENTED_EDGE('',*,*,#23784,.T.);
#35085=ORIENTED_EDGE('',*,*,#25817,.F.);
#35086=ORIENTED_EDGE('',*,*,#24899,.F.);
#35087=ORIENTED_EDGE('',*,*,#25820,.T.);
#35088=ORIENTED_EDGE('',*,*,#23785,.T.);
#35089=ORIENTED_EDGE('',*,*,#25819,.F.);
#35090=ORIENTED_EDGE('',*,*,#24904,.F.);
#35091=ORIENTED_EDGE('',*,*,#25821,.T.);
#35092=ORIENTED_EDGE('',*,*,#23786,.T.);
#35093=ORIENTED_EDGE('',*,*,#25820,.F.);
#35094=ORIENTED_EDGE('',*,*,#24903,.F.);
#35095=ORIENTED_EDGE('',*,*,#25822,.T.);
#35096=ORIENTED_EDGE('',*,*,#23787,.T.);
#35097=ORIENTED_EDGE('',*,*,#25821,.F.);
#35098=ORIENTED_EDGE('',*,*,#24902,.F.);
#35099=ORIENTED_EDGE('',*,*,#25818,.T.);
#35100=ORIENTED_EDGE('',*,*,#23788,.T.);
#35101=ORIENTED_EDGE('',*,*,#25822,.F.);
#35102=ORIENTED_EDGE('',*,*,#24901,.F.);
#35103=ORIENTED_EDGE('',*,*,#25823,.T.);
#35104=ORIENTED_EDGE('',*,*,#23777,.T.);
#35105=ORIENTED_EDGE('',*,*,#25824,.F.);
#35106=ORIENTED_EDGE('',*,*,#24894,.F.);
#35107=ORIENTED_EDGE('',*,*,#25825,.T.);
#35108=ORIENTED_EDGE('',*,*,#23778,.T.);
#35109=ORIENTED_EDGE('',*,*,#25823,.F.);
#35110=ORIENTED_EDGE('',*,*,#24893,.F.);
#35111=ORIENTED_EDGE('',*,*,#25826,.T.);
#35112=ORIENTED_EDGE('',*,*,#23779,.T.);
#35113=ORIENTED_EDGE('',*,*,#25825,.F.);
#35114=ORIENTED_EDGE('',*,*,#24898,.F.);
#35115=ORIENTED_EDGE('',*,*,#25827,.T.);
#35116=ORIENTED_EDGE('',*,*,#23780,.T.);
#35117=ORIENTED_EDGE('',*,*,#25826,.F.);
#35118=ORIENTED_EDGE('',*,*,#24897,.F.);
#35119=ORIENTED_EDGE('',*,*,#25828,.T.);
#35120=ORIENTED_EDGE('',*,*,#23781,.T.);
#35121=ORIENTED_EDGE('',*,*,#25827,.F.);
#35122=ORIENTED_EDGE('',*,*,#24896,.F.);
#35123=ORIENTED_EDGE('',*,*,#25824,.T.);
#35124=ORIENTED_EDGE('',*,*,#23782,.T.);
#35125=ORIENTED_EDGE('',*,*,#25828,.F.);
#35126=ORIENTED_EDGE('',*,*,#24895,.F.);
#35127=ORIENTED_EDGE('',*,*,#25829,.T.);
#35128=ORIENTED_EDGE('',*,*,#23771,.T.);
#35129=ORIENTED_EDGE('',*,*,#25830,.F.);
#35130=ORIENTED_EDGE('',*,*,#24888,.F.);
#35131=ORIENTED_EDGE('',*,*,#25831,.T.);
#35132=ORIENTED_EDGE('',*,*,#23772,.T.);
#35133=ORIENTED_EDGE('',*,*,#25829,.F.);
#35134=ORIENTED_EDGE('',*,*,#24887,.F.);
#35135=ORIENTED_EDGE('',*,*,#25832,.T.);
#35136=ORIENTED_EDGE('',*,*,#23773,.T.);
#35137=ORIENTED_EDGE('',*,*,#25831,.F.);
#35138=ORIENTED_EDGE('',*,*,#24892,.F.);
#35139=ORIENTED_EDGE('',*,*,#25833,.T.);
#35140=ORIENTED_EDGE('',*,*,#23774,.T.);
#35141=ORIENTED_EDGE('',*,*,#25832,.F.);
#35142=ORIENTED_EDGE('',*,*,#24891,.F.);
#35143=ORIENTED_EDGE('',*,*,#25834,.T.);
#35144=ORIENTED_EDGE('',*,*,#23775,.T.);
#35145=ORIENTED_EDGE('',*,*,#25833,.F.);
#35146=ORIENTED_EDGE('',*,*,#24890,.F.);
#35147=ORIENTED_EDGE('',*,*,#25830,.T.);
#35148=ORIENTED_EDGE('',*,*,#23776,.T.);
#35149=ORIENTED_EDGE('',*,*,#25834,.F.);
#35150=ORIENTED_EDGE('',*,*,#24889,.F.);
#35151=ORIENTED_EDGE('',*,*,#25835,.T.);
#35152=ORIENTED_EDGE('',*,*,#23765,.T.);
#35153=ORIENTED_EDGE('',*,*,#25836,.F.);
#35154=ORIENTED_EDGE('',*,*,#24882,.F.);
#35155=ORIENTED_EDGE('',*,*,#25837,.T.);
#35156=ORIENTED_EDGE('',*,*,#23766,.T.);
#35157=ORIENTED_EDGE('',*,*,#25835,.F.);
#35158=ORIENTED_EDGE('',*,*,#24881,.F.);
#35159=ORIENTED_EDGE('',*,*,#25838,.T.);
#35160=ORIENTED_EDGE('',*,*,#23767,.T.);
#35161=ORIENTED_EDGE('',*,*,#25837,.F.);
#35162=ORIENTED_EDGE('',*,*,#24886,.F.);
#35163=ORIENTED_EDGE('',*,*,#25839,.T.);
#35164=ORIENTED_EDGE('',*,*,#23768,.T.);
#35165=ORIENTED_EDGE('',*,*,#25838,.F.);
#35166=ORIENTED_EDGE('',*,*,#24885,.F.);
#35167=ORIENTED_EDGE('',*,*,#25840,.T.);
#35168=ORIENTED_EDGE('',*,*,#23769,.T.);
#35169=ORIENTED_EDGE('',*,*,#25839,.F.);
#35170=ORIENTED_EDGE('',*,*,#24884,.F.);
#35171=ORIENTED_EDGE('',*,*,#25836,.T.);
#35172=ORIENTED_EDGE('',*,*,#23770,.T.);
#35173=ORIENTED_EDGE('',*,*,#25840,.F.);
#35174=ORIENTED_EDGE('',*,*,#24883,.F.);
#35175=ORIENTED_EDGE('',*,*,#25841,.T.);
#35176=ORIENTED_EDGE('',*,*,#23759,.T.);
#35177=ORIENTED_EDGE('',*,*,#25842,.F.);
#35178=ORIENTED_EDGE('',*,*,#24876,.F.);
#35179=ORIENTED_EDGE('',*,*,#25843,.T.);
#35180=ORIENTED_EDGE('',*,*,#23760,.T.);
#35181=ORIENTED_EDGE('',*,*,#25841,.F.);
#35182=ORIENTED_EDGE('',*,*,#24875,.F.);
#35183=ORIENTED_EDGE('',*,*,#25844,.T.);
#35184=ORIENTED_EDGE('',*,*,#23761,.T.);
#35185=ORIENTED_EDGE('',*,*,#25843,.F.);
#35186=ORIENTED_EDGE('',*,*,#24880,.F.);
#35187=ORIENTED_EDGE('',*,*,#25845,.T.);
#35188=ORIENTED_EDGE('',*,*,#23762,.T.);
#35189=ORIENTED_EDGE('',*,*,#25844,.F.);
#35190=ORIENTED_EDGE('',*,*,#24879,.F.);
#35191=ORIENTED_EDGE('',*,*,#25846,.T.);
#35192=ORIENTED_EDGE('',*,*,#23763,.T.);
#35193=ORIENTED_EDGE('',*,*,#25845,.F.);
#35194=ORIENTED_EDGE('',*,*,#24878,.F.);
#35195=ORIENTED_EDGE('',*,*,#25842,.T.);
#35196=ORIENTED_EDGE('',*,*,#23764,.T.);
#35197=ORIENTED_EDGE('',*,*,#25846,.F.);
#35198=ORIENTED_EDGE('',*,*,#24877,.F.);
#35199=ORIENTED_EDGE('',*,*,#25847,.T.);
#35200=ORIENTED_EDGE('',*,*,#23753,.T.);
#35201=ORIENTED_EDGE('',*,*,#25848,.F.);
#35202=ORIENTED_EDGE('',*,*,#24870,.F.);
#35203=ORIENTED_EDGE('',*,*,#25849,.T.);
#35204=ORIENTED_EDGE('',*,*,#23754,.T.);
#35205=ORIENTED_EDGE('',*,*,#25847,.F.);
#35206=ORIENTED_EDGE('',*,*,#24869,.F.);
#35207=ORIENTED_EDGE('',*,*,#25850,.T.);
#35208=ORIENTED_EDGE('',*,*,#23755,.T.);
#35209=ORIENTED_EDGE('',*,*,#25849,.F.);
#35210=ORIENTED_EDGE('',*,*,#24874,.F.);
#35211=ORIENTED_EDGE('',*,*,#25851,.T.);
#35212=ORIENTED_EDGE('',*,*,#23756,.T.);
#35213=ORIENTED_EDGE('',*,*,#25850,.F.);
#35214=ORIENTED_EDGE('',*,*,#24873,.F.);
#35215=ORIENTED_EDGE('',*,*,#25852,.T.);
#35216=ORIENTED_EDGE('',*,*,#23757,.T.);
#35217=ORIENTED_EDGE('',*,*,#25851,.F.);
#35218=ORIENTED_EDGE('',*,*,#24872,.F.);
#35219=ORIENTED_EDGE('',*,*,#25848,.T.);
#35220=ORIENTED_EDGE('',*,*,#23758,.T.);
#35221=ORIENTED_EDGE('',*,*,#25852,.F.);
#35222=ORIENTED_EDGE('',*,*,#24871,.F.);
#35223=ORIENTED_EDGE('',*,*,#25853,.T.);
#35224=ORIENTED_EDGE('',*,*,#23747,.T.);
#35225=ORIENTED_EDGE('',*,*,#25854,.F.);
#35226=ORIENTED_EDGE('',*,*,#24864,.F.);
#35227=ORIENTED_EDGE('',*,*,#25855,.T.);
#35228=ORIENTED_EDGE('',*,*,#23748,.T.);
#35229=ORIENTED_EDGE('',*,*,#25853,.F.);
#35230=ORIENTED_EDGE('',*,*,#24863,.F.);
#35231=ORIENTED_EDGE('',*,*,#25856,.T.);
#35232=ORIENTED_EDGE('',*,*,#23749,.T.);
#35233=ORIENTED_EDGE('',*,*,#25855,.F.);
#35234=ORIENTED_EDGE('',*,*,#24868,.F.);
#35235=ORIENTED_EDGE('',*,*,#25857,.T.);
#35236=ORIENTED_EDGE('',*,*,#23750,.T.);
#35237=ORIENTED_EDGE('',*,*,#25856,.F.);
#35238=ORIENTED_EDGE('',*,*,#24867,.F.);
#35239=ORIENTED_EDGE('',*,*,#25858,.T.);
#35240=ORIENTED_EDGE('',*,*,#23751,.T.);
#35241=ORIENTED_EDGE('',*,*,#25857,.F.);
#35242=ORIENTED_EDGE('',*,*,#24866,.F.);
#35243=ORIENTED_EDGE('',*,*,#25854,.T.);
#35244=ORIENTED_EDGE('',*,*,#23752,.T.);
#35245=ORIENTED_EDGE('',*,*,#25858,.F.);
#35246=ORIENTED_EDGE('',*,*,#24865,.F.);
#35247=ORIENTED_EDGE('',*,*,#25859,.T.);
#35248=ORIENTED_EDGE('',*,*,#23741,.T.);
#35249=ORIENTED_EDGE('',*,*,#25860,.F.);
#35250=ORIENTED_EDGE('',*,*,#24858,.F.);
#35251=ORIENTED_EDGE('',*,*,#25861,.T.);
#35252=ORIENTED_EDGE('',*,*,#23742,.T.);
#35253=ORIENTED_EDGE('',*,*,#25859,.F.);
#35254=ORIENTED_EDGE('',*,*,#24857,.F.);
#35255=ORIENTED_EDGE('',*,*,#25862,.T.);
#35256=ORIENTED_EDGE('',*,*,#23743,.T.);
#35257=ORIENTED_EDGE('',*,*,#25861,.F.);
#35258=ORIENTED_EDGE('',*,*,#24862,.F.);
#35259=ORIENTED_EDGE('',*,*,#25863,.T.);
#35260=ORIENTED_EDGE('',*,*,#23744,.T.);
#35261=ORIENTED_EDGE('',*,*,#25862,.F.);
#35262=ORIENTED_EDGE('',*,*,#24861,.F.);
#35263=ORIENTED_EDGE('',*,*,#25864,.T.);
#35264=ORIENTED_EDGE('',*,*,#23745,.T.);
#35265=ORIENTED_EDGE('',*,*,#25863,.F.);
#35266=ORIENTED_EDGE('',*,*,#24860,.F.);
#35267=ORIENTED_EDGE('',*,*,#25860,.T.);
#35268=ORIENTED_EDGE('',*,*,#23746,.T.);
#35269=ORIENTED_EDGE('',*,*,#25864,.F.);
#35270=ORIENTED_EDGE('',*,*,#24859,.F.);
#35271=ORIENTED_EDGE('',*,*,#25865,.T.);
#35272=ORIENTED_EDGE('',*,*,#23735,.T.);
#35273=ORIENTED_EDGE('',*,*,#25866,.F.);
#35274=ORIENTED_EDGE('',*,*,#24852,.F.);
#35275=ORIENTED_EDGE('',*,*,#25867,.T.);
#35276=ORIENTED_EDGE('',*,*,#23736,.T.);
#35277=ORIENTED_EDGE('',*,*,#25865,.F.);
#35278=ORIENTED_EDGE('',*,*,#24851,.F.);
#35279=ORIENTED_EDGE('',*,*,#25868,.T.);
#35280=ORIENTED_EDGE('',*,*,#23737,.T.);
#35281=ORIENTED_EDGE('',*,*,#25867,.F.);
#35282=ORIENTED_EDGE('',*,*,#24856,.F.);
#35283=ORIENTED_EDGE('',*,*,#25869,.T.);
#35284=ORIENTED_EDGE('',*,*,#23738,.T.);
#35285=ORIENTED_EDGE('',*,*,#25868,.F.);
#35286=ORIENTED_EDGE('',*,*,#24855,.F.);
#35287=ORIENTED_EDGE('',*,*,#25870,.T.);
#35288=ORIENTED_EDGE('',*,*,#23739,.T.);
#35289=ORIENTED_EDGE('',*,*,#25869,.F.);
#35290=ORIENTED_EDGE('',*,*,#24854,.F.);
#35291=ORIENTED_EDGE('',*,*,#25866,.T.);
#35292=ORIENTED_EDGE('',*,*,#23740,.T.);
#35293=ORIENTED_EDGE('',*,*,#25870,.F.);
#35294=ORIENTED_EDGE('',*,*,#24853,.F.);
#35295=ORIENTED_EDGE('',*,*,#25871,.T.);
#35296=ORIENTED_EDGE('',*,*,#23729,.T.);
#35297=ORIENTED_EDGE('',*,*,#25872,.F.);
#35298=ORIENTED_EDGE('',*,*,#24846,.F.);
#35299=ORIENTED_EDGE('',*,*,#25873,.T.);
#35300=ORIENTED_EDGE('',*,*,#23730,.T.);
#35301=ORIENTED_EDGE('',*,*,#25871,.F.);
#35302=ORIENTED_EDGE('',*,*,#24845,.F.);
#35303=ORIENTED_EDGE('',*,*,#25874,.T.);
#35304=ORIENTED_EDGE('',*,*,#23731,.T.);
#35305=ORIENTED_EDGE('',*,*,#25873,.F.);
#35306=ORIENTED_EDGE('',*,*,#24850,.F.);
#35307=ORIENTED_EDGE('',*,*,#25875,.T.);
#35308=ORIENTED_EDGE('',*,*,#23732,.T.);
#35309=ORIENTED_EDGE('',*,*,#25874,.F.);
#35310=ORIENTED_EDGE('',*,*,#24849,.F.);
#35311=ORIENTED_EDGE('',*,*,#25876,.T.);
#35312=ORIENTED_EDGE('',*,*,#23733,.T.);
#35313=ORIENTED_EDGE('',*,*,#25875,.F.);
#35314=ORIENTED_EDGE('',*,*,#24848,.F.);
#35315=ORIENTED_EDGE('',*,*,#25872,.T.);
#35316=ORIENTED_EDGE('',*,*,#23734,.T.);
#35317=ORIENTED_EDGE('',*,*,#25876,.F.);
#35318=ORIENTED_EDGE('',*,*,#24847,.F.);
#35319=ORIENTED_EDGE('',*,*,#25877,.T.);
#35320=ORIENTED_EDGE('',*,*,#23723,.T.);
#35321=ORIENTED_EDGE('',*,*,#25878,.F.);
#35322=ORIENTED_EDGE('',*,*,#24840,.F.);
#35323=ORIENTED_EDGE('',*,*,#25879,.T.);
#35324=ORIENTED_EDGE('',*,*,#23724,.T.);
#35325=ORIENTED_EDGE('',*,*,#25877,.F.);
#35326=ORIENTED_EDGE('',*,*,#24839,.F.);
#35327=ORIENTED_EDGE('',*,*,#25880,.T.);
#35328=ORIENTED_EDGE('',*,*,#23725,.T.);
#35329=ORIENTED_EDGE('',*,*,#25879,.F.);
#35330=ORIENTED_EDGE('',*,*,#24844,.F.);
#35331=ORIENTED_EDGE('',*,*,#25881,.T.);
#35332=ORIENTED_EDGE('',*,*,#23726,.T.);
#35333=ORIENTED_EDGE('',*,*,#25880,.F.);
#35334=ORIENTED_EDGE('',*,*,#24843,.F.);
#35335=ORIENTED_EDGE('',*,*,#25882,.T.);
#35336=ORIENTED_EDGE('',*,*,#23727,.T.);
#35337=ORIENTED_EDGE('',*,*,#25881,.F.);
#35338=ORIENTED_EDGE('',*,*,#24842,.F.);
#35339=ORIENTED_EDGE('',*,*,#25878,.T.);
#35340=ORIENTED_EDGE('',*,*,#23728,.T.);
#35341=ORIENTED_EDGE('',*,*,#25882,.F.);
#35342=ORIENTED_EDGE('',*,*,#24841,.F.);
#35343=ORIENTED_EDGE('',*,*,#25883,.T.);
#35344=ORIENTED_EDGE('',*,*,#23717,.T.);
#35345=ORIENTED_EDGE('',*,*,#25884,.F.);
#35346=ORIENTED_EDGE('',*,*,#24834,.F.);
#35347=ORIENTED_EDGE('',*,*,#25885,.T.);
#35348=ORIENTED_EDGE('',*,*,#23718,.T.);
#35349=ORIENTED_EDGE('',*,*,#25883,.F.);
#35350=ORIENTED_EDGE('',*,*,#24833,.F.);
#35351=ORIENTED_EDGE('',*,*,#25886,.T.);
#35352=ORIENTED_EDGE('',*,*,#23719,.T.);
#35353=ORIENTED_EDGE('',*,*,#25885,.F.);
#35354=ORIENTED_EDGE('',*,*,#24838,.F.);
#35355=ORIENTED_EDGE('',*,*,#25887,.T.);
#35356=ORIENTED_EDGE('',*,*,#23720,.T.);
#35357=ORIENTED_EDGE('',*,*,#25886,.F.);
#35358=ORIENTED_EDGE('',*,*,#24837,.F.);
#35359=ORIENTED_EDGE('',*,*,#25888,.T.);
#35360=ORIENTED_EDGE('',*,*,#23721,.T.);
#35361=ORIENTED_EDGE('',*,*,#25887,.F.);
#35362=ORIENTED_EDGE('',*,*,#24836,.F.);
#35363=ORIENTED_EDGE('',*,*,#25884,.T.);
#35364=ORIENTED_EDGE('',*,*,#23722,.T.);
#35365=ORIENTED_EDGE('',*,*,#25888,.F.);
#35366=ORIENTED_EDGE('',*,*,#24835,.F.);
#35367=ORIENTED_EDGE('',*,*,#25889,.T.);
#35368=ORIENTED_EDGE('',*,*,#23711,.T.);
#35369=ORIENTED_EDGE('',*,*,#25890,.F.);
#35370=ORIENTED_EDGE('',*,*,#24828,.F.);
#35371=ORIENTED_EDGE('',*,*,#25891,.T.);
#35372=ORIENTED_EDGE('',*,*,#23712,.T.);
#35373=ORIENTED_EDGE('',*,*,#25889,.F.);
#35374=ORIENTED_EDGE('',*,*,#24827,.F.);
#35375=ORIENTED_EDGE('',*,*,#25892,.T.);
#35376=ORIENTED_EDGE('',*,*,#23713,.T.);
#35377=ORIENTED_EDGE('',*,*,#25891,.F.);
#35378=ORIENTED_EDGE('',*,*,#24832,.F.);
#35379=ORIENTED_EDGE('',*,*,#25893,.T.);
#35380=ORIENTED_EDGE('',*,*,#23714,.T.);
#35381=ORIENTED_EDGE('',*,*,#25892,.F.);
#35382=ORIENTED_EDGE('',*,*,#24831,.F.);
#35383=ORIENTED_EDGE('',*,*,#25894,.T.);
#35384=ORIENTED_EDGE('',*,*,#23715,.T.);
#35385=ORIENTED_EDGE('',*,*,#25893,.F.);
#35386=ORIENTED_EDGE('',*,*,#24830,.F.);
#35387=ORIENTED_EDGE('',*,*,#25890,.T.);
#35388=ORIENTED_EDGE('',*,*,#23716,.T.);
#35389=ORIENTED_EDGE('',*,*,#25894,.F.);
#35390=ORIENTED_EDGE('',*,*,#24829,.F.);
#35391=ORIENTED_EDGE('',*,*,#25895,.T.);
#35392=ORIENTED_EDGE('',*,*,#23705,.T.);
#35393=ORIENTED_EDGE('',*,*,#25896,.F.);
#35394=ORIENTED_EDGE('',*,*,#24822,.F.);
#35395=ORIENTED_EDGE('',*,*,#25897,.T.);
#35396=ORIENTED_EDGE('',*,*,#23706,.T.);
#35397=ORIENTED_EDGE('',*,*,#25895,.F.);
#35398=ORIENTED_EDGE('',*,*,#24821,.F.);
#35399=ORIENTED_EDGE('',*,*,#25898,.T.);
#35400=ORIENTED_EDGE('',*,*,#23707,.T.);
#35401=ORIENTED_EDGE('',*,*,#25897,.F.);
#35402=ORIENTED_EDGE('',*,*,#24826,.F.);
#35403=ORIENTED_EDGE('',*,*,#25899,.T.);
#35404=ORIENTED_EDGE('',*,*,#23708,.T.);
#35405=ORIENTED_EDGE('',*,*,#25898,.F.);
#35406=ORIENTED_EDGE('',*,*,#24825,.F.);
#35407=ORIENTED_EDGE('',*,*,#25900,.T.);
#35408=ORIENTED_EDGE('',*,*,#23709,.T.);
#35409=ORIENTED_EDGE('',*,*,#25899,.F.);
#35410=ORIENTED_EDGE('',*,*,#24824,.F.);
#35411=ORIENTED_EDGE('',*,*,#25896,.T.);
#35412=ORIENTED_EDGE('',*,*,#23710,.T.);
#35413=ORIENTED_EDGE('',*,*,#25900,.F.);
#35414=ORIENTED_EDGE('',*,*,#24823,.F.);
#35415=ORIENTED_EDGE('',*,*,#25901,.T.);
#35416=ORIENTED_EDGE('',*,*,#23699,.T.);
#35417=ORIENTED_EDGE('',*,*,#25902,.F.);
#35418=ORIENTED_EDGE('',*,*,#24816,.F.);
#35419=ORIENTED_EDGE('',*,*,#25903,.T.);
#35420=ORIENTED_EDGE('',*,*,#23700,.T.);
#35421=ORIENTED_EDGE('',*,*,#25901,.F.);
#35422=ORIENTED_EDGE('',*,*,#24815,.F.);
#35423=ORIENTED_EDGE('',*,*,#25904,.T.);
#35424=ORIENTED_EDGE('',*,*,#23701,.T.);
#35425=ORIENTED_EDGE('',*,*,#25903,.F.);
#35426=ORIENTED_EDGE('',*,*,#24820,.F.);
#35427=ORIENTED_EDGE('',*,*,#25905,.T.);
#35428=ORIENTED_EDGE('',*,*,#23702,.T.);
#35429=ORIENTED_EDGE('',*,*,#25904,.F.);
#35430=ORIENTED_EDGE('',*,*,#24819,.F.);
#35431=ORIENTED_EDGE('',*,*,#25906,.T.);
#35432=ORIENTED_EDGE('',*,*,#23703,.T.);
#35433=ORIENTED_EDGE('',*,*,#25905,.F.);
#35434=ORIENTED_EDGE('',*,*,#24818,.F.);
#35435=ORIENTED_EDGE('',*,*,#25902,.T.);
#35436=ORIENTED_EDGE('',*,*,#23704,.T.);
#35437=ORIENTED_EDGE('',*,*,#25906,.F.);
#35438=ORIENTED_EDGE('',*,*,#24817,.F.);
#35439=ORIENTED_EDGE('',*,*,#25907,.T.);
#35440=ORIENTED_EDGE('',*,*,#23693,.T.);
#35441=ORIENTED_EDGE('',*,*,#25908,.F.);
#35442=ORIENTED_EDGE('',*,*,#24810,.F.);
#35443=ORIENTED_EDGE('',*,*,#25909,.T.);
#35444=ORIENTED_EDGE('',*,*,#23694,.T.);
#35445=ORIENTED_EDGE('',*,*,#25907,.F.);
#35446=ORIENTED_EDGE('',*,*,#24809,.F.);
#35447=ORIENTED_EDGE('',*,*,#25910,.T.);
#35448=ORIENTED_EDGE('',*,*,#23695,.T.);
#35449=ORIENTED_EDGE('',*,*,#25909,.F.);
#35450=ORIENTED_EDGE('',*,*,#24814,.F.);
#35451=ORIENTED_EDGE('',*,*,#25911,.T.);
#35452=ORIENTED_EDGE('',*,*,#23696,.T.);
#35453=ORIENTED_EDGE('',*,*,#25910,.F.);
#35454=ORIENTED_EDGE('',*,*,#24813,.F.);
#35455=ORIENTED_EDGE('',*,*,#25912,.T.);
#35456=ORIENTED_EDGE('',*,*,#23697,.T.);
#35457=ORIENTED_EDGE('',*,*,#25911,.F.);
#35458=ORIENTED_EDGE('',*,*,#24812,.F.);
#35459=ORIENTED_EDGE('',*,*,#25908,.T.);
#35460=ORIENTED_EDGE('',*,*,#23698,.T.);
#35461=ORIENTED_EDGE('',*,*,#25912,.F.);
#35462=ORIENTED_EDGE('',*,*,#24811,.F.);
#35463=ORIENTED_EDGE('',*,*,#25913,.T.);
#35464=ORIENTED_EDGE('',*,*,#23687,.T.);
#35465=ORIENTED_EDGE('',*,*,#25914,.F.);
#35466=ORIENTED_EDGE('',*,*,#24804,.F.);
#35467=ORIENTED_EDGE('',*,*,#25915,.T.);
#35468=ORIENTED_EDGE('',*,*,#23688,.T.);
#35469=ORIENTED_EDGE('',*,*,#25913,.F.);
#35470=ORIENTED_EDGE('',*,*,#24803,.F.);
#35471=ORIENTED_EDGE('',*,*,#25916,.T.);
#35472=ORIENTED_EDGE('',*,*,#23689,.T.);
#35473=ORIENTED_EDGE('',*,*,#25915,.F.);
#35474=ORIENTED_EDGE('',*,*,#24808,.F.);
#35475=ORIENTED_EDGE('',*,*,#25917,.T.);
#35476=ORIENTED_EDGE('',*,*,#23690,.T.);
#35477=ORIENTED_EDGE('',*,*,#25916,.F.);
#35478=ORIENTED_EDGE('',*,*,#24807,.F.);
#35479=ORIENTED_EDGE('',*,*,#25918,.T.);
#35480=ORIENTED_EDGE('',*,*,#23691,.T.);
#35481=ORIENTED_EDGE('',*,*,#25917,.F.);
#35482=ORIENTED_EDGE('',*,*,#24806,.F.);
#35483=ORIENTED_EDGE('',*,*,#25914,.T.);
#35484=ORIENTED_EDGE('',*,*,#23692,.T.);
#35485=ORIENTED_EDGE('',*,*,#25918,.F.);
#35486=ORIENTED_EDGE('',*,*,#24805,.F.);
#35487=ORIENTED_EDGE('',*,*,#25919,.T.);
#35488=ORIENTED_EDGE('',*,*,#23681,.T.);
#35489=ORIENTED_EDGE('',*,*,#25920,.F.);
#35490=ORIENTED_EDGE('',*,*,#24798,.F.);
#35491=ORIENTED_EDGE('',*,*,#25921,.T.);
#35492=ORIENTED_EDGE('',*,*,#23682,.T.);
#35493=ORIENTED_EDGE('',*,*,#25919,.F.);
#35494=ORIENTED_EDGE('',*,*,#24797,.F.);
#35495=ORIENTED_EDGE('',*,*,#25922,.T.);
#35496=ORIENTED_EDGE('',*,*,#23683,.T.);
#35497=ORIENTED_EDGE('',*,*,#25921,.F.);
#35498=ORIENTED_EDGE('',*,*,#24802,.F.);
#35499=ORIENTED_EDGE('',*,*,#25923,.T.);
#35500=ORIENTED_EDGE('',*,*,#23684,.T.);
#35501=ORIENTED_EDGE('',*,*,#25922,.F.);
#35502=ORIENTED_EDGE('',*,*,#24801,.F.);
#35503=ORIENTED_EDGE('',*,*,#25924,.T.);
#35504=ORIENTED_EDGE('',*,*,#23685,.T.);
#35505=ORIENTED_EDGE('',*,*,#25923,.F.);
#35506=ORIENTED_EDGE('',*,*,#24800,.F.);
#35507=ORIENTED_EDGE('',*,*,#25920,.T.);
#35508=ORIENTED_EDGE('',*,*,#23686,.T.);
#35509=ORIENTED_EDGE('',*,*,#25924,.F.);
#35510=ORIENTED_EDGE('',*,*,#24799,.F.);
#35511=ORIENTED_EDGE('',*,*,#25925,.T.);
#35512=ORIENTED_EDGE('',*,*,#23675,.T.);
#35513=ORIENTED_EDGE('',*,*,#25926,.F.);
#35514=ORIENTED_EDGE('',*,*,#24792,.F.);
#35515=ORIENTED_EDGE('',*,*,#25927,.T.);
#35516=ORIENTED_EDGE('',*,*,#23676,.T.);
#35517=ORIENTED_EDGE('',*,*,#25925,.F.);
#35518=ORIENTED_EDGE('',*,*,#24791,.F.);
#35519=ORIENTED_EDGE('',*,*,#25928,.T.);
#35520=ORIENTED_EDGE('',*,*,#23677,.T.);
#35521=ORIENTED_EDGE('',*,*,#25927,.F.);
#35522=ORIENTED_EDGE('',*,*,#24796,.F.);
#35523=ORIENTED_EDGE('',*,*,#25929,.T.);
#35524=ORIENTED_EDGE('',*,*,#23678,.T.);
#35525=ORIENTED_EDGE('',*,*,#25928,.F.);
#35526=ORIENTED_EDGE('',*,*,#24795,.F.);
#35527=ORIENTED_EDGE('',*,*,#25930,.T.);
#35528=ORIENTED_EDGE('',*,*,#23679,.T.);
#35529=ORIENTED_EDGE('',*,*,#25929,.F.);
#35530=ORIENTED_EDGE('',*,*,#24794,.F.);
#35531=ORIENTED_EDGE('',*,*,#25926,.T.);
#35532=ORIENTED_EDGE('',*,*,#23680,.T.);
#35533=ORIENTED_EDGE('',*,*,#25930,.F.);
#35534=ORIENTED_EDGE('',*,*,#24793,.F.);
#35535=ORIENTED_EDGE('',*,*,#25931,.T.);
#35536=ORIENTED_EDGE('',*,*,#23669,.T.);
#35537=ORIENTED_EDGE('',*,*,#25932,.F.);
#35538=ORIENTED_EDGE('',*,*,#24786,.F.);
#35539=ORIENTED_EDGE('',*,*,#25933,.T.);
#35540=ORIENTED_EDGE('',*,*,#23670,.T.);
#35541=ORIENTED_EDGE('',*,*,#25931,.F.);
#35542=ORIENTED_EDGE('',*,*,#24785,.F.);
#35543=ORIENTED_EDGE('',*,*,#25934,.T.);
#35544=ORIENTED_EDGE('',*,*,#23671,.T.);
#35545=ORIENTED_EDGE('',*,*,#25933,.F.);
#35546=ORIENTED_EDGE('',*,*,#24790,.F.);
#35547=ORIENTED_EDGE('',*,*,#25935,.T.);
#35548=ORIENTED_EDGE('',*,*,#23672,.T.);
#35549=ORIENTED_EDGE('',*,*,#25934,.F.);
#35550=ORIENTED_EDGE('',*,*,#24789,.F.);
#35551=ORIENTED_EDGE('',*,*,#25936,.T.);
#35552=ORIENTED_EDGE('',*,*,#23673,.T.);
#35553=ORIENTED_EDGE('',*,*,#25935,.F.);
#35554=ORIENTED_EDGE('',*,*,#24788,.F.);
#35555=ORIENTED_EDGE('',*,*,#25932,.T.);
#35556=ORIENTED_EDGE('',*,*,#23674,.T.);
#35557=ORIENTED_EDGE('',*,*,#25936,.F.);
#35558=ORIENTED_EDGE('',*,*,#24787,.F.);
#35559=ORIENTED_EDGE('',*,*,#25937,.T.);
#35560=ORIENTED_EDGE('',*,*,#23663,.T.);
#35561=ORIENTED_EDGE('',*,*,#25938,.F.);
#35562=ORIENTED_EDGE('',*,*,#24780,.F.);
#35563=ORIENTED_EDGE('',*,*,#25939,.T.);
#35564=ORIENTED_EDGE('',*,*,#23664,.T.);
#35565=ORIENTED_EDGE('',*,*,#25937,.F.);
#35566=ORIENTED_EDGE('',*,*,#24779,.F.);
#35567=ORIENTED_EDGE('',*,*,#25940,.T.);
#35568=ORIENTED_EDGE('',*,*,#23665,.T.);
#35569=ORIENTED_EDGE('',*,*,#25939,.F.);
#35570=ORIENTED_EDGE('',*,*,#24784,.F.);
#35571=ORIENTED_EDGE('',*,*,#25941,.T.);
#35572=ORIENTED_EDGE('',*,*,#23666,.T.);
#35573=ORIENTED_EDGE('',*,*,#25940,.F.);
#35574=ORIENTED_EDGE('',*,*,#24783,.F.);
#35575=ORIENTED_EDGE('',*,*,#25942,.T.);
#35576=ORIENTED_EDGE('',*,*,#23667,.T.);
#35577=ORIENTED_EDGE('',*,*,#25941,.F.);
#35578=ORIENTED_EDGE('',*,*,#24782,.F.);
#35579=ORIENTED_EDGE('',*,*,#25938,.T.);
#35580=ORIENTED_EDGE('',*,*,#23668,.T.);
#35581=ORIENTED_EDGE('',*,*,#25942,.F.);
#35582=ORIENTED_EDGE('',*,*,#24781,.F.);
#35583=ORIENTED_EDGE('',*,*,#25943,.T.);
#35584=ORIENTED_EDGE('',*,*,#23657,.T.);
#35585=ORIENTED_EDGE('',*,*,#25944,.F.);
#35586=ORIENTED_EDGE('',*,*,#24774,.F.);
#35587=ORIENTED_EDGE('',*,*,#25945,.T.);
#35588=ORIENTED_EDGE('',*,*,#23658,.T.);
#35589=ORIENTED_EDGE('',*,*,#25943,.F.);
#35590=ORIENTED_EDGE('',*,*,#24773,.F.);
#35591=ORIENTED_EDGE('',*,*,#25946,.T.);
#35592=ORIENTED_EDGE('',*,*,#23659,.T.);
#35593=ORIENTED_EDGE('',*,*,#25945,.F.);
#35594=ORIENTED_EDGE('',*,*,#24778,.F.);
#35595=ORIENTED_EDGE('',*,*,#25947,.T.);
#35596=ORIENTED_EDGE('',*,*,#23660,.T.);
#35597=ORIENTED_EDGE('',*,*,#25946,.F.);
#35598=ORIENTED_EDGE('',*,*,#24777,.F.);
#35599=ORIENTED_EDGE('',*,*,#25948,.T.);
#35600=ORIENTED_EDGE('',*,*,#23661,.T.);
#35601=ORIENTED_EDGE('',*,*,#25947,.F.);
#35602=ORIENTED_EDGE('',*,*,#24776,.F.);
#35603=ORIENTED_EDGE('',*,*,#25944,.T.);
#35604=ORIENTED_EDGE('',*,*,#23662,.T.);
#35605=ORIENTED_EDGE('',*,*,#25948,.F.);
#35606=ORIENTED_EDGE('',*,*,#24775,.F.);
#35607=ORIENTED_EDGE('',*,*,#25949,.T.);
#35608=ORIENTED_EDGE('',*,*,#23651,.T.);
#35609=ORIENTED_EDGE('',*,*,#25950,.F.);
#35610=ORIENTED_EDGE('',*,*,#24768,.F.);
#35611=ORIENTED_EDGE('',*,*,#25951,.T.);
#35612=ORIENTED_EDGE('',*,*,#23652,.T.);
#35613=ORIENTED_EDGE('',*,*,#25949,.F.);
#35614=ORIENTED_EDGE('',*,*,#24767,.F.);
#35615=ORIENTED_EDGE('',*,*,#25952,.T.);
#35616=ORIENTED_EDGE('',*,*,#23653,.T.);
#35617=ORIENTED_EDGE('',*,*,#25951,.F.);
#35618=ORIENTED_EDGE('',*,*,#24772,.F.);
#35619=ORIENTED_EDGE('',*,*,#25953,.T.);
#35620=ORIENTED_EDGE('',*,*,#23654,.T.);
#35621=ORIENTED_EDGE('',*,*,#25952,.F.);
#35622=ORIENTED_EDGE('',*,*,#24771,.F.);
#35623=ORIENTED_EDGE('',*,*,#25954,.T.);
#35624=ORIENTED_EDGE('',*,*,#23655,.T.);
#35625=ORIENTED_EDGE('',*,*,#25953,.F.);
#35626=ORIENTED_EDGE('',*,*,#24770,.F.);
#35627=ORIENTED_EDGE('',*,*,#25950,.T.);
#35628=ORIENTED_EDGE('',*,*,#23656,.T.);
#35629=ORIENTED_EDGE('',*,*,#25954,.F.);
#35630=ORIENTED_EDGE('',*,*,#24769,.F.);
#35631=ORIENTED_EDGE('',*,*,#25955,.T.);
#35632=ORIENTED_EDGE('',*,*,#23645,.T.);
#35633=ORIENTED_EDGE('',*,*,#25956,.F.);
#35634=ORIENTED_EDGE('',*,*,#24762,.F.);
#35635=ORIENTED_EDGE('',*,*,#25957,.T.);
#35636=ORIENTED_EDGE('',*,*,#23646,.T.);
#35637=ORIENTED_EDGE('',*,*,#25955,.F.);
#35638=ORIENTED_EDGE('',*,*,#24761,.F.);
#35639=ORIENTED_EDGE('',*,*,#25958,.T.);
#35640=ORIENTED_EDGE('',*,*,#23647,.T.);
#35641=ORIENTED_EDGE('',*,*,#25957,.F.);
#35642=ORIENTED_EDGE('',*,*,#24766,.F.);
#35643=ORIENTED_EDGE('',*,*,#25959,.T.);
#35644=ORIENTED_EDGE('',*,*,#23648,.T.);
#35645=ORIENTED_EDGE('',*,*,#25958,.F.);
#35646=ORIENTED_EDGE('',*,*,#24765,.F.);
#35647=ORIENTED_EDGE('',*,*,#25960,.T.);
#35648=ORIENTED_EDGE('',*,*,#23649,.T.);
#35649=ORIENTED_EDGE('',*,*,#25959,.F.);
#35650=ORIENTED_EDGE('',*,*,#24764,.F.);
#35651=ORIENTED_EDGE('',*,*,#25956,.T.);
#35652=ORIENTED_EDGE('',*,*,#23650,.T.);
#35653=ORIENTED_EDGE('',*,*,#25960,.F.);
#35654=ORIENTED_EDGE('',*,*,#24763,.F.);
#35655=ORIENTED_EDGE('',*,*,#25961,.T.);
#35656=ORIENTED_EDGE('',*,*,#23639,.T.);
#35657=ORIENTED_EDGE('',*,*,#25962,.F.);
#35658=ORIENTED_EDGE('',*,*,#24756,.F.);
#35659=ORIENTED_EDGE('',*,*,#25963,.T.);
#35660=ORIENTED_EDGE('',*,*,#23640,.T.);
#35661=ORIENTED_EDGE('',*,*,#25961,.F.);
#35662=ORIENTED_EDGE('',*,*,#24755,.F.);
#35663=ORIENTED_EDGE('',*,*,#25964,.T.);
#35664=ORIENTED_EDGE('',*,*,#23641,.T.);
#35665=ORIENTED_EDGE('',*,*,#25963,.F.);
#35666=ORIENTED_EDGE('',*,*,#24760,.F.);
#35667=ORIENTED_EDGE('',*,*,#25965,.T.);
#35668=ORIENTED_EDGE('',*,*,#23642,.T.);
#35669=ORIENTED_EDGE('',*,*,#25964,.F.);
#35670=ORIENTED_EDGE('',*,*,#24759,.F.);
#35671=ORIENTED_EDGE('',*,*,#25966,.T.);
#35672=ORIENTED_EDGE('',*,*,#23643,.T.);
#35673=ORIENTED_EDGE('',*,*,#25965,.F.);
#35674=ORIENTED_EDGE('',*,*,#24758,.F.);
#35675=ORIENTED_EDGE('',*,*,#25962,.T.);
#35676=ORIENTED_EDGE('',*,*,#23644,.T.);
#35677=ORIENTED_EDGE('',*,*,#25966,.F.);
#35678=ORIENTED_EDGE('',*,*,#24757,.F.);
#35679=ORIENTED_EDGE('',*,*,#25967,.T.);
#35680=ORIENTED_EDGE('',*,*,#23633,.T.);
#35681=ORIENTED_EDGE('',*,*,#25968,.F.);
#35682=ORIENTED_EDGE('',*,*,#24750,.F.);
#35683=ORIENTED_EDGE('',*,*,#25969,.T.);
#35684=ORIENTED_EDGE('',*,*,#23634,.T.);
#35685=ORIENTED_EDGE('',*,*,#25967,.F.);
#35686=ORIENTED_EDGE('',*,*,#24749,.F.);
#35687=ORIENTED_EDGE('',*,*,#25970,.T.);
#35688=ORIENTED_EDGE('',*,*,#23635,.T.);
#35689=ORIENTED_EDGE('',*,*,#25969,.F.);
#35690=ORIENTED_EDGE('',*,*,#24754,.F.);
#35691=ORIENTED_EDGE('',*,*,#25971,.T.);
#35692=ORIENTED_EDGE('',*,*,#23636,.T.);
#35693=ORIENTED_EDGE('',*,*,#25970,.F.);
#35694=ORIENTED_EDGE('',*,*,#24753,.F.);
#35695=ORIENTED_EDGE('',*,*,#25972,.T.);
#35696=ORIENTED_EDGE('',*,*,#23637,.T.);
#35697=ORIENTED_EDGE('',*,*,#25971,.F.);
#35698=ORIENTED_EDGE('',*,*,#24752,.F.);
#35699=ORIENTED_EDGE('',*,*,#25968,.T.);
#35700=ORIENTED_EDGE('',*,*,#23638,.T.);
#35701=ORIENTED_EDGE('',*,*,#25972,.F.);
#35702=ORIENTED_EDGE('',*,*,#24751,.F.);
#35703=ORIENTED_EDGE('',*,*,#25973,.T.);
#35704=ORIENTED_EDGE('',*,*,#23627,.T.);
#35705=ORIENTED_EDGE('',*,*,#25974,.F.);
#35706=ORIENTED_EDGE('',*,*,#24744,.F.);
#35707=ORIENTED_EDGE('',*,*,#25975,.T.);
#35708=ORIENTED_EDGE('',*,*,#23628,.T.);
#35709=ORIENTED_EDGE('',*,*,#25973,.F.);
#35710=ORIENTED_EDGE('',*,*,#24743,.F.);
#35711=ORIENTED_EDGE('',*,*,#25976,.T.);
#35712=ORIENTED_EDGE('',*,*,#23629,.T.);
#35713=ORIENTED_EDGE('',*,*,#25975,.F.);
#35714=ORIENTED_EDGE('',*,*,#24748,.F.);
#35715=ORIENTED_EDGE('',*,*,#25977,.T.);
#35716=ORIENTED_EDGE('',*,*,#23630,.T.);
#35717=ORIENTED_EDGE('',*,*,#25976,.F.);
#35718=ORIENTED_EDGE('',*,*,#24747,.F.);
#35719=ORIENTED_EDGE('',*,*,#25978,.T.);
#35720=ORIENTED_EDGE('',*,*,#23631,.T.);
#35721=ORIENTED_EDGE('',*,*,#25977,.F.);
#35722=ORIENTED_EDGE('',*,*,#24746,.F.);
#35723=ORIENTED_EDGE('',*,*,#25974,.T.);
#35724=ORIENTED_EDGE('',*,*,#23632,.T.);
#35725=ORIENTED_EDGE('',*,*,#25978,.F.);
#35726=ORIENTED_EDGE('',*,*,#24745,.F.);
#35727=ORIENTED_EDGE('',*,*,#25979,.T.);
#35728=ORIENTED_EDGE('',*,*,#23621,.T.);
#35729=ORIENTED_EDGE('',*,*,#25980,.F.);
#35730=ORIENTED_EDGE('',*,*,#24738,.F.);
#35731=ORIENTED_EDGE('',*,*,#25981,.T.);
#35732=ORIENTED_EDGE('',*,*,#23622,.T.);
#35733=ORIENTED_EDGE('',*,*,#25979,.F.);
#35734=ORIENTED_EDGE('',*,*,#24737,.F.);
#35735=ORIENTED_EDGE('',*,*,#25982,.T.);
#35736=ORIENTED_EDGE('',*,*,#23623,.T.);
#35737=ORIENTED_EDGE('',*,*,#25981,.F.);
#35738=ORIENTED_EDGE('',*,*,#24742,.F.);
#35739=ORIENTED_EDGE('',*,*,#25983,.T.);
#35740=ORIENTED_EDGE('',*,*,#23624,.T.);
#35741=ORIENTED_EDGE('',*,*,#25982,.F.);
#35742=ORIENTED_EDGE('',*,*,#24741,.F.);
#35743=ORIENTED_EDGE('',*,*,#25984,.T.);
#35744=ORIENTED_EDGE('',*,*,#23625,.T.);
#35745=ORIENTED_EDGE('',*,*,#25983,.F.);
#35746=ORIENTED_EDGE('',*,*,#24740,.F.);
#35747=ORIENTED_EDGE('',*,*,#25980,.T.);
#35748=ORIENTED_EDGE('',*,*,#23626,.T.);
#35749=ORIENTED_EDGE('',*,*,#25984,.F.);
#35750=ORIENTED_EDGE('',*,*,#24739,.F.);
#35751=ORIENTED_EDGE('',*,*,#25985,.T.);
#35752=ORIENTED_EDGE('',*,*,#23615,.T.);
#35753=ORIENTED_EDGE('',*,*,#25986,.F.);
#35754=ORIENTED_EDGE('',*,*,#24732,.F.);
#35755=ORIENTED_EDGE('',*,*,#25987,.T.);
#35756=ORIENTED_EDGE('',*,*,#23616,.T.);
#35757=ORIENTED_EDGE('',*,*,#25985,.F.);
#35758=ORIENTED_EDGE('',*,*,#24731,.F.);
#35759=ORIENTED_EDGE('',*,*,#25988,.T.);
#35760=ORIENTED_EDGE('',*,*,#23617,.T.);
#35761=ORIENTED_EDGE('',*,*,#25987,.F.);
#35762=ORIENTED_EDGE('',*,*,#24736,.F.);
#35763=ORIENTED_EDGE('',*,*,#25989,.T.);
#35764=ORIENTED_EDGE('',*,*,#23618,.T.);
#35765=ORIENTED_EDGE('',*,*,#25988,.F.);
#35766=ORIENTED_EDGE('',*,*,#24735,.F.);
#35767=ORIENTED_EDGE('',*,*,#25990,.T.);
#35768=ORIENTED_EDGE('',*,*,#23619,.T.);
#35769=ORIENTED_EDGE('',*,*,#25989,.F.);
#35770=ORIENTED_EDGE('',*,*,#24734,.F.);
#35771=ORIENTED_EDGE('',*,*,#25986,.T.);
#35772=ORIENTED_EDGE('',*,*,#23620,.T.);
#35773=ORIENTED_EDGE('',*,*,#25990,.F.);
#35774=ORIENTED_EDGE('',*,*,#24733,.F.);
#35775=ORIENTED_EDGE('',*,*,#25991,.T.);
#35776=ORIENTED_EDGE('',*,*,#23609,.T.);
#35777=ORIENTED_EDGE('',*,*,#25992,.F.);
#35778=ORIENTED_EDGE('',*,*,#24726,.F.);
#35779=ORIENTED_EDGE('',*,*,#25993,.T.);
#35780=ORIENTED_EDGE('',*,*,#23610,.T.);
#35781=ORIENTED_EDGE('',*,*,#25991,.F.);
#35782=ORIENTED_EDGE('',*,*,#24725,.F.);
#35783=ORIENTED_EDGE('',*,*,#25994,.T.);
#35784=ORIENTED_EDGE('',*,*,#23611,.T.);
#35785=ORIENTED_EDGE('',*,*,#25993,.F.);
#35786=ORIENTED_EDGE('',*,*,#24730,.F.);
#35787=ORIENTED_EDGE('',*,*,#25995,.T.);
#35788=ORIENTED_EDGE('',*,*,#23612,.T.);
#35789=ORIENTED_EDGE('',*,*,#25994,.F.);
#35790=ORIENTED_EDGE('',*,*,#24729,.F.);
#35791=ORIENTED_EDGE('',*,*,#25996,.T.);
#35792=ORIENTED_EDGE('',*,*,#23613,.T.);
#35793=ORIENTED_EDGE('',*,*,#25995,.F.);
#35794=ORIENTED_EDGE('',*,*,#24728,.F.);
#35795=ORIENTED_EDGE('',*,*,#25992,.T.);
#35796=ORIENTED_EDGE('',*,*,#23614,.T.);
#35797=ORIENTED_EDGE('',*,*,#25996,.F.);
#35798=ORIENTED_EDGE('',*,*,#24727,.F.);
#35799=ORIENTED_EDGE('',*,*,#25997,.T.);
#35800=ORIENTED_EDGE('',*,*,#23603,.T.);
#35801=ORIENTED_EDGE('',*,*,#25998,.F.);
#35802=ORIENTED_EDGE('',*,*,#24720,.F.);
#35803=ORIENTED_EDGE('',*,*,#25999,.T.);
#35804=ORIENTED_EDGE('',*,*,#23604,.T.);
#35805=ORIENTED_EDGE('',*,*,#25997,.F.);
#35806=ORIENTED_EDGE('',*,*,#24719,.F.);
#35807=ORIENTED_EDGE('',*,*,#26000,.T.);
#35808=ORIENTED_EDGE('',*,*,#23605,.T.);
#35809=ORIENTED_EDGE('',*,*,#25999,.F.);
#35810=ORIENTED_EDGE('',*,*,#24724,.F.);
#35811=ORIENTED_EDGE('',*,*,#26001,.T.);
#35812=ORIENTED_EDGE('',*,*,#23606,.T.);
#35813=ORIENTED_EDGE('',*,*,#26000,.F.);
#35814=ORIENTED_EDGE('',*,*,#24723,.F.);
#35815=ORIENTED_EDGE('',*,*,#26002,.T.);
#35816=ORIENTED_EDGE('',*,*,#23607,.T.);
#35817=ORIENTED_EDGE('',*,*,#26001,.F.);
#35818=ORIENTED_EDGE('',*,*,#24722,.F.);
#35819=ORIENTED_EDGE('',*,*,#25998,.T.);
#35820=ORIENTED_EDGE('',*,*,#23608,.T.);
#35821=ORIENTED_EDGE('',*,*,#26002,.F.);
#35822=ORIENTED_EDGE('',*,*,#24721,.F.);
#35823=ORIENTED_EDGE('',*,*,#26003,.T.);
#35824=ORIENTED_EDGE('',*,*,#23597,.T.);
#35825=ORIENTED_EDGE('',*,*,#26004,.F.);
#35826=ORIENTED_EDGE('',*,*,#24714,.F.);
#35827=ORIENTED_EDGE('',*,*,#26005,.T.);
#35828=ORIENTED_EDGE('',*,*,#23598,.T.);
#35829=ORIENTED_EDGE('',*,*,#26003,.F.);
#35830=ORIENTED_EDGE('',*,*,#24713,.F.);
#35831=ORIENTED_EDGE('',*,*,#26006,.T.);
#35832=ORIENTED_EDGE('',*,*,#23599,.T.);
#35833=ORIENTED_EDGE('',*,*,#26005,.F.);
#35834=ORIENTED_EDGE('',*,*,#24718,.F.);
#35835=ORIENTED_EDGE('',*,*,#26007,.T.);
#35836=ORIENTED_EDGE('',*,*,#23600,.T.);
#35837=ORIENTED_EDGE('',*,*,#26006,.F.);
#35838=ORIENTED_EDGE('',*,*,#24717,.F.);
#35839=ORIENTED_EDGE('',*,*,#26008,.T.);
#35840=ORIENTED_EDGE('',*,*,#23601,.T.);
#35841=ORIENTED_EDGE('',*,*,#26007,.F.);
#35842=ORIENTED_EDGE('',*,*,#24716,.F.);
#35843=ORIENTED_EDGE('',*,*,#26004,.T.);
#35844=ORIENTED_EDGE('',*,*,#23602,.T.);
#35845=ORIENTED_EDGE('',*,*,#26008,.F.);
#35846=ORIENTED_EDGE('',*,*,#24715,.F.);
#35847=ORIENTED_EDGE('',*,*,#26009,.T.);
#35848=ORIENTED_EDGE('',*,*,#23591,.T.);
#35849=ORIENTED_EDGE('',*,*,#26010,.F.);
#35850=ORIENTED_EDGE('',*,*,#24708,.F.);
#35851=ORIENTED_EDGE('',*,*,#26011,.T.);
#35852=ORIENTED_EDGE('',*,*,#23592,.T.);
#35853=ORIENTED_EDGE('',*,*,#26009,.F.);
#35854=ORIENTED_EDGE('',*,*,#24707,.F.);
#35855=ORIENTED_EDGE('',*,*,#26012,.T.);
#35856=ORIENTED_EDGE('',*,*,#23593,.T.);
#35857=ORIENTED_EDGE('',*,*,#26011,.F.);
#35858=ORIENTED_EDGE('',*,*,#24712,.F.);
#35859=ORIENTED_EDGE('',*,*,#26013,.T.);
#35860=ORIENTED_EDGE('',*,*,#23594,.T.);
#35861=ORIENTED_EDGE('',*,*,#26012,.F.);
#35862=ORIENTED_EDGE('',*,*,#24711,.F.);
#35863=ORIENTED_EDGE('',*,*,#26014,.T.);
#35864=ORIENTED_EDGE('',*,*,#23595,.T.);
#35865=ORIENTED_EDGE('',*,*,#26013,.F.);
#35866=ORIENTED_EDGE('',*,*,#24710,.F.);
#35867=ORIENTED_EDGE('',*,*,#26010,.T.);
#35868=ORIENTED_EDGE('',*,*,#23596,.T.);
#35869=ORIENTED_EDGE('',*,*,#26014,.F.);
#35870=ORIENTED_EDGE('',*,*,#24709,.F.);
#35871=ORIENTED_EDGE('',*,*,#26015,.T.);
#35872=ORIENTED_EDGE('',*,*,#23585,.T.);
#35873=ORIENTED_EDGE('',*,*,#26016,.F.);
#35874=ORIENTED_EDGE('',*,*,#24702,.F.);
#35875=ORIENTED_EDGE('',*,*,#26017,.T.);
#35876=ORIENTED_EDGE('',*,*,#23586,.T.);
#35877=ORIENTED_EDGE('',*,*,#26015,.F.);
#35878=ORIENTED_EDGE('',*,*,#24701,.F.);
#35879=ORIENTED_EDGE('',*,*,#26018,.T.);
#35880=ORIENTED_EDGE('',*,*,#23587,.T.);
#35881=ORIENTED_EDGE('',*,*,#26017,.F.);
#35882=ORIENTED_EDGE('',*,*,#24706,.F.);
#35883=ORIENTED_EDGE('',*,*,#26019,.T.);
#35884=ORIENTED_EDGE('',*,*,#23588,.T.);
#35885=ORIENTED_EDGE('',*,*,#26018,.F.);
#35886=ORIENTED_EDGE('',*,*,#24705,.F.);
#35887=ORIENTED_EDGE('',*,*,#26020,.T.);
#35888=ORIENTED_EDGE('',*,*,#23589,.T.);
#35889=ORIENTED_EDGE('',*,*,#26019,.F.);
#35890=ORIENTED_EDGE('',*,*,#24704,.F.);
#35891=ORIENTED_EDGE('',*,*,#26016,.T.);
#35892=ORIENTED_EDGE('',*,*,#23590,.T.);
#35893=ORIENTED_EDGE('',*,*,#26020,.F.);
#35894=ORIENTED_EDGE('',*,*,#24703,.F.);
#35895=ORIENTED_EDGE('',*,*,#26021,.T.);
#35896=ORIENTED_EDGE('',*,*,#23579,.T.);
#35897=ORIENTED_EDGE('',*,*,#26022,.F.);
#35898=ORIENTED_EDGE('',*,*,#24696,.F.);
#35899=ORIENTED_EDGE('',*,*,#26023,.T.);
#35900=ORIENTED_EDGE('',*,*,#23580,.T.);
#35901=ORIENTED_EDGE('',*,*,#26021,.F.);
#35902=ORIENTED_EDGE('',*,*,#24695,.F.);
#35903=ORIENTED_EDGE('',*,*,#26024,.T.);
#35904=ORIENTED_EDGE('',*,*,#23581,.T.);
#35905=ORIENTED_EDGE('',*,*,#26023,.F.);
#35906=ORIENTED_EDGE('',*,*,#24700,.F.);
#35907=ORIENTED_EDGE('',*,*,#26025,.T.);
#35908=ORIENTED_EDGE('',*,*,#23582,.T.);
#35909=ORIENTED_EDGE('',*,*,#26024,.F.);
#35910=ORIENTED_EDGE('',*,*,#24699,.F.);
#35911=ORIENTED_EDGE('',*,*,#26026,.T.);
#35912=ORIENTED_EDGE('',*,*,#23583,.T.);
#35913=ORIENTED_EDGE('',*,*,#26025,.F.);
#35914=ORIENTED_EDGE('',*,*,#24698,.F.);
#35915=ORIENTED_EDGE('',*,*,#26022,.T.);
#35916=ORIENTED_EDGE('',*,*,#23584,.T.);
#35917=ORIENTED_EDGE('',*,*,#26026,.F.);
#35918=ORIENTED_EDGE('',*,*,#24697,.F.);
#35919=ORIENTED_EDGE('',*,*,#26027,.T.);
#35920=ORIENTED_EDGE('',*,*,#23573,.T.);
#35921=ORIENTED_EDGE('',*,*,#26028,.F.);
#35922=ORIENTED_EDGE('',*,*,#24690,.F.);
#35923=ORIENTED_EDGE('',*,*,#26029,.T.);
#35924=ORIENTED_EDGE('',*,*,#23574,.T.);
#35925=ORIENTED_EDGE('',*,*,#26027,.F.);
#35926=ORIENTED_EDGE('',*,*,#24689,.F.);
#35927=ORIENTED_EDGE('',*,*,#26030,.T.);
#35928=ORIENTED_EDGE('',*,*,#23575,.T.);
#35929=ORIENTED_EDGE('',*,*,#26029,.F.);
#35930=ORIENTED_EDGE('',*,*,#24694,.F.);
#35931=ORIENTED_EDGE('',*,*,#26031,.T.);
#35932=ORIENTED_EDGE('',*,*,#23576,.T.);
#35933=ORIENTED_EDGE('',*,*,#26030,.F.);
#35934=ORIENTED_EDGE('',*,*,#24693,.F.);
#35935=ORIENTED_EDGE('',*,*,#26032,.T.);
#35936=ORIENTED_EDGE('',*,*,#23577,.T.);
#35937=ORIENTED_EDGE('',*,*,#26031,.F.);
#35938=ORIENTED_EDGE('',*,*,#24692,.F.);
#35939=ORIENTED_EDGE('',*,*,#26028,.T.);
#35940=ORIENTED_EDGE('',*,*,#23578,.T.);
#35941=ORIENTED_EDGE('',*,*,#26032,.F.);
#35942=ORIENTED_EDGE('',*,*,#24691,.F.);
#35943=ORIENTED_EDGE('',*,*,#26033,.T.);
#35944=ORIENTED_EDGE('',*,*,#23567,.T.);
#35945=ORIENTED_EDGE('',*,*,#26034,.F.);
#35946=ORIENTED_EDGE('',*,*,#24684,.F.);
#35947=ORIENTED_EDGE('',*,*,#26035,.T.);
#35948=ORIENTED_EDGE('',*,*,#23568,.T.);
#35949=ORIENTED_EDGE('',*,*,#26033,.F.);
#35950=ORIENTED_EDGE('',*,*,#24683,.F.);
#35951=ORIENTED_EDGE('',*,*,#26036,.T.);
#35952=ORIENTED_EDGE('',*,*,#23569,.T.);
#35953=ORIENTED_EDGE('',*,*,#26035,.F.);
#35954=ORIENTED_EDGE('',*,*,#24688,.F.);
#35955=ORIENTED_EDGE('',*,*,#26037,.T.);
#35956=ORIENTED_EDGE('',*,*,#23570,.T.);
#35957=ORIENTED_EDGE('',*,*,#26036,.F.);
#35958=ORIENTED_EDGE('',*,*,#24687,.F.);
#35959=ORIENTED_EDGE('',*,*,#26038,.T.);
#35960=ORIENTED_EDGE('',*,*,#23571,.T.);
#35961=ORIENTED_EDGE('',*,*,#26037,.F.);
#35962=ORIENTED_EDGE('',*,*,#24686,.F.);
#35963=ORIENTED_EDGE('',*,*,#26034,.T.);
#35964=ORIENTED_EDGE('',*,*,#23572,.T.);
#35965=ORIENTED_EDGE('',*,*,#26038,.F.);
#35966=ORIENTED_EDGE('',*,*,#24685,.F.);
#35967=ORIENTED_EDGE('',*,*,#26039,.T.);
#35968=ORIENTED_EDGE('',*,*,#23561,.T.);
#35969=ORIENTED_EDGE('',*,*,#26040,.F.);
#35970=ORIENTED_EDGE('',*,*,#24678,.F.);
#35971=ORIENTED_EDGE('',*,*,#26041,.T.);
#35972=ORIENTED_EDGE('',*,*,#23562,.T.);
#35973=ORIENTED_EDGE('',*,*,#26039,.F.);
#35974=ORIENTED_EDGE('',*,*,#24677,.F.);
#35975=ORIENTED_EDGE('',*,*,#26042,.T.);
#35976=ORIENTED_EDGE('',*,*,#23563,.T.);
#35977=ORIENTED_EDGE('',*,*,#26041,.F.);
#35978=ORIENTED_EDGE('',*,*,#24682,.F.);
#35979=ORIENTED_EDGE('',*,*,#26043,.T.);
#35980=ORIENTED_EDGE('',*,*,#23564,.T.);
#35981=ORIENTED_EDGE('',*,*,#26042,.F.);
#35982=ORIENTED_EDGE('',*,*,#24681,.F.);
#35983=ORIENTED_EDGE('',*,*,#26044,.T.);
#35984=ORIENTED_EDGE('',*,*,#23565,.T.);
#35985=ORIENTED_EDGE('',*,*,#26043,.F.);
#35986=ORIENTED_EDGE('',*,*,#24680,.F.);
#35987=ORIENTED_EDGE('',*,*,#26040,.T.);
#35988=ORIENTED_EDGE('',*,*,#23566,.T.);
#35989=ORIENTED_EDGE('',*,*,#26044,.F.);
#35990=ORIENTED_EDGE('',*,*,#24679,.F.);
#35991=ORIENTED_EDGE('',*,*,#26045,.T.);
#35992=ORIENTED_EDGE('',*,*,#23555,.T.);
#35993=ORIENTED_EDGE('',*,*,#26046,.F.);
#35994=ORIENTED_EDGE('',*,*,#24672,.F.);
#35995=ORIENTED_EDGE('',*,*,#26047,.T.);
#35996=ORIENTED_EDGE('',*,*,#23556,.T.);
#35997=ORIENTED_EDGE('',*,*,#26045,.F.);
#35998=ORIENTED_EDGE('',*,*,#24671,.F.);
#35999=ORIENTED_EDGE('',*,*,#26048,.T.);
#36000=ORIENTED_EDGE('',*,*,#23557,.T.);
#36001=ORIENTED_EDGE('',*,*,#26047,.F.);
#36002=ORIENTED_EDGE('',*,*,#24676,.F.);
#36003=ORIENTED_EDGE('',*,*,#26049,.T.);
#36004=ORIENTED_EDGE('',*,*,#23558,.T.);
#36005=ORIENTED_EDGE('',*,*,#26048,.F.);
#36006=ORIENTED_EDGE('',*,*,#24675,.F.);
#36007=ORIENTED_EDGE('',*,*,#26050,.T.);
#36008=ORIENTED_EDGE('',*,*,#23559,.T.);
#36009=ORIENTED_EDGE('',*,*,#26049,.F.);
#36010=ORIENTED_EDGE('',*,*,#24674,.F.);
#36011=ORIENTED_EDGE('',*,*,#26046,.T.);
#36012=ORIENTED_EDGE('',*,*,#23560,.T.);
#36013=ORIENTED_EDGE('',*,*,#26050,.F.);
#36014=ORIENTED_EDGE('',*,*,#24673,.F.);
#36015=ORIENTED_EDGE('',*,*,#26051,.T.);
#36016=ORIENTED_EDGE('',*,*,#23549,.T.);
#36017=ORIENTED_EDGE('',*,*,#26052,.F.);
#36018=ORIENTED_EDGE('',*,*,#24666,.F.);
#36019=ORIENTED_EDGE('',*,*,#26053,.T.);
#36020=ORIENTED_EDGE('',*,*,#23550,.T.);
#36021=ORIENTED_EDGE('',*,*,#26051,.F.);
#36022=ORIENTED_EDGE('',*,*,#24665,.F.);
#36023=ORIENTED_EDGE('',*,*,#26054,.T.);
#36024=ORIENTED_EDGE('',*,*,#23551,.T.);
#36025=ORIENTED_EDGE('',*,*,#26053,.F.);
#36026=ORIENTED_EDGE('',*,*,#24670,.F.);
#36027=ORIENTED_EDGE('',*,*,#26055,.T.);
#36028=ORIENTED_EDGE('',*,*,#23552,.T.);
#36029=ORIENTED_EDGE('',*,*,#26054,.F.);
#36030=ORIENTED_EDGE('',*,*,#24669,.F.);
#36031=ORIENTED_EDGE('',*,*,#26056,.T.);
#36032=ORIENTED_EDGE('',*,*,#23553,.T.);
#36033=ORIENTED_EDGE('',*,*,#26055,.F.);
#36034=ORIENTED_EDGE('',*,*,#24668,.F.);
#36035=ORIENTED_EDGE('',*,*,#26052,.T.);
#36036=ORIENTED_EDGE('',*,*,#23554,.T.);
#36037=ORIENTED_EDGE('',*,*,#26056,.F.);
#36038=ORIENTED_EDGE('',*,*,#24667,.F.);
#36039=ORIENTED_EDGE('',*,*,#26057,.T.);
#36040=ORIENTED_EDGE('',*,*,#23543,.T.);
#36041=ORIENTED_EDGE('',*,*,#26058,.F.);
#36042=ORIENTED_EDGE('',*,*,#24660,.F.);
#36043=ORIENTED_EDGE('',*,*,#26059,.T.);
#36044=ORIENTED_EDGE('',*,*,#23544,.T.);
#36045=ORIENTED_EDGE('',*,*,#26057,.F.);
#36046=ORIENTED_EDGE('',*,*,#24659,.F.);
#36047=ORIENTED_EDGE('',*,*,#26060,.T.);
#36048=ORIENTED_EDGE('',*,*,#23545,.T.);
#36049=ORIENTED_EDGE('',*,*,#26059,.F.);
#36050=ORIENTED_EDGE('',*,*,#24664,.F.);
#36051=ORIENTED_EDGE('',*,*,#26061,.T.);
#36052=ORIENTED_EDGE('',*,*,#23546,.T.);
#36053=ORIENTED_EDGE('',*,*,#26060,.F.);
#36054=ORIENTED_EDGE('',*,*,#24663,.F.);
#36055=ORIENTED_EDGE('',*,*,#26062,.T.);
#36056=ORIENTED_EDGE('',*,*,#23547,.T.);
#36057=ORIENTED_EDGE('',*,*,#26061,.F.);
#36058=ORIENTED_EDGE('',*,*,#24662,.F.);
#36059=ORIENTED_EDGE('',*,*,#26058,.T.);
#36060=ORIENTED_EDGE('',*,*,#23548,.T.);
#36061=ORIENTED_EDGE('',*,*,#26062,.F.);
#36062=ORIENTED_EDGE('',*,*,#24661,.F.);
#36063=ORIENTED_EDGE('',*,*,#26063,.T.);
#36064=ORIENTED_EDGE('',*,*,#23537,.T.);
#36065=ORIENTED_EDGE('',*,*,#26064,.F.);
#36066=ORIENTED_EDGE('',*,*,#24654,.F.);
#36067=ORIENTED_EDGE('',*,*,#26065,.T.);
#36068=ORIENTED_EDGE('',*,*,#23538,.T.);
#36069=ORIENTED_EDGE('',*,*,#26063,.F.);
#36070=ORIENTED_EDGE('',*,*,#24653,.F.);
#36071=ORIENTED_EDGE('',*,*,#26066,.T.);
#36072=ORIENTED_EDGE('',*,*,#23539,.T.);
#36073=ORIENTED_EDGE('',*,*,#26065,.F.);
#36074=ORIENTED_EDGE('',*,*,#24658,.F.);
#36075=ORIENTED_EDGE('',*,*,#26067,.T.);
#36076=ORIENTED_EDGE('',*,*,#23540,.T.);
#36077=ORIENTED_EDGE('',*,*,#26066,.F.);
#36078=ORIENTED_EDGE('',*,*,#24657,.F.);
#36079=ORIENTED_EDGE('',*,*,#26068,.T.);
#36080=ORIENTED_EDGE('',*,*,#23541,.T.);
#36081=ORIENTED_EDGE('',*,*,#26067,.F.);
#36082=ORIENTED_EDGE('',*,*,#24656,.F.);
#36083=ORIENTED_EDGE('',*,*,#26064,.T.);
#36084=ORIENTED_EDGE('',*,*,#23542,.T.);
#36085=ORIENTED_EDGE('',*,*,#26068,.F.);
#36086=ORIENTED_EDGE('',*,*,#24655,.F.);
#36087=ORIENTED_EDGE('',*,*,#26069,.T.);
#36088=ORIENTED_EDGE('',*,*,#23531,.T.);
#36089=ORIENTED_EDGE('',*,*,#26070,.F.);
#36090=ORIENTED_EDGE('',*,*,#24648,.F.);
#36091=ORIENTED_EDGE('',*,*,#26071,.T.);
#36092=ORIENTED_EDGE('',*,*,#23532,.T.);
#36093=ORIENTED_EDGE('',*,*,#26069,.F.);
#36094=ORIENTED_EDGE('',*,*,#24647,.F.);
#36095=ORIENTED_EDGE('',*,*,#26072,.T.);
#36096=ORIENTED_EDGE('',*,*,#23533,.T.);
#36097=ORIENTED_EDGE('',*,*,#26071,.F.);
#36098=ORIENTED_EDGE('',*,*,#24652,.F.);
#36099=ORIENTED_EDGE('',*,*,#26073,.T.);
#36100=ORIENTED_EDGE('',*,*,#23534,.T.);
#36101=ORIENTED_EDGE('',*,*,#26072,.F.);
#36102=ORIENTED_EDGE('',*,*,#24651,.F.);
#36103=ORIENTED_EDGE('',*,*,#26074,.T.);
#36104=ORIENTED_EDGE('',*,*,#23535,.T.);
#36105=ORIENTED_EDGE('',*,*,#26073,.F.);
#36106=ORIENTED_EDGE('',*,*,#24650,.F.);
#36107=ORIENTED_EDGE('',*,*,#26070,.T.);
#36108=ORIENTED_EDGE('',*,*,#23536,.T.);
#36109=ORIENTED_EDGE('',*,*,#26074,.F.);
#36110=ORIENTED_EDGE('',*,*,#24649,.F.);
#36111=ORIENTED_EDGE('',*,*,#26075,.T.);
#36112=ORIENTED_EDGE('',*,*,#23525,.T.);
#36113=ORIENTED_EDGE('',*,*,#26076,.F.);
#36114=ORIENTED_EDGE('',*,*,#24642,.F.);
#36115=ORIENTED_EDGE('',*,*,#26077,.T.);
#36116=ORIENTED_EDGE('',*,*,#23526,.T.);
#36117=ORIENTED_EDGE('',*,*,#26075,.F.);
#36118=ORIENTED_EDGE('',*,*,#24641,.F.);
#36119=ORIENTED_EDGE('',*,*,#26078,.T.);
#36120=ORIENTED_EDGE('',*,*,#23527,.T.);
#36121=ORIENTED_EDGE('',*,*,#26077,.F.);
#36122=ORIENTED_EDGE('',*,*,#24646,.F.);
#36123=ORIENTED_EDGE('',*,*,#26079,.T.);
#36124=ORIENTED_EDGE('',*,*,#23528,.T.);
#36125=ORIENTED_EDGE('',*,*,#26078,.F.);
#36126=ORIENTED_EDGE('',*,*,#24645,.F.);
#36127=ORIENTED_EDGE('',*,*,#26080,.T.);
#36128=ORIENTED_EDGE('',*,*,#23529,.T.);
#36129=ORIENTED_EDGE('',*,*,#26079,.F.);
#36130=ORIENTED_EDGE('',*,*,#24644,.F.);
#36131=ORIENTED_EDGE('',*,*,#26076,.T.);
#36132=ORIENTED_EDGE('',*,*,#23530,.T.);
#36133=ORIENTED_EDGE('',*,*,#26080,.F.);
#36134=ORIENTED_EDGE('',*,*,#24643,.F.);
#36135=ORIENTED_EDGE('',*,*,#26081,.T.);
#36136=ORIENTED_EDGE('',*,*,#23519,.T.);
#36137=ORIENTED_EDGE('',*,*,#26082,.F.);
#36138=ORIENTED_EDGE('',*,*,#24636,.F.);
#36139=ORIENTED_EDGE('',*,*,#26083,.T.);
#36140=ORIENTED_EDGE('',*,*,#23520,.T.);
#36141=ORIENTED_EDGE('',*,*,#26081,.F.);
#36142=ORIENTED_EDGE('',*,*,#24635,.F.);
#36143=ORIENTED_EDGE('',*,*,#26084,.T.);
#36144=ORIENTED_EDGE('',*,*,#23521,.T.);
#36145=ORIENTED_EDGE('',*,*,#26083,.F.);
#36146=ORIENTED_EDGE('',*,*,#24640,.F.);
#36147=ORIENTED_EDGE('',*,*,#26085,.T.);
#36148=ORIENTED_EDGE('',*,*,#23522,.T.);
#36149=ORIENTED_EDGE('',*,*,#26084,.F.);
#36150=ORIENTED_EDGE('',*,*,#24639,.F.);
#36151=ORIENTED_EDGE('',*,*,#26086,.T.);
#36152=ORIENTED_EDGE('',*,*,#23523,.T.);
#36153=ORIENTED_EDGE('',*,*,#26085,.F.);
#36154=ORIENTED_EDGE('',*,*,#24638,.F.);
#36155=ORIENTED_EDGE('',*,*,#26082,.T.);
#36156=ORIENTED_EDGE('',*,*,#23524,.T.);
#36157=ORIENTED_EDGE('',*,*,#26086,.F.);
#36158=ORIENTED_EDGE('',*,*,#24637,.F.);
#36159=ORIENTED_EDGE('',*,*,#26087,.T.);
#36160=ORIENTED_EDGE('',*,*,#23513,.T.);
#36161=ORIENTED_EDGE('',*,*,#26088,.F.);
#36162=ORIENTED_EDGE('',*,*,#24630,.F.);
#36163=ORIENTED_EDGE('',*,*,#26089,.T.);
#36164=ORIENTED_EDGE('',*,*,#23514,.T.);
#36165=ORIENTED_EDGE('',*,*,#26087,.F.);
#36166=ORIENTED_EDGE('',*,*,#24629,.F.);
#36167=ORIENTED_EDGE('',*,*,#26090,.T.);
#36168=ORIENTED_EDGE('',*,*,#23515,.T.);
#36169=ORIENTED_EDGE('',*,*,#26089,.F.);
#36170=ORIENTED_EDGE('',*,*,#24634,.F.);
#36171=ORIENTED_EDGE('',*,*,#26091,.T.);
#36172=ORIENTED_EDGE('',*,*,#23516,.T.);
#36173=ORIENTED_EDGE('',*,*,#26090,.F.);
#36174=ORIENTED_EDGE('',*,*,#24633,.F.);
#36175=ORIENTED_EDGE('',*,*,#26092,.T.);
#36176=ORIENTED_EDGE('',*,*,#23517,.T.);
#36177=ORIENTED_EDGE('',*,*,#26091,.F.);
#36178=ORIENTED_EDGE('',*,*,#24632,.F.);
#36179=ORIENTED_EDGE('',*,*,#26088,.T.);
#36180=ORIENTED_EDGE('',*,*,#23518,.T.);
#36181=ORIENTED_EDGE('',*,*,#26092,.F.);
#36182=ORIENTED_EDGE('',*,*,#24631,.F.);
#36183=ORIENTED_EDGE('',*,*,#26093,.T.);
#36184=ORIENTED_EDGE('',*,*,#23507,.T.);
#36185=ORIENTED_EDGE('',*,*,#26094,.F.);
#36186=ORIENTED_EDGE('',*,*,#24624,.F.);
#36187=ORIENTED_EDGE('',*,*,#26095,.T.);
#36188=ORIENTED_EDGE('',*,*,#23508,.T.);
#36189=ORIENTED_EDGE('',*,*,#26093,.F.);
#36190=ORIENTED_EDGE('',*,*,#24623,.F.);
#36191=ORIENTED_EDGE('',*,*,#26096,.T.);
#36192=ORIENTED_EDGE('',*,*,#23509,.T.);
#36193=ORIENTED_EDGE('',*,*,#26095,.F.);
#36194=ORIENTED_EDGE('',*,*,#24628,.F.);
#36195=ORIENTED_EDGE('',*,*,#26097,.T.);
#36196=ORIENTED_EDGE('',*,*,#23510,.T.);
#36197=ORIENTED_EDGE('',*,*,#26096,.F.);
#36198=ORIENTED_EDGE('',*,*,#24627,.F.);
#36199=ORIENTED_EDGE('',*,*,#26098,.T.);
#36200=ORIENTED_EDGE('',*,*,#23511,.T.);
#36201=ORIENTED_EDGE('',*,*,#26097,.F.);
#36202=ORIENTED_EDGE('',*,*,#24626,.F.);
#36203=ORIENTED_EDGE('',*,*,#26094,.T.);
#36204=ORIENTED_EDGE('',*,*,#23512,.T.);
#36205=ORIENTED_EDGE('',*,*,#26098,.F.);
#36206=ORIENTED_EDGE('',*,*,#24625,.F.);
#36207=ORIENTED_EDGE('',*,*,#26099,.T.);
#36208=ORIENTED_EDGE('',*,*,#23501,.T.);
#36209=ORIENTED_EDGE('',*,*,#26100,.F.);
#36210=ORIENTED_EDGE('',*,*,#24618,.F.);
#36211=ORIENTED_EDGE('',*,*,#26101,.T.);
#36212=ORIENTED_EDGE('',*,*,#23502,.T.);
#36213=ORIENTED_EDGE('',*,*,#26099,.F.);
#36214=ORIENTED_EDGE('',*,*,#24617,.F.);
#36215=ORIENTED_EDGE('',*,*,#26102,.T.);
#36216=ORIENTED_EDGE('',*,*,#23503,.T.);
#36217=ORIENTED_EDGE('',*,*,#26101,.F.);
#36218=ORIENTED_EDGE('',*,*,#24622,.F.);
#36219=ORIENTED_EDGE('',*,*,#26103,.T.);
#36220=ORIENTED_EDGE('',*,*,#23504,.T.);
#36221=ORIENTED_EDGE('',*,*,#26102,.F.);
#36222=ORIENTED_EDGE('',*,*,#24621,.F.);
#36223=ORIENTED_EDGE('',*,*,#26104,.T.);
#36224=ORIENTED_EDGE('',*,*,#23505,.T.);
#36225=ORIENTED_EDGE('',*,*,#26103,.F.);
#36226=ORIENTED_EDGE('',*,*,#24620,.F.);
#36227=ORIENTED_EDGE('',*,*,#26100,.T.);
#36228=ORIENTED_EDGE('',*,*,#23506,.T.);
#36229=ORIENTED_EDGE('',*,*,#26104,.F.);
#36230=ORIENTED_EDGE('',*,*,#24619,.F.);
#36231=ORIENTED_EDGE('',*,*,#26105,.T.);
#36232=ORIENTED_EDGE('',*,*,#23495,.T.);
#36233=ORIENTED_EDGE('',*,*,#26106,.F.);
#36234=ORIENTED_EDGE('',*,*,#24612,.F.);
#36235=ORIENTED_EDGE('',*,*,#26107,.T.);
#36236=ORIENTED_EDGE('',*,*,#23496,.T.);
#36237=ORIENTED_EDGE('',*,*,#26105,.F.);
#36238=ORIENTED_EDGE('',*,*,#24611,.F.);
#36239=ORIENTED_EDGE('',*,*,#26108,.T.);
#36240=ORIENTED_EDGE('',*,*,#23497,.T.);
#36241=ORIENTED_EDGE('',*,*,#26107,.F.);
#36242=ORIENTED_EDGE('',*,*,#24616,.F.);
#36243=ORIENTED_EDGE('',*,*,#26109,.T.);
#36244=ORIENTED_EDGE('',*,*,#23498,.T.);
#36245=ORIENTED_EDGE('',*,*,#26108,.F.);
#36246=ORIENTED_EDGE('',*,*,#24615,.F.);
#36247=ORIENTED_EDGE('',*,*,#26110,.T.);
#36248=ORIENTED_EDGE('',*,*,#23499,.T.);
#36249=ORIENTED_EDGE('',*,*,#26109,.F.);
#36250=ORIENTED_EDGE('',*,*,#24614,.F.);
#36251=ORIENTED_EDGE('',*,*,#26106,.T.);
#36252=ORIENTED_EDGE('',*,*,#23500,.T.);
#36253=ORIENTED_EDGE('',*,*,#26110,.F.);
#36254=ORIENTED_EDGE('',*,*,#24613,.F.);
#36255=ORIENTED_EDGE('',*,*,#26111,.T.);
#36256=ORIENTED_EDGE('',*,*,#23489,.T.);
#36257=ORIENTED_EDGE('',*,*,#26112,.F.);
#36258=ORIENTED_EDGE('',*,*,#24606,.F.);
#36259=ORIENTED_EDGE('',*,*,#26113,.T.);
#36260=ORIENTED_EDGE('',*,*,#23490,.T.);
#36261=ORIENTED_EDGE('',*,*,#26111,.F.);
#36262=ORIENTED_EDGE('',*,*,#24605,.F.);
#36263=ORIENTED_EDGE('',*,*,#26114,.T.);
#36264=ORIENTED_EDGE('',*,*,#23491,.T.);
#36265=ORIENTED_EDGE('',*,*,#26113,.F.);
#36266=ORIENTED_EDGE('',*,*,#24610,.F.);
#36267=ORIENTED_EDGE('',*,*,#26115,.T.);
#36268=ORIENTED_EDGE('',*,*,#23492,.T.);
#36269=ORIENTED_EDGE('',*,*,#26114,.F.);
#36270=ORIENTED_EDGE('',*,*,#24609,.F.);
#36271=ORIENTED_EDGE('',*,*,#26116,.T.);
#36272=ORIENTED_EDGE('',*,*,#23493,.T.);
#36273=ORIENTED_EDGE('',*,*,#26115,.F.);
#36274=ORIENTED_EDGE('',*,*,#24608,.F.);
#36275=ORIENTED_EDGE('',*,*,#26112,.T.);
#36276=ORIENTED_EDGE('',*,*,#23494,.T.);
#36277=ORIENTED_EDGE('',*,*,#26116,.F.);
#36278=ORIENTED_EDGE('',*,*,#24607,.F.);
#36279=ORIENTED_EDGE('',*,*,#26117,.T.);
#36280=ORIENTED_EDGE('',*,*,#23483,.T.);
#36281=ORIENTED_EDGE('',*,*,#26118,.F.);
#36282=ORIENTED_EDGE('',*,*,#24600,.F.);
#36283=ORIENTED_EDGE('',*,*,#26119,.T.);
#36284=ORIENTED_EDGE('',*,*,#23484,.T.);
#36285=ORIENTED_EDGE('',*,*,#26117,.F.);
#36286=ORIENTED_EDGE('',*,*,#24599,.F.);
#36287=ORIENTED_EDGE('',*,*,#26120,.T.);
#36288=ORIENTED_EDGE('',*,*,#23485,.T.);
#36289=ORIENTED_EDGE('',*,*,#26119,.F.);
#36290=ORIENTED_EDGE('',*,*,#24604,.F.);
#36291=ORIENTED_EDGE('',*,*,#26121,.T.);
#36292=ORIENTED_EDGE('',*,*,#23486,.T.);
#36293=ORIENTED_EDGE('',*,*,#26120,.F.);
#36294=ORIENTED_EDGE('',*,*,#24603,.F.);
#36295=ORIENTED_EDGE('',*,*,#26122,.T.);
#36296=ORIENTED_EDGE('',*,*,#23487,.T.);
#36297=ORIENTED_EDGE('',*,*,#26121,.F.);
#36298=ORIENTED_EDGE('',*,*,#24602,.F.);
#36299=ORIENTED_EDGE('',*,*,#26118,.T.);
#36300=ORIENTED_EDGE('',*,*,#23488,.T.);
#36301=ORIENTED_EDGE('',*,*,#26122,.F.);
#36302=ORIENTED_EDGE('',*,*,#24601,.F.);
#36303=ORIENTED_EDGE('',*,*,#26123,.T.);
#36304=ORIENTED_EDGE('',*,*,#23477,.T.);
#36305=ORIENTED_EDGE('',*,*,#26124,.F.);
#36306=ORIENTED_EDGE('',*,*,#24594,.F.);
#36307=ORIENTED_EDGE('',*,*,#26125,.T.);
#36308=ORIENTED_EDGE('',*,*,#23478,.T.);
#36309=ORIENTED_EDGE('',*,*,#26123,.F.);
#36310=ORIENTED_EDGE('',*,*,#24593,.F.);
#36311=ORIENTED_EDGE('',*,*,#26126,.T.);
#36312=ORIENTED_EDGE('',*,*,#23479,.T.);
#36313=ORIENTED_EDGE('',*,*,#26125,.F.);
#36314=ORIENTED_EDGE('',*,*,#24598,.F.);
#36315=ORIENTED_EDGE('',*,*,#26127,.T.);
#36316=ORIENTED_EDGE('',*,*,#23480,.T.);
#36317=ORIENTED_EDGE('',*,*,#26126,.F.);
#36318=ORIENTED_EDGE('',*,*,#24597,.F.);
#36319=ORIENTED_EDGE('',*,*,#26128,.T.);
#36320=ORIENTED_EDGE('',*,*,#23481,.T.);
#36321=ORIENTED_EDGE('',*,*,#26127,.F.);
#36322=ORIENTED_EDGE('',*,*,#24596,.F.);
#36323=ORIENTED_EDGE('',*,*,#26124,.T.);
#36324=ORIENTED_EDGE('',*,*,#23482,.T.);
#36325=ORIENTED_EDGE('',*,*,#26128,.F.);
#36326=ORIENTED_EDGE('',*,*,#24595,.F.);
#36327=ORIENTED_EDGE('',*,*,#26129,.T.);
#36328=ORIENTED_EDGE('',*,*,#23471,.T.);
#36329=ORIENTED_EDGE('',*,*,#26130,.F.);
#36330=ORIENTED_EDGE('',*,*,#24588,.F.);
#36331=ORIENTED_EDGE('',*,*,#26131,.T.);
#36332=ORIENTED_EDGE('',*,*,#23472,.T.);
#36333=ORIENTED_EDGE('',*,*,#26129,.F.);
#36334=ORIENTED_EDGE('',*,*,#24587,.F.);
#36335=ORIENTED_EDGE('',*,*,#26132,.T.);
#36336=ORIENTED_EDGE('',*,*,#23473,.T.);
#36337=ORIENTED_EDGE('',*,*,#26131,.F.);
#36338=ORIENTED_EDGE('',*,*,#24592,.F.);
#36339=ORIENTED_EDGE('',*,*,#26133,.T.);
#36340=ORIENTED_EDGE('',*,*,#23474,.T.);
#36341=ORIENTED_EDGE('',*,*,#26132,.F.);
#36342=ORIENTED_EDGE('',*,*,#24591,.F.);
#36343=ORIENTED_EDGE('',*,*,#26134,.T.);
#36344=ORIENTED_EDGE('',*,*,#23475,.T.);
#36345=ORIENTED_EDGE('',*,*,#26133,.F.);
#36346=ORIENTED_EDGE('',*,*,#24590,.F.);
#36347=ORIENTED_EDGE('',*,*,#26130,.T.);
#36348=ORIENTED_EDGE('',*,*,#23476,.T.);
#36349=ORIENTED_EDGE('',*,*,#26134,.F.);
#36350=ORIENTED_EDGE('',*,*,#24589,.F.);
#36351=ORIENTED_EDGE('',*,*,#26135,.T.);
#36352=ORIENTED_EDGE('',*,*,#23465,.T.);
#36353=ORIENTED_EDGE('',*,*,#26136,.F.);
#36354=ORIENTED_EDGE('',*,*,#24582,.F.);
#36355=ORIENTED_EDGE('',*,*,#26137,.T.);
#36356=ORIENTED_EDGE('',*,*,#23466,.T.);
#36357=ORIENTED_EDGE('',*,*,#26135,.F.);
#36358=ORIENTED_EDGE('',*,*,#24581,.F.);
#36359=ORIENTED_EDGE('',*,*,#26138,.T.);
#36360=ORIENTED_EDGE('',*,*,#23467,.T.);
#36361=ORIENTED_EDGE('',*,*,#26137,.F.);
#36362=ORIENTED_EDGE('',*,*,#24586,.F.);
#36363=ORIENTED_EDGE('',*,*,#26139,.T.);
#36364=ORIENTED_EDGE('',*,*,#23468,.T.);
#36365=ORIENTED_EDGE('',*,*,#26138,.F.);
#36366=ORIENTED_EDGE('',*,*,#24585,.F.);
#36367=ORIENTED_EDGE('',*,*,#26140,.T.);
#36368=ORIENTED_EDGE('',*,*,#23469,.T.);
#36369=ORIENTED_EDGE('',*,*,#26139,.F.);
#36370=ORIENTED_EDGE('',*,*,#24584,.F.);
#36371=ORIENTED_EDGE('',*,*,#26136,.T.);
#36372=ORIENTED_EDGE('',*,*,#23470,.T.);
#36373=ORIENTED_EDGE('',*,*,#26140,.F.);
#36374=ORIENTED_EDGE('',*,*,#24583,.F.);
#36375=ORIENTED_EDGE('',*,*,#26141,.T.);
#36376=ORIENTED_EDGE('',*,*,#23459,.T.);
#36377=ORIENTED_EDGE('',*,*,#26142,.F.);
#36378=ORIENTED_EDGE('',*,*,#24576,.F.);
#36379=ORIENTED_EDGE('',*,*,#26143,.T.);
#36380=ORIENTED_EDGE('',*,*,#23460,.T.);
#36381=ORIENTED_EDGE('',*,*,#26141,.F.);
#36382=ORIENTED_EDGE('',*,*,#24575,.F.);
#36383=ORIENTED_EDGE('',*,*,#26144,.T.);
#36384=ORIENTED_EDGE('',*,*,#23461,.T.);
#36385=ORIENTED_EDGE('',*,*,#26143,.F.);
#36386=ORIENTED_EDGE('',*,*,#24580,.F.);
#36387=ORIENTED_EDGE('',*,*,#26145,.T.);
#36388=ORIENTED_EDGE('',*,*,#23462,.T.);
#36389=ORIENTED_EDGE('',*,*,#26144,.F.);
#36390=ORIENTED_EDGE('',*,*,#24579,.F.);
#36391=ORIENTED_EDGE('',*,*,#26146,.T.);
#36392=ORIENTED_EDGE('',*,*,#23463,.T.);
#36393=ORIENTED_EDGE('',*,*,#26145,.F.);
#36394=ORIENTED_EDGE('',*,*,#24578,.F.);
#36395=ORIENTED_EDGE('',*,*,#26142,.T.);
#36396=ORIENTED_EDGE('',*,*,#23464,.T.);
#36397=ORIENTED_EDGE('',*,*,#26146,.F.);
#36398=ORIENTED_EDGE('',*,*,#24577,.F.);
#36399=ORIENTED_EDGE('',*,*,#26147,.T.);
#36400=ORIENTED_EDGE('',*,*,#23453,.T.);
#36401=ORIENTED_EDGE('',*,*,#26148,.F.);
#36402=ORIENTED_EDGE('',*,*,#24570,.F.);
#36403=ORIENTED_EDGE('',*,*,#26149,.T.);
#36404=ORIENTED_EDGE('',*,*,#23454,.T.);
#36405=ORIENTED_EDGE('',*,*,#26147,.F.);
#36406=ORIENTED_EDGE('',*,*,#24569,.F.);
#36407=ORIENTED_EDGE('',*,*,#26150,.T.);
#36408=ORIENTED_EDGE('',*,*,#23455,.T.);
#36409=ORIENTED_EDGE('',*,*,#26149,.F.);
#36410=ORIENTED_EDGE('',*,*,#24574,.F.);
#36411=ORIENTED_EDGE('',*,*,#26151,.T.);
#36412=ORIENTED_EDGE('',*,*,#23456,.T.);
#36413=ORIENTED_EDGE('',*,*,#26150,.F.);
#36414=ORIENTED_EDGE('',*,*,#24573,.F.);
#36415=ORIENTED_EDGE('',*,*,#26152,.T.);
#36416=ORIENTED_EDGE('',*,*,#23457,.T.);
#36417=ORIENTED_EDGE('',*,*,#26151,.F.);
#36418=ORIENTED_EDGE('',*,*,#24572,.F.);
#36419=ORIENTED_EDGE('',*,*,#26148,.T.);
#36420=ORIENTED_EDGE('',*,*,#23458,.T.);
#36421=ORIENTED_EDGE('',*,*,#26152,.F.);
#36422=ORIENTED_EDGE('',*,*,#24571,.F.);
#36423=ORIENTED_EDGE('',*,*,#26153,.T.);
#36424=ORIENTED_EDGE('',*,*,#23447,.T.);
#36425=ORIENTED_EDGE('',*,*,#26154,.F.);
#36426=ORIENTED_EDGE('',*,*,#24564,.F.);
#36427=ORIENTED_EDGE('',*,*,#26155,.T.);
#36428=ORIENTED_EDGE('',*,*,#23448,.T.);
#36429=ORIENTED_EDGE('',*,*,#26153,.F.);
#36430=ORIENTED_EDGE('',*,*,#24563,.F.);
#36431=ORIENTED_EDGE('',*,*,#26156,.T.);
#36432=ORIENTED_EDGE('',*,*,#23449,.T.);
#36433=ORIENTED_EDGE('',*,*,#26155,.F.);
#36434=ORIENTED_EDGE('',*,*,#24568,.F.);
#36435=ORIENTED_EDGE('',*,*,#26157,.T.);
#36436=ORIENTED_EDGE('',*,*,#23450,.T.);
#36437=ORIENTED_EDGE('',*,*,#26156,.F.);
#36438=ORIENTED_EDGE('',*,*,#24567,.F.);
#36439=ORIENTED_EDGE('',*,*,#26158,.T.);
#36440=ORIENTED_EDGE('',*,*,#23451,.T.);
#36441=ORIENTED_EDGE('',*,*,#26157,.F.);
#36442=ORIENTED_EDGE('',*,*,#24566,.F.);
#36443=ORIENTED_EDGE('',*,*,#26154,.T.);
#36444=ORIENTED_EDGE('',*,*,#23452,.T.);
#36445=ORIENTED_EDGE('',*,*,#26158,.F.);
#36446=ORIENTED_EDGE('',*,*,#24565,.F.);
#36447=ORIENTED_EDGE('',*,*,#26159,.T.);
#36448=ORIENTED_EDGE('',*,*,#23441,.T.);
#36449=ORIENTED_EDGE('',*,*,#26160,.F.);
#36450=ORIENTED_EDGE('',*,*,#24558,.F.);
#36451=ORIENTED_EDGE('',*,*,#26161,.T.);
#36452=ORIENTED_EDGE('',*,*,#23442,.T.);
#36453=ORIENTED_EDGE('',*,*,#26159,.F.);
#36454=ORIENTED_EDGE('',*,*,#24557,.F.);
#36455=ORIENTED_EDGE('',*,*,#26162,.T.);
#36456=ORIENTED_EDGE('',*,*,#23443,.T.);
#36457=ORIENTED_EDGE('',*,*,#26161,.F.);
#36458=ORIENTED_EDGE('',*,*,#24562,.F.);
#36459=ORIENTED_EDGE('',*,*,#26163,.T.);
#36460=ORIENTED_EDGE('',*,*,#23444,.T.);
#36461=ORIENTED_EDGE('',*,*,#26162,.F.);
#36462=ORIENTED_EDGE('',*,*,#24561,.F.);
#36463=ORIENTED_EDGE('',*,*,#26164,.T.);
#36464=ORIENTED_EDGE('',*,*,#23445,.T.);
#36465=ORIENTED_EDGE('',*,*,#26163,.F.);
#36466=ORIENTED_EDGE('',*,*,#24560,.F.);
#36467=ORIENTED_EDGE('',*,*,#26160,.T.);
#36468=ORIENTED_EDGE('',*,*,#23446,.T.);
#36469=ORIENTED_EDGE('',*,*,#26164,.F.);
#36470=ORIENTED_EDGE('',*,*,#24559,.F.);
#36471=ORIENTED_EDGE('',*,*,#26165,.T.);
#36472=ORIENTED_EDGE('',*,*,#23435,.T.);
#36473=ORIENTED_EDGE('',*,*,#26166,.F.);
#36474=ORIENTED_EDGE('',*,*,#24552,.F.);
#36475=ORIENTED_EDGE('',*,*,#26167,.T.);
#36476=ORIENTED_EDGE('',*,*,#23436,.T.);
#36477=ORIENTED_EDGE('',*,*,#26165,.F.);
#36478=ORIENTED_EDGE('',*,*,#24551,.F.);
#36479=ORIENTED_EDGE('',*,*,#26168,.T.);
#36480=ORIENTED_EDGE('',*,*,#23437,.T.);
#36481=ORIENTED_EDGE('',*,*,#26167,.F.);
#36482=ORIENTED_EDGE('',*,*,#24556,.F.);
#36483=ORIENTED_EDGE('',*,*,#26169,.T.);
#36484=ORIENTED_EDGE('',*,*,#23438,.T.);
#36485=ORIENTED_EDGE('',*,*,#26168,.F.);
#36486=ORIENTED_EDGE('',*,*,#24555,.F.);
#36487=ORIENTED_EDGE('',*,*,#26170,.T.);
#36488=ORIENTED_EDGE('',*,*,#23439,.T.);
#36489=ORIENTED_EDGE('',*,*,#26169,.F.);
#36490=ORIENTED_EDGE('',*,*,#24554,.F.);
#36491=ORIENTED_EDGE('',*,*,#26166,.T.);
#36492=ORIENTED_EDGE('',*,*,#23440,.T.);
#36493=ORIENTED_EDGE('',*,*,#26170,.F.);
#36494=ORIENTED_EDGE('',*,*,#24553,.F.);
#36495=ORIENTED_EDGE('',*,*,#26171,.T.);
#36496=ORIENTED_EDGE('',*,*,#23429,.T.);
#36497=ORIENTED_EDGE('',*,*,#26172,.F.);
#36498=ORIENTED_EDGE('',*,*,#24546,.F.);
#36499=ORIENTED_EDGE('',*,*,#26173,.T.);
#36500=ORIENTED_EDGE('',*,*,#23430,.T.);
#36501=ORIENTED_EDGE('',*,*,#26171,.F.);
#36502=ORIENTED_EDGE('',*,*,#24545,.F.);
#36503=ORIENTED_EDGE('',*,*,#26174,.T.);
#36504=ORIENTED_EDGE('',*,*,#23431,.T.);
#36505=ORIENTED_EDGE('',*,*,#26173,.F.);
#36506=ORIENTED_EDGE('',*,*,#24550,.F.);
#36507=ORIENTED_EDGE('',*,*,#26175,.T.);
#36508=ORIENTED_EDGE('',*,*,#23432,.T.);
#36509=ORIENTED_EDGE('',*,*,#26174,.F.);
#36510=ORIENTED_EDGE('',*,*,#24549,.F.);
#36511=ORIENTED_EDGE('',*,*,#26176,.T.);
#36512=ORIENTED_EDGE('',*,*,#23433,.T.);
#36513=ORIENTED_EDGE('',*,*,#26175,.F.);
#36514=ORIENTED_EDGE('',*,*,#24548,.F.);
#36515=ORIENTED_EDGE('',*,*,#26172,.T.);
#36516=ORIENTED_EDGE('',*,*,#23434,.T.);
#36517=ORIENTED_EDGE('',*,*,#26176,.F.);
#36518=ORIENTED_EDGE('',*,*,#24547,.F.);
#36519=ORIENTED_EDGE('',*,*,#26177,.T.);
#36520=ORIENTED_EDGE('',*,*,#23423,.T.);
#36521=ORIENTED_EDGE('',*,*,#26178,.F.);
#36522=ORIENTED_EDGE('',*,*,#24540,.F.);
#36523=ORIENTED_EDGE('',*,*,#26179,.T.);
#36524=ORIENTED_EDGE('',*,*,#23424,.T.);
#36525=ORIENTED_EDGE('',*,*,#26177,.F.);
#36526=ORIENTED_EDGE('',*,*,#24539,.F.);
#36527=ORIENTED_EDGE('',*,*,#26180,.T.);
#36528=ORIENTED_EDGE('',*,*,#23425,.T.);
#36529=ORIENTED_EDGE('',*,*,#26179,.F.);
#36530=ORIENTED_EDGE('',*,*,#24544,.F.);
#36531=ORIENTED_EDGE('',*,*,#26181,.T.);
#36532=ORIENTED_EDGE('',*,*,#23426,.T.);
#36533=ORIENTED_EDGE('',*,*,#26180,.F.);
#36534=ORIENTED_EDGE('',*,*,#24543,.F.);
#36535=ORIENTED_EDGE('',*,*,#26182,.T.);
#36536=ORIENTED_EDGE('',*,*,#23427,.T.);
#36537=ORIENTED_EDGE('',*,*,#26181,.F.);
#36538=ORIENTED_EDGE('',*,*,#24542,.F.);
#36539=ORIENTED_EDGE('',*,*,#26178,.T.);
#36540=ORIENTED_EDGE('',*,*,#23428,.T.);
#36541=ORIENTED_EDGE('',*,*,#26182,.F.);
#36542=ORIENTED_EDGE('',*,*,#24541,.F.);
#36543=ORIENTED_EDGE('',*,*,#26183,.T.);
#36544=ORIENTED_EDGE('',*,*,#23417,.T.);
#36545=ORIENTED_EDGE('',*,*,#26184,.F.);
#36546=ORIENTED_EDGE('',*,*,#24534,.F.);
#36547=ORIENTED_EDGE('',*,*,#26185,.T.);
#36548=ORIENTED_EDGE('',*,*,#23418,.T.);
#36549=ORIENTED_EDGE('',*,*,#26183,.F.);
#36550=ORIENTED_EDGE('',*,*,#24533,.F.);
#36551=ORIENTED_EDGE('',*,*,#26186,.T.);
#36552=ORIENTED_EDGE('',*,*,#23419,.T.);
#36553=ORIENTED_EDGE('',*,*,#26185,.F.);
#36554=ORIENTED_EDGE('',*,*,#24538,.F.);
#36555=ORIENTED_EDGE('',*,*,#26187,.T.);
#36556=ORIENTED_EDGE('',*,*,#23420,.T.);
#36557=ORIENTED_EDGE('',*,*,#26186,.F.);
#36558=ORIENTED_EDGE('',*,*,#24537,.F.);
#36559=ORIENTED_EDGE('',*,*,#26188,.T.);
#36560=ORIENTED_EDGE('',*,*,#23421,.T.);
#36561=ORIENTED_EDGE('',*,*,#26187,.F.);
#36562=ORIENTED_EDGE('',*,*,#24536,.F.);
#36563=ORIENTED_EDGE('',*,*,#26184,.T.);
#36564=ORIENTED_EDGE('',*,*,#23422,.T.);
#36565=ORIENTED_EDGE('',*,*,#26188,.F.);
#36566=ORIENTED_EDGE('',*,*,#24535,.F.);
#36567=ORIENTED_EDGE('',*,*,#26189,.T.);
#36568=ORIENTED_EDGE('',*,*,#23411,.T.);
#36569=ORIENTED_EDGE('',*,*,#26190,.F.);
#36570=ORIENTED_EDGE('',*,*,#24528,.F.);
#36571=ORIENTED_EDGE('',*,*,#26191,.T.);
#36572=ORIENTED_EDGE('',*,*,#23412,.T.);
#36573=ORIENTED_EDGE('',*,*,#26189,.F.);
#36574=ORIENTED_EDGE('',*,*,#24527,.F.);
#36575=ORIENTED_EDGE('',*,*,#26192,.T.);
#36576=ORIENTED_EDGE('',*,*,#23413,.T.);
#36577=ORIENTED_EDGE('',*,*,#26191,.F.);
#36578=ORIENTED_EDGE('',*,*,#24532,.F.);
#36579=ORIENTED_EDGE('',*,*,#26193,.T.);
#36580=ORIENTED_EDGE('',*,*,#23414,.T.);
#36581=ORIENTED_EDGE('',*,*,#26192,.F.);
#36582=ORIENTED_EDGE('',*,*,#24531,.F.);
#36583=ORIENTED_EDGE('',*,*,#26194,.T.);
#36584=ORIENTED_EDGE('',*,*,#23415,.T.);
#36585=ORIENTED_EDGE('',*,*,#26193,.F.);
#36586=ORIENTED_EDGE('',*,*,#24530,.F.);
#36587=ORIENTED_EDGE('',*,*,#26190,.T.);
#36588=ORIENTED_EDGE('',*,*,#23416,.T.);
#36589=ORIENTED_EDGE('',*,*,#26194,.F.);
#36590=ORIENTED_EDGE('',*,*,#24529,.F.);
#36591=ORIENTED_EDGE('',*,*,#26195,.T.);
#36592=ORIENTED_EDGE('',*,*,#23405,.T.);
#36593=ORIENTED_EDGE('',*,*,#26196,.F.);
#36594=ORIENTED_EDGE('',*,*,#24522,.F.);
#36595=ORIENTED_EDGE('',*,*,#26197,.T.);
#36596=ORIENTED_EDGE('',*,*,#23406,.T.);
#36597=ORIENTED_EDGE('',*,*,#26195,.F.);
#36598=ORIENTED_EDGE('',*,*,#24521,.F.);
#36599=ORIENTED_EDGE('',*,*,#26198,.T.);
#36600=ORIENTED_EDGE('',*,*,#23407,.T.);
#36601=ORIENTED_EDGE('',*,*,#26197,.F.);
#36602=ORIENTED_EDGE('',*,*,#24526,.F.);
#36603=ORIENTED_EDGE('',*,*,#26199,.T.);
#36604=ORIENTED_EDGE('',*,*,#23408,.T.);
#36605=ORIENTED_EDGE('',*,*,#26198,.F.);
#36606=ORIENTED_EDGE('',*,*,#24525,.F.);
#36607=ORIENTED_EDGE('',*,*,#26200,.T.);
#36608=ORIENTED_EDGE('',*,*,#23409,.T.);
#36609=ORIENTED_EDGE('',*,*,#26199,.F.);
#36610=ORIENTED_EDGE('',*,*,#24524,.F.);
#36611=ORIENTED_EDGE('',*,*,#26196,.T.);
#36612=ORIENTED_EDGE('',*,*,#23410,.T.);
#36613=ORIENTED_EDGE('',*,*,#26200,.F.);
#36614=ORIENTED_EDGE('',*,*,#24523,.F.);
#36615=ORIENTED_EDGE('',*,*,#26201,.T.);
#36616=ORIENTED_EDGE('',*,*,#23399,.T.);
#36617=ORIENTED_EDGE('',*,*,#26202,.F.);
#36618=ORIENTED_EDGE('',*,*,#24516,.F.);
#36619=ORIENTED_EDGE('',*,*,#26203,.T.);
#36620=ORIENTED_EDGE('',*,*,#23400,.T.);
#36621=ORIENTED_EDGE('',*,*,#26201,.F.);
#36622=ORIENTED_EDGE('',*,*,#24515,.F.);
#36623=ORIENTED_EDGE('',*,*,#26204,.T.);
#36624=ORIENTED_EDGE('',*,*,#23401,.T.);
#36625=ORIENTED_EDGE('',*,*,#26203,.F.);
#36626=ORIENTED_EDGE('',*,*,#24520,.F.);
#36627=ORIENTED_EDGE('',*,*,#26205,.T.);
#36628=ORIENTED_EDGE('',*,*,#23402,.T.);
#36629=ORIENTED_EDGE('',*,*,#26204,.F.);
#36630=ORIENTED_EDGE('',*,*,#24519,.F.);
#36631=ORIENTED_EDGE('',*,*,#26206,.T.);
#36632=ORIENTED_EDGE('',*,*,#23403,.T.);
#36633=ORIENTED_EDGE('',*,*,#26205,.F.);
#36634=ORIENTED_EDGE('',*,*,#24518,.F.);
#36635=ORIENTED_EDGE('',*,*,#26202,.T.);
#36636=ORIENTED_EDGE('',*,*,#23404,.T.);
#36637=ORIENTED_EDGE('',*,*,#26206,.F.);
#36638=ORIENTED_EDGE('',*,*,#24517,.F.);
#36639=ORIENTED_EDGE('',*,*,#26207,.T.);
#36640=ORIENTED_EDGE('',*,*,#23393,.T.);
#36641=ORIENTED_EDGE('',*,*,#26208,.F.);
#36642=ORIENTED_EDGE('',*,*,#24510,.F.);
#36643=ORIENTED_EDGE('',*,*,#26209,.T.);
#36644=ORIENTED_EDGE('',*,*,#23394,.T.);
#36645=ORIENTED_EDGE('',*,*,#26207,.F.);
#36646=ORIENTED_EDGE('',*,*,#24509,.F.);
#36647=ORIENTED_EDGE('',*,*,#26210,.T.);
#36648=ORIENTED_EDGE('',*,*,#23395,.T.);
#36649=ORIENTED_EDGE('',*,*,#26209,.F.);
#36650=ORIENTED_EDGE('',*,*,#24514,.F.);
#36651=ORIENTED_EDGE('',*,*,#26211,.T.);
#36652=ORIENTED_EDGE('',*,*,#23396,.T.);
#36653=ORIENTED_EDGE('',*,*,#26210,.F.);
#36654=ORIENTED_EDGE('',*,*,#24513,.F.);
#36655=ORIENTED_EDGE('',*,*,#26212,.T.);
#36656=ORIENTED_EDGE('',*,*,#23397,.T.);
#36657=ORIENTED_EDGE('',*,*,#26211,.F.);
#36658=ORIENTED_EDGE('',*,*,#24512,.F.);
#36659=ORIENTED_EDGE('',*,*,#26208,.T.);
#36660=ORIENTED_EDGE('',*,*,#23398,.T.);
#36661=ORIENTED_EDGE('',*,*,#26212,.F.);
#36662=ORIENTED_EDGE('',*,*,#24511,.F.);
#36663=ORIENTED_EDGE('',*,*,#26213,.T.);
#36664=ORIENTED_EDGE('',*,*,#23387,.T.);
#36665=ORIENTED_EDGE('',*,*,#26214,.F.);
#36666=ORIENTED_EDGE('',*,*,#24504,.F.);
#36667=ORIENTED_EDGE('',*,*,#26215,.T.);
#36668=ORIENTED_EDGE('',*,*,#23388,.T.);
#36669=ORIENTED_EDGE('',*,*,#26213,.F.);
#36670=ORIENTED_EDGE('',*,*,#24503,.F.);
#36671=ORIENTED_EDGE('',*,*,#26216,.T.);
#36672=ORIENTED_EDGE('',*,*,#23389,.T.);
#36673=ORIENTED_EDGE('',*,*,#26215,.F.);
#36674=ORIENTED_EDGE('',*,*,#24508,.F.);
#36675=ORIENTED_EDGE('',*,*,#26217,.T.);
#36676=ORIENTED_EDGE('',*,*,#23390,.T.);
#36677=ORIENTED_EDGE('',*,*,#26216,.F.);
#36678=ORIENTED_EDGE('',*,*,#24507,.F.);
#36679=ORIENTED_EDGE('',*,*,#26218,.T.);
#36680=ORIENTED_EDGE('',*,*,#23391,.T.);
#36681=ORIENTED_EDGE('',*,*,#26217,.F.);
#36682=ORIENTED_EDGE('',*,*,#24506,.F.);
#36683=ORIENTED_EDGE('',*,*,#26214,.T.);
#36684=ORIENTED_EDGE('',*,*,#23392,.T.);
#36685=ORIENTED_EDGE('',*,*,#26218,.F.);
#36686=ORIENTED_EDGE('',*,*,#24505,.F.);
#36687=ORIENTED_EDGE('',*,*,#26219,.T.);
#36688=ORIENTED_EDGE('',*,*,#23381,.T.);
#36689=ORIENTED_EDGE('',*,*,#26220,.F.);
#36690=ORIENTED_EDGE('',*,*,#24498,.F.);
#36691=ORIENTED_EDGE('',*,*,#26221,.T.);
#36692=ORIENTED_EDGE('',*,*,#23382,.T.);
#36693=ORIENTED_EDGE('',*,*,#26219,.F.);
#36694=ORIENTED_EDGE('',*,*,#24497,.F.);
#36695=ORIENTED_EDGE('',*,*,#26222,.T.);
#36696=ORIENTED_EDGE('',*,*,#23383,.T.);
#36697=ORIENTED_EDGE('',*,*,#26221,.F.);
#36698=ORIENTED_EDGE('',*,*,#24502,.F.);
#36699=ORIENTED_EDGE('',*,*,#26223,.T.);
#36700=ORIENTED_EDGE('',*,*,#23384,.T.);
#36701=ORIENTED_EDGE('',*,*,#26222,.F.);
#36702=ORIENTED_EDGE('',*,*,#24501,.F.);
#36703=ORIENTED_EDGE('',*,*,#26224,.T.);
#36704=ORIENTED_EDGE('',*,*,#23385,.T.);
#36705=ORIENTED_EDGE('',*,*,#26223,.F.);
#36706=ORIENTED_EDGE('',*,*,#24500,.F.);
#36707=ORIENTED_EDGE('',*,*,#26220,.T.);
#36708=ORIENTED_EDGE('',*,*,#23386,.T.);
#36709=ORIENTED_EDGE('',*,*,#26224,.F.);
#36710=ORIENTED_EDGE('',*,*,#24499,.F.);
#36711=ORIENTED_EDGE('',*,*,#26225,.T.);
#36712=ORIENTED_EDGE('',*,*,#23375,.T.);
#36713=ORIENTED_EDGE('',*,*,#26226,.F.);
#36714=ORIENTED_EDGE('',*,*,#24492,.F.);
#36715=ORIENTED_EDGE('',*,*,#26227,.T.);
#36716=ORIENTED_EDGE('',*,*,#23376,.T.);
#36717=ORIENTED_EDGE('',*,*,#26225,.F.);
#36718=ORIENTED_EDGE('',*,*,#24491,.F.);
#36719=ORIENTED_EDGE('',*,*,#26228,.T.);
#36720=ORIENTED_EDGE('',*,*,#23377,.T.);
#36721=ORIENTED_EDGE('',*,*,#26227,.F.);
#36722=ORIENTED_EDGE('',*,*,#24496,.F.);
#36723=ORIENTED_EDGE('',*,*,#26229,.T.);
#36724=ORIENTED_EDGE('',*,*,#23378,.T.);
#36725=ORIENTED_EDGE('',*,*,#26228,.F.);
#36726=ORIENTED_EDGE('',*,*,#24495,.F.);
#36727=ORIENTED_EDGE('',*,*,#26230,.T.);
#36728=ORIENTED_EDGE('',*,*,#23379,.T.);
#36729=ORIENTED_EDGE('',*,*,#26229,.F.);
#36730=ORIENTED_EDGE('',*,*,#24494,.F.);
#36731=ORIENTED_EDGE('',*,*,#26226,.T.);
#36732=ORIENTED_EDGE('',*,*,#23380,.T.);
#36733=ORIENTED_EDGE('',*,*,#26230,.F.);
#36734=ORIENTED_EDGE('',*,*,#24493,.F.);
#36735=ORIENTED_EDGE('',*,*,#26231,.T.);
#36736=ORIENTED_EDGE('',*,*,#23369,.T.);
#36737=ORIENTED_EDGE('',*,*,#26232,.F.);
#36738=ORIENTED_EDGE('',*,*,#24486,.F.);
#36739=ORIENTED_EDGE('',*,*,#26233,.T.);
#36740=ORIENTED_EDGE('',*,*,#23370,.T.);
#36741=ORIENTED_EDGE('',*,*,#26231,.F.);
#36742=ORIENTED_EDGE('',*,*,#24485,.F.);
#36743=ORIENTED_EDGE('',*,*,#26234,.T.);
#36744=ORIENTED_EDGE('',*,*,#23371,.T.);
#36745=ORIENTED_EDGE('',*,*,#26233,.F.);
#36746=ORIENTED_EDGE('',*,*,#24490,.F.);
#36747=ORIENTED_EDGE('',*,*,#26235,.T.);
#36748=ORIENTED_EDGE('',*,*,#23372,.T.);
#36749=ORIENTED_EDGE('',*,*,#26234,.F.);
#36750=ORIENTED_EDGE('',*,*,#24489,.F.);
#36751=ORIENTED_EDGE('',*,*,#26236,.T.);
#36752=ORIENTED_EDGE('',*,*,#23373,.T.);
#36753=ORIENTED_EDGE('',*,*,#26235,.F.);
#36754=ORIENTED_EDGE('',*,*,#24488,.F.);
#36755=ORIENTED_EDGE('',*,*,#26232,.T.);
#36756=ORIENTED_EDGE('',*,*,#23374,.T.);
#36757=ORIENTED_EDGE('',*,*,#26236,.F.);
#36758=ORIENTED_EDGE('',*,*,#24487,.F.);
#36759=ORIENTED_EDGE('',*,*,#26237,.T.);
#36760=ORIENTED_EDGE('',*,*,#23363,.T.);
#36761=ORIENTED_EDGE('',*,*,#26238,.F.);
#36762=ORIENTED_EDGE('',*,*,#24480,.F.);
#36763=ORIENTED_EDGE('',*,*,#26239,.T.);
#36764=ORIENTED_EDGE('',*,*,#23364,.T.);
#36765=ORIENTED_EDGE('',*,*,#26237,.F.);
#36766=ORIENTED_EDGE('',*,*,#24479,.F.);
#36767=ORIENTED_EDGE('',*,*,#26240,.T.);
#36768=ORIENTED_EDGE('',*,*,#23365,.T.);
#36769=ORIENTED_EDGE('',*,*,#26239,.F.);
#36770=ORIENTED_EDGE('',*,*,#24484,.F.);
#36771=ORIENTED_EDGE('',*,*,#26241,.T.);
#36772=ORIENTED_EDGE('',*,*,#23366,.T.);
#36773=ORIENTED_EDGE('',*,*,#26240,.F.);
#36774=ORIENTED_EDGE('',*,*,#24483,.F.);
#36775=ORIENTED_EDGE('',*,*,#26242,.T.);
#36776=ORIENTED_EDGE('',*,*,#23367,.T.);
#36777=ORIENTED_EDGE('',*,*,#26241,.F.);
#36778=ORIENTED_EDGE('',*,*,#24482,.F.);
#36779=ORIENTED_EDGE('',*,*,#26238,.T.);
#36780=ORIENTED_EDGE('',*,*,#23368,.T.);
#36781=ORIENTED_EDGE('',*,*,#26242,.F.);
#36782=ORIENTED_EDGE('',*,*,#24481,.F.);
#36783=ORIENTED_EDGE('',*,*,#26243,.T.);
#36784=ORIENTED_EDGE('',*,*,#23357,.T.);
#36785=ORIENTED_EDGE('',*,*,#26244,.F.);
#36786=ORIENTED_EDGE('',*,*,#24474,.F.);
#36787=ORIENTED_EDGE('',*,*,#26245,.T.);
#36788=ORIENTED_EDGE('',*,*,#23358,.T.);
#36789=ORIENTED_EDGE('',*,*,#26243,.F.);
#36790=ORIENTED_EDGE('',*,*,#24473,.F.);
#36791=ORIENTED_EDGE('',*,*,#26246,.T.);
#36792=ORIENTED_EDGE('',*,*,#23359,.T.);
#36793=ORIENTED_EDGE('',*,*,#26245,.F.);
#36794=ORIENTED_EDGE('',*,*,#24478,.F.);
#36795=ORIENTED_EDGE('',*,*,#26247,.T.);
#36796=ORIENTED_EDGE('',*,*,#23360,.T.);
#36797=ORIENTED_EDGE('',*,*,#26246,.F.);
#36798=ORIENTED_EDGE('',*,*,#24477,.F.);
#36799=ORIENTED_EDGE('',*,*,#26248,.T.);
#36800=ORIENTED_EDGE('',*,*,#23361,.T.);
#36801=ORIENTED_EDGE('',*,*,#26247,.F.);
#36802=ORIENTED_EDGE('',*,*,#24476,.F.);
#36803=ORIENTED_EDGE('',*,*,#26244,.T.);
#36804=ORIENTED_EDGE('',*,*,#23362,.T.);
#36805=ORIENTED_EDGE('',*,*,#26248,.F.);
#36806=ORIENTED_EDGE('',*,*,#24475,.F.);
#36807=ORIENTED_EDGE('',*,*,#26249,.T.);
#36808=ORIENTED_EDGE('',*,*,#23351,.T.);
#36809=ORIENTED_EDGE('',*,*,#26250,.F.);
#36810=ORIENTED_EDGE('',*,*,#24468,.F.);
#36811=ORIENTED_EDGE('',*,*,#26251,.T.);
#36812=ORIENTED_EDGE('',*,*,#23352,.T.);
#36813=ORIENTED_EDGE('',*,*,#26249,.F.);
#36814=ORIENTED_EDGE('',*,*,#24467,.F.);
#36815=ORIENTED_EDGE('',*,*,#26252,.T.);
#36816=ORIENTED_EDGE('',*,*,#23353,.T.);
#36817=ORIENTED_EDGE('',*,*,#26251,.F.);
#36818=ORIENTED_EDGE('',*,*,#24472,.F.);
#36819=ORIENTED_EDGE('',*,*,#26253,.T.);
#36820=ORIENTED_EDGE('',*,*,#23354,.T.);
#36821=ORIENTED_EDGE('',*,*,#26252,.F.);
#36822=ORIENTED_EDGE('',*,*,#24471,.F.);
#36823=ORIENTED_EDGE('',*,*,#26254,.T.);
#36824=ORIENTED_EDGE('',*,*,#23355,.T.);
#36825=ORIENTED_EDGE('',*,*,#26253,.F.);
#36826=ORIENTED_EDGE('',*,*,#24470,.F.);
#36827=ORIENTED_EDGE('',*,*,#26250,.T.);
#36828=ORIENTED_EDGE('',*,*,#23356,.T.);
#36829=ORIENTED_EDGE('',*,*,#26254,.F.);
#36830=ORIENTED_EDGE('',*,*,#24469,.F.);
#36831=ORIENTED_EDGE('',*,*,#26255,.T.);
#36832=ORIENTED_EDGE('',*,*,#23345,.T.);
#36833=ORIENTED_EDGE('',*,*,#26256,.F.);
#36834=ORIENTED_EDGE('',*,*,#24462,.F.);
#36835=ORIENTED_EDGE('',*,*,#26257,.T.);
#36836=ORIENTED_EDGE('',*,*,#23346,.T.);
#36837=ORIENTED_EDGE('',*,*,#26255,.F.);
#36838=ORIENTED_EDGE('',*,*,#24461,.F.);
#36839=ORIENTED_EDGE('',*,*,#26258,.T.);
#36840=ORIENTED_EDGE('',*,*,#23347,.T.);
#36841=ORIENTED_EDGE('',*,*,#26257,.F.);
#36842=ORIENTED_EDGE('',*,*,#24466,.F.);
#36843=ORIENTED_EDGE('',*,*,#26259,.T.);
#36844=ORIENTED_EDGE('',*,*,#23348,.T.);
#36845=ORIENTED_EDGE('',*,*,#26258,.F.);
#36846=ORIENTED_EDGE('',*,*,#24465,.F.);
#36847=ORIENTED_EDGE('',*,*,#26260,.T.);
#36848=ORIENTED_EDGE('',*,*,#23349,.T.);
#36849=ORIENTED_EDGE('',*,*,#26259,.F.);
#36850=ORIENTED_EDGE('',*,*,#24464,.F.);
#36851=ORIENTED_EDGE('',*,*,#26256,.T.);
#36852=ORIENTED_EDGE('',*,*,#23350,.T.);
#36853=ORIENTED_EDGE('',*,*,#26260,.F.);
#36854=ORIENTED_EDGE('',*,*,#24463,.F.);
#36855=ORIENTED_EDGE('',*,*,#26261,.T.);
#36856=ORIENTED_EDGE('',*,*,#23339,.T.);
#36857=ORIENTED_EDGE('',*,*,#26262,.F.);
#36858=ORIENTED_EDGE('',*,*,#24456,.F.);
#36859=ORIENTED_EDGE('',*,*,#26263,.T.);
#36860=ORIENTED_EDGE('',*,*,#23340,.T.);
#36861=ORIENTED_EDGE('',*,*,#26261,.F.);
#36862=ORIENTED_EDGE('',*,*,#24455,.F.);
#36863=ORIENTED_EDGE('',*,*,#26264,.T.);
#36864=ORIENTED_EDGE('',*,*,#23341,.T.);
#36865=ORIENTED_EDGE('',*,*,#26263,.F.);
#36866=ORIENTED_EDGE('',*,*,#24460,.F.);
#36867=ORIENTED_EDGE('',*,*,#26265,.T.);
#36868=ORIENTED_EDGE('',*,*,#23342,.T.);
#36869=ORIENTED_EDGE('',*,*,#26264,.F.);
#36870=ORIENTED_EDGE('',*,*,#24459,.F.);
#36871=ORIENTED_EDGE('',*,*,#26266,.T.);
#36872=ORIENTED_EDGE('',*,*,#23343,.T.);
#36873=ORIENTED_EDGE('',*,*,#26265,.F.);
#36874=ORIENTED_EDGE('',*,*,#24458,.F.);
#36875=ORIENTED_EDGE('',*,*,#26262,.T.);
#36876=ORIENTED_EDGE('',*,*,#23344,.T.);
#36877=ORIENTED_EDGE('',*,*,#26266,.F.);
#36878=ORIENTED_EDGE('',*,*,#24457,.F.);
#36879=ORIENTED_EDGE('',*,*,#26267,.T.);
#36880=ORIENTED_EDGE('',*,*,#23333,.T.);
#36881=ORIENTED_EDGE('',*,*,#26268,.F.);
#36882=ORIENTED_EDGE('',*,*,#24450,.F.);
#36883=ORIENTED_EDGE('',*,*,#26269,.T.);
#36884=ORIENTED_EDGE('',*,*,#23334,.T.);
#36885=ORIENTED_EDGE('',*,*,#26267,.F.);
#36886=ORIENTED_EDGE('',*,*,#24449,.F.);
#36887=ORIENTED_EDGE('',*,*,#26270,.T.);
#36888=ORIENTED_EDGE('',*,*,#23335,.T.);
#36889=ORIENTED_EDGE('',*,*,#26269,.F.);
#36890=ORIENTED_EDGE('',*,*,#24454,.F.);
#36891=ORIENTED_EDGE('',*,*,#26271,.T.);
#36892=ORIENTED_EDGE('',*,*,#23336,.T.);
#36893=ORIENTED_EDGE('',*,*,#26270,.F.);
#36894=ORIENTED_EDGE('',*,*,#24453,.F.);
#36895=ORIENTED_EDGE('',*,*,#26272,.T.);
#36896=ORIENTED_EDGE('',*,*,#23337,.T.);
#36897=ORIENTED_EDGE('',*,*,#26271,.F.);
#36898=ORIENTED_EDGE('',*,*,#24452,.F.);
#36899=ORIENTED_EDGE('',*,*,#26268,.T.);
#36900=ORIENTED_EDGE('',*,*,#23338,.T.);
#36901=ORIENTED_EDGE('',*,*,#26272,.F.);
#36902=ORIENTED_EDGE('',*,*,#24451,.F.);
#36903=ORIENTED_EDGE('',*,*,#26273,.T.);
#36904=ORIENTED_EDGE('',*,*,#23327,.T.);
#36905=ORIENTED_EDGE('',*,*,#26274,.F.);
#36906=ORIENTED_EDGE('',*,*,#24444,.F.);
#36907=ORIENTED_EDGE('',*,*,#26275,.T.);
#36908=ORIENTED_EDGE('',*,*,#23328,.T.);
#36909=ORIENTED_EDGE('',*,*,#26273,.F.);
#36910=ORIENTED_EDGE('',*,*,#24443,.F.);
#36911=ORIENTED_EDGE('',*,*,#26276,.T.);
#36912=ORIENTED_EDGE('',*,*,#23329,.T.);
#36913=ORIENTED_EDGE('',*,*,#26275,.F.);
#36914=ORIENTED_EDGE('',*,*,#24448,.F.);
#36915=ORIENTED_EDGE('',*,*,#26277,.T.);
#36916=ORIENTED_EDGE('',*,*,#23330,.T.);
#36917=ORIENTED_EDGE('',*,*,#26276,.F.);
#36918=ORIENTED_EDGE('',*,*,#24447,.F.);
#36919=ORIENTED_EDGE('',*,*,#26278,.T.);
#36920=ORIENTED_EDGE('',*,*,#23331,.T.);
#36921=ORIENTED_EDGE('',*,*,#26277,.F.);
#36922=ORIENTED_EDGE('',*,*,#24446,.F.);
#36923=ORIENTED_EDGE('',*,*,#26274,.T.);
#36924=ORIENTED_EDGE('',*,*,#23332,.T.);
#36925=ORIENTED_EDGE('',*,*,#26278,.F.);
#36926=ORIENTED_EDGE('',*,*,#24445,.F.);
#36927=ORIENTED_EDGE('',*,*,#26279,.T.);
#36928=ORIENTED_EDGE('',*,*,#23321,.T.);
#36929=ORIENTED_EDGE('',*,*,#26280,.F.);
#36930=ORIENTED_EDGE('',*,*,#24438,.F.);
#36931=ORIENTED_EDGE('',*,*,#26281,.T.);
#36932=ORIENTED_EDGE('',*,*,#23322,.T.);
#36933=ORIENTED_EDGE('',*,*,#26279,.F.);
#36934=ORIENTED_EDGE('',*,*,#24437,.F.);
#36935=ORIENTED_EDGE('',*,*,#26282,.T.);
#36936=ORIENTED_EDGE('',*,*,#23323,.T.);
#36937=ORIENTED_EDGE('',*,*,#26281,.F.);
#36938=ORIENTED_EDGE('',*,*,#24442,.F.);
#36939=ORIENTED_EDGE('',*,*,#26283,.T.);
#36940=ORIENTED_EDGE('',*,*,#23324,.T.);
#36941=ORIENTED_EDGE('',*,*,#26282,.F.);
#36942=ORIENTED_EDGE('',*,*,#24441,.F.);
#36943=ORIENTED_EDGE('',*,*,#26284,.T.);
#36944=ORIENTED_EDGE('',*,*,#23325,.T.);
#36945=ORIENTED_EDGE('',*,*,#26283,.F.);
#36946=ORIENTED_EDGE('',*,*,#24440,.F.);
#36947=ORIENTED_EDGE('',*,*,#26280,.T.);
#36948=ORIENTED_EDGE('',*,*,#23326,.T.);
#36949=ORIENTED_EDGE('',*,*,#26284,.F.);
#36950=ORIENTED_EDGE('',*,*,#24439,.F.);
#36951=ORIENTED_EDGE('',*,*,#26285,.T.);
#36952=ORIENTED_EDGE('',*,*,#23315,.T.);
#36953=ORIENTED_EDGE('',*,*,#26286,.F.);
#36954=ORIENTED_EDGE('',*,*,#24432,.F.);
#36955=ORIENTED_EDGE('',*,*,#26287,.T.);
#36956=ORIENTED_EDGE('',*,*,#23316,.T.);
#36957=ORIENTED_EDGE('',*,*,#26285,.F.);
#36958=ORIENTED_EDGE('',*,*,#24431,.F.);
#36959=ORIENTED_EDGE('',*,*,#26288,.T.);
#36960=ORIENTED_EDGE('',*,*,#23317,.T.);
#36961=ORIENTED_EDGE('',*,*,#26287,.F.);
#36962=ORIENTED_EDGE('',*,*,#24436,.F.);
#36963=ORIENTED_EDGE('',*,*,#26289,.T.);
#36964=ORIENTED_EDGE('',*,*,#23318,.T.);
#36965=ORIENTED_EDGE('',*,*,#26288,.F.);
#36966=ORIENTED_EDGE('',*,*,#24435,.F.);
#36967=ORIENTED_EDGE('',*,*,#26290,.T.);
#36968=ORIENTED_EDGE('',*,*,#23319,.T.);
#36969=ORIENTED_EDGE('',*,*,#26289,.F.);
#36970=ORIENTED_EDGE('',*,*,#24434,.F.);
#36971=ORIENTED_EDGE('',*,*,#26286,.T.);
#36972=ORIENTED_EDGE('',*,*,#23320,.T.);
#36973=ORIENTED_EDGE('',*,*,#26290,.F.);
#36974=ORIENTED_EDGE('',*,*,#24433,.F.);
#36975=ORIENTED_EDGE('',*,*,#26291,.T.);
#36976=ORIENTED_EDGE('',*,*,#23309,.T.);
#36977=ORIENTED_EDGE('',*,*,#26292,.F.);
#36978=ORIENTED_EDGE('',*,*,#24426,.F.);
#36979=ORIENTED_EDGE('',*,*,#26293,.T.);
#36980=ORIENTED_EDGE('',*,*,#23310,.T.);
#36981=ORIENTED_EDGE('',*,*,#26291,.F.);
#36982=ORIENTED_EDGE('',*,*,#24425,.F.);
#36983=ORIENTED_EDGE('',*,*,#26294,.T.);
#36984=ORIENTED_EDGE('',*,*,#23311,.T.);
#36985=ORIENTED_EDGE('',*,*,#26293,.F.);
#36986=ORIENTED_EDGE('',*,*,#24430,.F.);
#36987=ORIENTED_EDGE('',*,*,#26295,.T.);
#36988=ORIENTED_EDGE('',*,*,#23312,.T.);
#36989=ORIENTED_EDGE('',*,*,#26294,.F.);
#36990=ORIENTED_EDGE('',*,*,#24429,.F.);
#36991=ORIENTED_EDGE('',*,*,#26296,.T.);
#36992=ORIENTED_EDGE('',*,*,#23313,.T.);
#36993=ORIENTED_EDGE('',*,*,#26295,.F.);
#36994=ORIENTED_EDGE('',*,*,#24428,.F.);
#36995=ORIENTED_EDGE('',*,*,#26292,.T.);
#36996=ORIENTED_EDGE('',*,*,#23314,.T.);
#36997=ORIENTED_EDGE('',*,*,#26296,.F.);
#36998=ORIENTED_EDGE('',*,*,#24427,.F.);
#36999=ORIENTED_EDGE('',*,*,#26297,.T.);
#37000=ORIENTED_EDGE('',*,*,#23303,.T.);
#37001=ORIENTED_EDGE('',*,*,#26298,.F.);
#37002=ORIENTED_EDGE('',*,*,#24420,.F.);
#37003=ORIENTED_EDGE('',*,*,#26299,.T.);
#37004=ORIENTED_EDGE('',*,*,#23304,.T.);
#37005=ORIENTED_EDGE('',*,*,#26297,.F.);
#37006=ORIENTED_EDGE('',*,*,#24419,.F.);
#37007=ORIENTED_EDGE('',*,*,#26300,.T.);
#37008=ORIENTED_EDGE('',*,*,#23305,.T.);
#37009=ORIENTED_EDGE('',*,*,#26299,.F.);
#37010=ORIENTED_EDGE('',*,*,#24424,.F.);
#37011=ORIENTED_EDGE('',*,*,#26301,.T.);
#37012=ORIENTED_EDGE('',*,*,#23306,.T.);
#37013=ORIENTED_EDGE('',*,*,#26300,.F.);
#37014=ORIENTED_EDGE('',*,*,#24423,.F.);
#37015=ORIENTED_EDGE('',*,*,#26302,.T.);
#37016=ORIENTED_EDGE('',*,*,#23307,.T.);
#37017=ORIENTED_EDGE('',*,*,#26301,.F.);
#37018=ORIENTED_EDGE('',*,*,#24422,.F.);
#37019=ORIENTED_EDGE('',*,*,#26298,.T.);
#37020=ORIENTED_EDGE('',*,*,#23308,.T.);
#37021=ORIENTED_EDGE('',*,*,#26302,.F.);
#37022=ORIENTED_EDGE('',*,*,#24421,.F.);
#37023=ORIENTED_EDGE('',*,*,#26303,.T.);
#37024=ORIENTED_EDGE('',*,*,#23297,.T.);
#37025=ORIENTED_EDGE('',*,*,#26304,.F.);
#37026=ORIENTED_EDGE('',*,*,#24414,.F.);
#37027=ORIENTED_EDGE('',*,*,#26305,.T.);
#37028=ORIENTED_EDGE('',*,*,#23298,.T.);
#37029=ORIENTED_EDGE('',*,*,#26303,.F.);
#37030=ORIENTED_EDGE('',*,*,#24413,.F.);
#37031=ORIENTED_EDGE('',*,*,#26306,.T.);
#37032=ORIENTED_EDGE('',*,*,#23299,.T.);
#37033=ORIENTED_EDGE('',*,*,#26305,.F.);
#37034=ORIENTED_EDGE('',*,*,#24418,.F.);
#37035=ORIENTED_EDGE('',*,*,#26307,.T.);
#37036=ORIENTED_EDGE('',*,*,#23300,.T.);
#37037=ORIENTED_EDGE('',*,*,#26306,.F.);
#37038=ORIENTED_EDGE('',*,*,#24417,.F.);
#37039=ORIENTED_EDGE('',*,*,#26308,.T.);
#37040=ORIENTED_EDGE('',*,*,#23301,.T.);
#37041=ORIENTED_EDGE('',*,*,#26307,.F.);
#37042=ORIENTED_EDGE('',*,*,#24416,.F.);
#37043=ORIENTED_EDGE('',*,*,#26304,.T.);
#37044=ORIENTED_EDGE('',*,*,#23302,.T.);
#37045=ORIENTED_EDGE('',*,*,#26308,.F.);
#37046=ORIENTED_EDGE('',*,*,#24415,.F.);
#37047=ORIENTED_EDGE('',*,*,#26309,.T.);
#37048=ORIENTED_EDGE('',*,*,#23291,.T.);
#37049=ORIENTED_EDGE('',*,*,#26310,.F.);
#37050=ORIENTED_EDGE('',*,*,#24408,.F.);
#37051=ORIENTED_EDGE('',*,*,#26311,.T.);
#37052=ORIENTED_EDGE('',*,*,#23292,.T.);
#37053=ORIENTED_EDGE('',*,*,#26309,.F.);
#37054=ORIENTED_EDGE('',*,*,#24407,.F.);
#37055=ORIENTED_EDGE('',*,*,#26312,.T.);
#37056=ORIENTED_EDGE('',*,*,#23293,.T.);
#37057=ORIENTED_EDGE('',*,*,#26311,.F.);
#37058=ORIENTED_EDGE('',*,*,#24412,.F.);
#37059=ORIENTED_EDGE('',*,*,#26313,.T.);
#37060=ORIENTED_EDGE('',*,*,#23294,.T.);
#37061=ORIENTED_EDGE('',*,*,#26312,.F.);
#37062=ORIENTED_EDGE('',*,*,#24411,.F.);
#37063=ORIENTED_EDGE('',*,*,#26314,.T.);
#37064=ORIENTED_EDGE('',*,*,#23295,.T.);
#37065=ORIENTED_EDGE('',*,*,#26313,.F.);
#37066=ORIENTED_EDGE('',*,*,#24410,.F.);
#37067=ORIENTED_EDGE('',*,*,#26310,.T.);
#37068=ORIENTED_EDGE('',*,*,#23296,.T.);
#37069=ORIENTED_EDGE('',*,*,#26314,.F.);
#37070=ORIENTED_EDGE('',*,*,#24409,.F.);
#37071=ORIENTED_EDGE('',*,*,#26315,.T.);
#37072=ORIENTED_EDGE('',*,*,#23285,.T.);
#37073=ORIENTED_EDGE('',*,*,#26316,.F.);
#37074=ORIENTED_EDGE('',*,*,#24402,.F.);
#37075=ORIENTED_EDGE('',*,*,#26317,.T.);
#37076=ORIENTED_EDGE('',*,*,#23286,.T.);
#37077=ORIENTED_EDGE('',*,*,#26315,.F.);
#37078=ORIENTED_EDGE('',*,*,#24401,.F.);
#37079=ORIENTED_EDGE('',*,*,#26318,.T.);
#37080=ORIENTED_EDGE('',*,*,#23287,.T.);
#37081=ORIENTED_EDGE('',*,*,#26317,.F.);
#37082=ORIENTED_EDGE('',*,*,#24406,.F.);
#37083=ORIENTED_EDGE('',*,*,#26319,.T.);
#37084=ORIENTED_EDGE('',*,*,#23288,.T.);
#37085=ORIENTED_EDGE('',*,*,#26318,.F.);
#37086=ORIENTED_EDGE('',*,*,#24405,.F.);
#37087=ORIENTED_EDGE('',*,*,#26320,.T.);
#37088=ORIENTED_EDGE('',*,*,#23289,.T.);
#37089=ORIENTED_EDGE('',*,*,#26319,.F.);
#37090=ORIENTED_EDGE('',*,*,#24404,.F.);
#37091=ORIENTED_EDGE('',*,*,#26316,.T.);
#37092=ORIENTED_EDGE('',*,*,#23290,.T.);
#37093=ORIENTED_EDGE('',*,*,#26320,.F.);
#37094=ORIENTED_EDGE('',*,*,#24403,.F.);
#37095=ORIENTED_EDGE('',*,*,#26321,.T.);
#37096=ORIENTED_EDGE('',*,*,#23279,.T.);
#37097=ORIENTED_EDGE('',*,*,#26322,.F.);
#37098=ORIENTED_EDGE('',*,*,#24396,.F.);
#37099=ORIENTED_EDGE('',*,*,#26323,.T.);
#37100=ORIENTED_EDGE('',*,*,#23280,.T.);
#37101=ORIENTED_EDGE('',*,*,#26321,.F.);
#37102=ORIENTED_EDGE('',*,*,#24395,.F.);
#37103=ORIENTED_EDGE('',*,*,#26324,.T.);
#37104=ORIENTED_EDGE('',*,*,#23281,.T.);
#37105=ORIENTED_EDGE('',*,*,#26323,.F.);
#37106=ORIENTED_EDGE('',*,*,#24400,.F.);
#37107=ORIENTED_EDGE('',*,*,#26325,.T.);
#37108=ORIENTED_EDGE('',*,*,#23282,.T.);
#37109=ORIENTED_EDGE('',*,*,#26324,.F.);
#37110=ORIENTED_EDGE('',*,*,#24399,.F.);
#37111=ORIENTED_EDGE('',*,*,#26326,.T.);
#37112=ORIENTED_EDGE('',*,*,#23283,.T.);
#37113=ORIENTED_EDGE('',*,*,#26325,.F.);
#37114=ORIENTED_EDGE('',*,*,#24398,.F.);
#37115=ORIENTED_EDGE('',*,*,#26322,.T.);
#37116=ORIENTED_EDGE('',*,*,#23284,.T.);
#37117=ORIENTED_EDGE('',*,*,#26326,.F.);
#37118=ORIENTED_EDGE('',*,*,#24397,.F.);
#37119=ORIENTED_EDGE('',*,*,#26327,.T.);
#37120=ORIENTED_EDGE('',*,*,#23273,.T.);
#37121=ORIENTED_EDGE('',*,*,#26328,.F.);
#37122=ORIENTED_EDGE('',*,*,#24390,.F.);
#37123=ORIENTED_EDGE('',*,*,#26329,.T.);
#37124=ORIENTED_EDGE('',*,*,#23274,.T.);
#37125=ORIENTED_EDGE('',*,*,#26327,.F.);
#37126=ORIENTED_EDGE('',*,*,#24389,.F.);
#37127=ORIENTED_EDGE('',*,*,#26330,.T.);
#37128=ORIENTED_EDGE('',*,*,#23275,.T.);
#37129=ORIENTED_EDGE('',*,*,#26329,.F.);
#37130=ORIENTED_EDGE('',*,*,#24394,.F.);
#37131=ORIENTED_EDGE('',*,*,#26331,.T.);
#37132=ORIENTED_EDGE('',*,*,#23276,.T.);
#37133=ORIENTED_EDGE('',*,*,#26330,.F.);
#37134=ORIENTED_EDGE('',*,*,#24393,.F.);
#37135=ORIENTED_EDGE('',*,*,#26332,.T.);
#37136=ORIENTED_EDGE('',*,*,#23277,.T.);
#37137=ORIENTED_EDGE('',*,*,#26331,.F.);
#37138=ORIENTED_EDGE('',*,*,#24392,.F.);
#37139=ORIENTED_EDGE('',*,*,#26328,.T.);
#37140=ORIENTED_EDGE('',*,*,#23278,.T.);
#37141=ORIENTED_EDGE('',*,*,#26332,.F.);
#37142=ORIENTED_EDGE('',*,*,#24391,.F.);
#37143=ORIENTED_EDGE('',*,*,#26333,.T.);
#37144=ORIENTED_EDGE('',*,*,#23267,.T.);
#37145=ORIENTED_EDGE('',*,*,#26334,.F.);
#37146=ORIENTED_EDGE('',*,*,#24384,.F.);
#37147=ORIENTED_EDGE('',*,*,#26335,.T.);
#37148=ORIENTED_EDGE('',*,*,#23268,.T.);
#37149=ORIENTED_EDGE('',*,*,#26333,.F.);
#37150=ORIENTED_EDGE('',*,*,#24383,.F.);
#37151=ORIENTED_EDGE('',*,*,#26336,.T.);
#37152=ORIENTED_EDGE('',*,*,#23269,.T.);
#37153=ORIENTED_EDGE('',*,*,#26335,.F.);
#37154=ORIENTED_EDGE('',*,*,#24388,.F.);
#37155=ORIENTED_EDGE('',*,*,#26337,.T.);
#37156=ORIENTED_EDGE('',*,*,#23270,.T.);
#37157=ORIENTED_EDGE('',*,*,#26336,.F.);
#37158=ORIENTED_EDGE('',*,*,#24387,.F.);
#37159=ORIENTED_EDGE('',*,*,#26338,.T.);
#37160=ORIENTED_EDGE('',*,*,#23271,.T.);
#37161=ORIENTED_EDGE('',*,*,#26337,.F.);
#37162=ORIENTED_EDGE('',*,*,#24386,.F.);
#37163=ORIENTED_EDGE('',*,*,#26334,.T.);
#37164=ORIENTED_EDGE('',*,*,#23272,.T.);
#37165=ORIENTED_EDGE('',*,*,#26338,.F.);
#37166=ORIENTED_EDGE('',*,*,#24385,.F.);
#37167=ORIENTED_EDGE('',*,*,#26339,.T.);
#37168=ORIENTED_EDGE('',*,*,#23261,.T.);
#37169=ORIENTED_EDGE('',*,*,#26340,.F.);
#37170=ORIENTED_EDGE('',*,*,#24378,.F.);
#37171=ORIENTED_EDGE('',*,*,#26341,.T.);
#37172=ORIENTED_EDGE('',*,*,#23262,.T.);
#37173=ORIENTED_EDGE('',*,*,#26339,.F.);
#37174=ORIENTED_EDGE('',*,*,#24377,.F.);
#37175=ORIENTED_EDGE('',*,*,#26342,.T.);
#37176=ORIENTED_EDGE('',*,*,#23263,.T.);
#37177=ORIENTED_EDGE('',*,*,#26341,.F.);
#37178=ORIENTED_EDGE('',*,*,#24382,.F.);
#37179=ORIENTED_EDGE('',*,*,#26343,.T.);
#37180=ORIENTED_EDGE('',*,*,#23264,.T.);
#37181=ORIENTED_EDGE('',*,*,#26342,.F.);
#37182=ORIENTED_EDGE('',*,*,#24381,.F.);
#37183=ORIENTED_EDGE('',*,*,#26344,.T.);
#37184=ORIENTED_EDGE('',*,*,#23265,.T.);
#37185=ORIENTED_EDGE('',*,*,#26343,.F.);
#37186=ORIENTED_EDGE('',*,*,#24380,.F.);
#37187=ORIENTED_EDGE('',*,*,#26340,.T.);
#37188=ORIENTED_EDGE('',*,*,#23266,.T.);
#37189=ORIENTED_EDGE('',*,*,#26344,.F.);
#37190=ORIENTED_EDGE('',*,*,#24379,.F.);
#37191=ORIENTED_EDGE('',*,*,#26345,.T.);
#37192=ORIENTED_EDGE('',*,*,#23255,.T.);
#37193=ORIENTED_EDGE('',*,*,#26346,.F.);
#37194=ORIENTED_EDGE('',*,*,#24372,.F.);
#37195=ORIENTED_EDGE('',*,*,#26347,.T.);
#37196=ORIENTED_EDGE('',*,*,#23256,.T.);
#37197=ORIENTED_EDGE('',*,*,#26345,.F.);
#37198=ORIENTED_EDGE('',*,*,#24371,.F.);
#37199=ORIENTED_EDGE('',*,*,#26348,.T.);
#37200=ORIENTED_EDGE('',*,*,#23257,.T.);
#37201=ORIENTED_EDGE('',*,*,#26347,.F.);
#37202=ORIENTED_EDGE('',*,*,#24376,.F.);
#37203=ORIENTED_EDGE('',*,*,#26349,.T.);
#37204=ORIENTED_EDGE('',*,*,#23258,.T.);
#37205=ORIENTED_EDGE('',*,*,#26348,.F.);
#37206=ORIENTED_EDGE('',*,*,#24375,.F.);
#37207=ORIENTED_EDGE('',*,*,#26350,.T.);
#37208=ORIENTED_EDGE('',*,*,#23259,.T.);
#37209=ORIENTED_EDGE('',*,*,#26349,.F.);
#37210=ORIENTED_EDGE('',*,*,#24374,.F.);
#37211=ORIENTED_EDGE('',*,*,#26346,.T.);
#37212=ORIENTED_EDGE('',*,*,#23260,.T.);
#37213=ORIENTED_EDGE('',*,*,#26350,.F.);
#37214=ORIENTED_EDGE('',*,*,#24373,.F.);
#37215=ORIENTED_EDGE('',*,*,#26351,.T.);
#37216=ORIENTED_EDGE('',*,*,#23249,.T.);
#37217=ORIENTED_EDGE('',*,*,#26352,.F.);
#37218=ORIENTED_EDGE('',*,*,#24366,.F.);
#37219=ORIENTED_EDGE('',*,*,#26353,.T.);
#37220=ORIENTED_EDGE('',*,*,#23250,.T.);
#37221=ORIENTED_EDGE('',*,*,#26351,.F.);
#37222=ORIENTED_EDGE('',*,*,#24365,.F.);
#37223=ORIENTED_EDGE('',*,*,#26354,.T.);
#37224=ORIENTED_EDGE('',*,*,#23251,.T.);
#37225=ORIENTED_EDGE('',*,*,#26353,.F.);
#37226=ORIENTED_EDGE('',*,*,#24370,.F.);
#37227=ORIENTED_EDGE('',*,*,#26355,.T.);
#37228=ORIENTED_EDGE('',*,*,#23252,.T.);
#37229=ORIENTED_EDGE('',*,*,#26354,.F.);
#37230=ORIENTED_EDGE('',*,*,#24369,.F.);
#37231=ORIENTED_EDGE('',*,*,#26356,.T.);
#37232=ORIENTED_EDGE('',*,*,#23253,.T.);
#37233=ORIENTED_EDGE('',*,*,#26355,.F.);
#37234=ORIENTED_EDGE('',*,*,#24368,.F.);
#37235=ORIENTED_EDGE('',*,*,#26352,.T.);
#37236=ORIENTED_EDGE('',*,*,#23254,.T.);
#37237=ORIENTED_EDGE('',*,*,#26356,.F.);
#37238=ORIENTED_EDGE('',*,*,#24367,.F.);
#37239=ORIENTED_EDGE('',*,*,#26357,.T.);
#37240=ORIENTED_EDGE('',*,*,#23243,.T.);
#37241=ORIENTED_EDGE('',*,*,#26358,.F.);
#37242=ORIENTED_EDGE('',*,*,#24360,.F.);
#37243=ORIENTED_EDGE('',*,*,#26359,.T.);
#37244=ORIENTED_EDGE('',*,*,#23244,.T.);
#37245=ORIENTED_EDGE('',*,*,#26357,.F.);
#37246=ORIENTED_EDGE('',*,*,#24359,.F.);
#37247=ORIENTED_EDGE('',*,*,#26360,.T.);
#37248=ORIENTED_EDGE('',*,*,#23245,.T.);
#37249=ORIENTED_EDGE('',*,*,#26359,.F.);
#37250=ORIENTED_EDGE('',*,*,#24364,.F.);
#37251=ORIENTED_EDGE('',*,*,#26361,.T.);
#37252=ORIENTED_EDGE('',*,*,#23246,.T.);
#37253=ORIENTED_EDGE('',*,*,#26360,.F.);
#37254=ORIENTED_EDGE('',*,*,#24363,.F.);
#37255=ORIENTED_EDGE('',*,*,#26362,.T.);
#37256=ORIENTED_EDGE('',*,*,#23247,.T.);
#37257=ORIENTED_EDGE('',*,*,#26361,.F.);
#37258=ORIENTED_EDGE('',*,*,#24362,.F.);
#37259=ORIENTED_EDGE('',*,*,#26358,.T.);
#37260=ORIENTED_EDGE('',*,*,#23248,.T.);
#37261=ORIENTED_EDGE('',*,*,#26362,.F.);
#37262=ORIENTED_EDGE('',*,*,#24361,.F.);
#37263=ORIENTED_EDGE('',*,*,#26363,.T.);
#37264=ORIENTED_EDGE('',*,*,#23237,.T.);
#37265=ORIENTED_EDGE('',*,*,#26364,.F.);
#37266=ORIENTED_EDGE('',*,*,#24354,.F.);
#37267=ORIENTED_EDGE('',*,*,#26365,.T.);
#37268=ORIENTED_EDGE('',*,*,#23238,.T.);
#37269=ORIENTED_EDGE('',*,*,#26363,.F.);
#37270=ORIENTED_EDGE('',*,*,#24353,.F.);
#37271=ORIENTED_EDGE('',*,*,#26366,.T.);
#37272=ORIENTED_EDGE('',*,*,#23239,.T.);
#37273=ORIENTED_EDGE('',*,*,#26365,.F.);
#37274=ORIENTED_EDGE('',*,*,#24358,.F.);
#37275=ORIENTED_EDGE('',*,*,#26367,.T.);
#37276=ORIENTED_EDGE('',*,*,#23240,.T.);
#37277=ORIENTED_EDGE('',*,*,#26366,.F.);
#37278=ORIENTED_EDGE('',*,*,#24357,.F.);
#37279=ORIENTED_EDGE('',*,*,#26368,.T.);
#37280=ORIENTED_EDGE('',*,*,#23241,.T.);
#37281=ORIENTED_EDGE('',*,*,#26367,.F.);
#37282=ORIENTED_EDGE('',*,*,#24356,.F.);
#37283=ORIENTED_EDGE('',*,*,#26364,.T.);
#37284=ORIENTED_EDGE('',*,*,#23242,.T.);
#37285=ORIENTED_EDGE('',*,*,#26368,.F.);
#37286=ORIENTED_EDGE('',*,*,#24355,.F.);
#37287=ORIENTED_EDGE('',*,*,#26369,.T.);
#37288=ORIENTED_EDGE('',*,*,#23231,.T.);
#37289=ORIENTED_EDGE('',*,*,#26370,.F.);
#37290=ORIENTED_EDGE('',*,*,#24348,.F.);
#37291=ORIENTED_EDGE('',*,*,#26371,.T.);
#37292=ORIENTED_EDGE('',*,*,#23232,.T.);
#37293=ORIENTED_EDGE('',*,*,#26369,.F.);
#37294=ORIENTED_EDGE('',*,*,#24347,.F.);
#37295=ORIENTED_EDGE('',*,*,#26372,.T.);
#37296=ORIENTED_EDGE('',*,*,#23233,.T.);
#37297=ORIENTED_EDGE('',*,*,#26371,.F.);
#37298=ORIENTED_EDGE('',*,*,#24352,.F.);
#37299=ORIENTED_EDGE('',*,*,#26373,.T.);
#37300=ORIENTED_EDGE('',*,*,#23234,.T.);
#37301=ORIENTED_EDGE('',*,*,#26372,.F.);
#37302=ORIENTED_EDGE('',*,*,#24351,.F.);
#37303=ORIENTED_EDGE('',*,*,#26374,.T.);
#37304=ORIENTED_EDGE('',*,*,#23235,.T.);
#37305=ORIENTED_EDGE('',*,*,#26373,.F.);
#37306=ORIENTED_EDGE('',*,*,#24350,.F.);
#37307=ORIENTED_EDGE('',*,*,#26370,.T.);
#37308=ORIENTED_EDGE('',*,*,#23236,.T.);
#37309=ORIENTED_EDGE('',*,*,#26374,.F.);
#37310=ORIENTED_EDGE('',*,*,#24349,.F.);
#37311=ORIENTED_EDGE('',*,*,#26375,.T.);
#37312=ORIENTED_EDGE('',*,*,#23225,.T.);
#37313=ORIENTED_EDGE('',*,*,#26376,.F.);
#37314=ORIENTED_EDGE('',*,*,#24342,.F.);
#37315=ORIENTED_EDGE('',*,*,#26377,.T.);
#37316=ORIENTED_EDGE('',*,*,#23226,.T.);
#37317=ORIENTED_EDGE('',*,*,#26375,.F.);
#37318=ORIENTED_EDGE('',*,*,#24341,.F.);
#37319=ORIENTED_EDGE('',*,*,#26378,.T.);
#37320=ORIENTED_EDGE('',*,*,#23227,.T.);
#37321=ORIENTED_EDGE('',*,*,#26377,.F.);
#37322=ORIENTED_EDGE('',*,*,#24346,.F.);
#37323=ORIENTED_EDGE('',*,*,#26379,.T.);
#37324=ORIENTED_EDGE('',*,*,#23228,.T.);
#37325=ORIENTED_EDGE('',*,*,#26378,.F.);
#37326=ORIENTED_EDGE('',*,*,#24345,.F.);
#37327=ORIENTED_EDGE('',*,*,#26380,.T.);
#37328=ORIENTED_EDGE('',*,*,#23229,.T.);
#37329=ORIENTED_EDGE('',*,*,#26379,.F.);
#37330=ORIENTED_EDGE('',*,*,#24344,.F.);
#37331=ORIENTED_EDGE('',*,*,#26376,.T.);
#37332=ORIENTED_EDGE('',*,*,#23230,.T.);
#37333=ORIENTED_EDGE('',*,*,#26380,.F.);
#37334=ORIENTED_EDGE('',*,*,#24343,.F.);
#37335=ORIENTED_EDGE('',*,*,#26381,.T.);
#37336=ORIENTED_EDGE('',*,*,#23219,.T.);
#37337=ORIENTED_EDGE('',*,*,#26382,.F.);
#37338=ORIENTED_EDGE('',*,*,#24336,.F.);
#37339=ORIENTED_EDGE('',*,*,#26383,.T.);
#37340=ORIENTED_EDGE('',*,*,#23220,.T.);
#37341=ORIENTED_EDGE('',*,*,#26381,.F.);
#37342=ORIENTED_EDGE('',*,*,#24335,.F.);
#37343=ORIENTED_EDGE('',*,*,#26384,.T.);
#37344=ORIENTED_EDGE('',*,*,#23221,.T.);
#37345=ORIENTED_EDGE('',*,*,#26383,.F.);
#37346=ORIENTED_EDGE('',*,*,#24340,.F.);
#37347=ORIENTED_EDGE('',*,*,#26385,.T.);
#37348=ORIENTED_EDGE('',*,*,#23222,.T.);
#37349=ORIENTED_EDGE('',*,*,#26384,.F.);
#37350=ORIENTED_EDGE('',*,*,#24339,.F.);
#37351=ORIENTED_EDGE('',*,*,#26386,.T.);
#37352=ORIENTED_EDGE('',*,*,#23223,.T.);
#37353=ORIENTED_EDGE('',*,*,#26385,.F.);
#37354=ORIENTED_EDGE('',*,*,#24338,.F.);
#37355=ORIENTED_EDGE('',*,*,#26382,.T.);
#37356=ORIENTED_EDGE('',*,*,#23224,.T.);
#37357=ORIENTED_EDGE('',*,*,#26386,.F.);
#37358=ORIENTED_EDGE('',*,*,#24337,.F.);
#37359=ORIENTED_EDGE('',*,*,#26387,.T.);
#37360=ORIENTED_EDGE('',*,*,#23213,.T.);
#37361=ORIENTED_EDGE('',*,*,#26388,.F.);
#37362=ORIENTED_EDGE('',*,*,#24330,.F.);
#37363=ORIENTED_EDGE('',*,*,#26389,.T.);
#37364=ORIENTED_EDGE('',*,*,#23214,.T.);
#37365=ORIENTED_EDGE('',*,*,#26387,.F.);
#37366=ORIENTED_EDGE('',*,*,#24329,.F.);
#37367=ORIENTED_EDGE('',*,*,#26390,.T.);
#37368=ORIENTED_EDGE('',*,*,#23215,.T.);
#37369=ORIENTED_EDGE('',*,*,#26389,.F.);
#37370=ORIENTED_EDGE('',*,*,#24334,.F.);
#37371=ORIENTED_EDGE('',*,*,#26391,.T.);
#37372=ORIENTED_EDGE('',*,*,#23216,.T.);
#37373=ORIENTED_EDGE('',*,*,#26390,.F.);
#37374=ORIENTED_EDGE('',*,*,#24333,.F.);
#37375=ORIENTED_EDGE('',*,*,#26392,.T.);
#37376=ORIENTED_EDGE('',*,*,#23217,.T.);
#37377=ORIENTED_EDGE('',*,*,#26391,.F.);
#37378=ORIENTED_EDGE('',*,*,#24332,.F.);
#37379=ORIENTED_EDGE('',*,*,#26388,.T.);
#37380=ORIENTED_EDGE('',*,*,#23218,.T.);
#37381=ORIENTED_EDGE('',*,*,#26392,.F.);
#37382=ORIENTED_EDGE('',*,*,#24331,.F.);
#37383=ORIENTED_EDGE('',*,*,#26393,.T.);
#37384=ORIENTED_EDGE('',*,*,#23207,.T.);
#37385=ORIENTED_EDGE('',*,*,#26394,.F.);
#37386=ORIENTED_EDGE('',*,*,#24324,.F.);
#37387=ORIENTED_EDGE('',*,*,#26395,.T.);
#37388=ORIENTED_EDGE('',*,*,#23208,.T.);
#37389=ORIENTED_EDGE('',*,*,#26393,.F.);
#37390=ORIENTED_EDGE('',*,*,#24323,.F.);
#37391=ORIENTED_EDGE('',*,*,#26396,.T.);
#37392=ORIENTED_EDGE('',*,*,#23209,.T.);
#37393=ORIENTED_EDGE('',*,*,#26395,.F.);
#37394=ORIENTED_EDGE('',*,*,#24328,.F.);
#37395=ORIENTED_EDGE('',*,*,#26397,.T.);
#37396=ORIENTED_EDGE('',*,*,#23210,.T.);
#37397=ORIENTED_EDGE('',*,*,#26396,.F.);
#37398=ORIENTED_EDGE('',*,*,#24327,.F.);
#37399=ORIENTED_EDGE('',*,*,#26398,.T.);
#37400=ORIENTED_EDGE('',*,*,#23211,.T.);
#37401=ORIENTED_EDGE('',*,*,#26397,.F.);
#37402=ORIENTED_EDGE('',*,*,#24326,.F.);
#37403=ORIENTED_EDGE('',*,*,#26394,.T.);
#37404=ORIENTED_EDGE('',*,*,#23212,.T.);
#37405=ORIENTED_EDGE('',*,*,#26398,.F.);
#37406=ORIENTED_EDGE('',*,*,#24325,.F.);
#37407=ORIENTED_EDGE('',*,*,#26399,.T.);
#37408=ORIENTED_EDGE('',*,*,#23201,.T.);
#37409=ORIENTED_EDGE('',*,*,#26400,.F.);
#37410=ORIENTED_EDGE('',*,*,#24318,.F.);
#37411=ORIENTED_EDGE('',*,*,#26401,.T.);
#37412=ORIENTED_EDGE('',*,*,#23202,.T.);
#37413=ORIENTED_EDGE('',*,*,#26399,.F.);
#37414=ORIENTED_EDGE('',*,*,#24317,.F.);
#37415=ORIENTED_EDGE('',*,*,#26402,.T.);
#37416=ORIENTED_EDGE('',*,*,#23203,.T.);
#37417=ORIENTED_EDGE('',*,*,#26401,.F.);
#37418=ORIENTED_EDGE('',*,*,#24322,.F.);
#37419=ORIENTED_EDGE('',*,*,#26403,.T.);
#37420=ORIENTED_EDGE('',*,*,#23204,.T.);
#37421=ORIENTED_EDGE('',*,*,#26402,.F.);
#37422=ORIENTED_EDGE('',*,*,#24321,.F.);
#37423=ORIENTED_EDGE('',*,*,#26404,.T.);
#37424=ORIENTED_EDGE('',*,*,#23205,.T.);
#37425=ORIENTED_EDGE('',*,*,#26403,.F.);
#37426=ORIENTED_EDGE('',*,*,#24320,.F.);
#37427=ORIENTED_EDGE('',*,*,#26400,.T.);
#37428=ORIENTED_EDGE('',*,*,#23206,.T.);
#37429=ORIENTED_EDGE('',*,*,#26404,.F.);
#37430=ORIENTED_EDGE('',*,*,#24319,.F.);
#37431=ORIENTED_EDGE('',*,*,#26405,.T.);
#37432=ORIENTED_EDGE('',*,*,#23195,.T.);
#37433=ORIENTED_EDGE('',*,*,#26406,.F.);
#37434=ORIENTED_EDGE('',*,*,#24312,.F.);
#37435=ORIENTED_EDGE('',*,*,#26407,.T.);
#37436=ORIENTED_EDGE('',*,*,#23196,.T.);
#37437=ORIENTED_EDGE('',*,*,#26405,.F.);
#37438=ORIENTED_EDGE('',*,*,#24311,.F.);
#37439=ORIENTED_EDGE('',*,*,#26408,.T.);
#37440=ORIENTED_EDGE('',*,*,#23197,.T.);
#37441=ORIENTED_EDGE('',*,*,#26407,.F.);
#37442=ORIENTED_EDGE('',*,*,#24316,.F.);
#37443=ORIENTED_EDGE('',*,*,#26409,.T.);
#37444=ORIENTED_EDGE('',*,*,#23198,.T.);
#37445=ORIENTED_EDGE('',*,*,#26408,.F.);
#37446=ORIENTED_EDGE('',*,*,#24315,.F.);
#37447=ORIENTED_EDGE('',*,*,#26410,.T.);
#37448=ORIENTED_EDGE('',*,*,#23199,.T.);
#37449=ORIENTED_EDGE('',*,*,#26409,.F.);
#37450=ORIENTED_EDGE('',*,*,#24314,.F.);
#37451=ORIENTED_EDGE('',*,*,#26406,.T.);
#37452=ORIENTED_EDGE('',*,*,#23200,.T.);
#37453=ORIENTED_EDGE('',*,*,#26410,.F.);
#37454=ORIENTED_EDGE('',*,*,#24313,.F.);
#37455=ORIENTED_EDGE('',*,*,#26411,.T.);
#37456=ORIENTED_EDGE('',*,*,#23189,.T.);
#37457=ORIENTED_EDGE('',*,*,#26412,.F.);
#37458=ORIENTED_EDGE('',*,*,#24306,.F.);
#37459=ORIENTED_EDGE('',*,*,#26413,.T.);
#37460=ORIENTED_EDGE('',*,*,#23190,.T.);
#37461=ORIENTED_EDGE('',*,*,#26411,.F.);
#37462=ORIENTED_EDGE('',*,*,#24305,.F.);
#37463=ORIENTED_EDGE('',*,*,#26414,.T.);
#37464=ORIENTED_EDGE('',*,*,#23191,.T.);
#37465=ORIENTED_EDGE('',*,*,#26413,.F.);
#37466=ORIENTED_EDGE('',*,*,#24310,.F.);
#37467=ORIENTED_EDGE('',*,*,#26415,.T.);
#37468=ORIENTED_EDGE('',*,*,#23192,.T.);
#37469=ORIENTED_EDGE('',*,*,#26414,.F.);
#37470=ORIENTED_EDGE('',*,*,#24309,.F.);
#37471=ORIENTED_EDGE('',*,*,#26416,.T.);
#37472=ORIENTED_EDGE('',*,*,#23193,.T.);
#37473=ORIENTED_EDGE('',*,*,#26415,.F.);
#37474=ORIENTED_EDGE('',*,*,#24308,.F.);
#37475=ORIENTED_EDGE('',*,*,#26412,.T.);
#37476=ORIENTED_EDGE('',*,*,#23194,.T.);
#37477=ORIENTED_EDGE('',*,*,#26416,.F.);
#37478=ORIENTED_EDGE('',*,*,#24307,.F.);
#37479=ORIENTED_EDGE('',*,*,#26417,.T.);
#37480=ORIENTED_EDGE('',*,*,#23183,.T.);
#37481=ORIENTED_EDGE('',*,*,#26418,.F.);
#37482=ORIENTED_EDGE('',*,*,#24300,.F.);
#37483=ORIENTED_EDGE('',*,*,#26419,.T.);
#37484=ORIENTED_EDGE('',*,*,#23184,.T.);
#37485=ORIENTED_EDGE('',*,*,#26417,.F.);
#37486=ORIENTED_EDGE('',*,*,#24299,.F.);
#37487=ORIENTED_EDGE('',*,*,#26420,.T.);
#37488=ORIENTED_EDGE('',*,*,#23185,.T.);
#37489=ORIENTED_EDGE('',*,*,#26419,.F.);
#37490=ORIENTED_EDGE('',*,*,#24304,.F.);
#37491=ORIENTED_EDGE('',*,*,#26421,.T.);
#37492=ORIENTED_EDGE('',*,*,#23186,.T.);
#37493=ORIENTED_EDGE('',*,*,#26420,.F.);
#37494=ORIENTED_EDGE('',*,*,#24303,.F.);
#37495=ORIENTED_EDGE('',*,*,#26422,.T.);
#37496=ORIENTED_EDGE('',*,*,#23187,.T.);
#37497=ORIENTED_EDGE('',*,*,#26421,.F.);
#37498=ORIENTED_EDGE('',*,*,#24302,.F.);
#37499=ORIENTED_EDGE('',*,*,#26418,.T.);
#37500=ORIENTED_EDGE('',*,*,#23188,.T.);
#37501=ORIENTED_EDGE('',*,*,#26422,.F.);
#37502=ORIENTED_EDGE('',*,*,#24301,.F.);
#37503=ORIENTED_EDGE('',*,*,#26423,.T.);
#37504=ORIENTED_EDGE('',*,*,#23177,.T.);
#37505=ORIENTED_EDGE('',*,*,#26424,.F.);
#37506=ORIENTED_EDGE('',*,*,#24294,.F.);
#37507=ORIENTED_EDGE('',*,*,#26425,.T.);
#37508=ORIENTED_EDGE('',*,*,#23178,.T.);
#37509=ORIENTED_EDGE('',*,*,#26423,.F.);
#37510=ORIENTED_EDGE('',*,*,#24293,.F.);
#37511=ORIENTED_EDGE('',*,*,#26426,.T.);
#37512=ORIENTED_EDGE('',*,*,#23179,.T.);
#37513=ORIENTED_EDGE('',*,*,#26425,.F.);
#37514=ORIENTED_EDGE('',*,*,#24298,.F.);
#37515=ORIENTED_EDGE('',*,*,#26427,.T.);
#37516=ORIENTED_EDGE('',*,*,#23180,.T.);
#37517=ORIENTED_EDGE('',*,*,#26426,.F.);
#37518=ORIENTED_EDGE('',*,*,#24297,.F.);
#37519=ORIENTED_EDGE('',*,*,#26428,.T.);
#37520=ORIENTED_EDGE('',*,*,#23181,.T.);
#37521=ORIENTED_EDGE('',*,*,#26427,.F.);
#37522=ORIENTED_EDGE('',*,*,#24296,.F.);
#37523=ORIENTED_EDGE('',*,*,#26424,.T.);
#37524=ORIENTED_EDGE('',*,*,#23182,.T.);
#37525=ORIENTED_EDGE('',*,*,#26428,.F.);
#37526=ORIENTED_EDGE('',*,*,#24295,.F.);
#37527=ORIENTED_EDGE('',*,*,#26429,.T.);
#37528=ORIENTED_EDGE('',*,*,#23171,.T.);
#37529=ORIENTED_EDGE('',*,*,#26430,.F.);
#37530=ORIENTED_EDGE('',*,*,#24288,.F.);
#37531=ORIENTED_EDGE('',*,*,#26431,.T.);
#37532=ORIENTED_EDGE('',*,*,#23172,.T.);
#37533=ORIENTED_EDGE('',*,*,#26429,.F.);
#37534=ORIENTED_EDGE('',*,*,#24287,.F.);
#37535=ORIENTED_EDGE('',*,*,#26432,.T.);
#37536=ORIENTED_EDGE('',*,*,#23173,.T.);
#37537=ORIENTED_EDGE('',*,*,#26431,.F.);
#37538=ORIENTED_EDGE('',*,*,#24292,.F.);
#37539=ORIENTED_EDGE('',*,*,#26433,.T.);
#37540=ORIENTED_EDGE('',*,*,#23174,.T.);
#37541=ORIENTED_EDGE('',*,*,#26432,.F.);
#37542=ORIENTED_EDGE('',*,*,#24291,.F.);
#37543=ORIENTED_EDGE('',*,*,#26434,.T.);
#37544=ORIENTED_EDGE('',*,*,#23175,.T.);
#37545=ORIENTED_EDGE('',*,*,#26433,.F.);
#37546=ORIENTED_EDGE('',*,*,#24290,.F.);
#37547=ORIENTED_EDGE('',*,*,#26430,.T.);
#37548=ORIENTED_EDGE('',*,*,#23176,.T.);
#37549=ORIENTED_EDGE('',*,*,#26434,.F.);
#37550=ORIENTED_EDGE('',*,*,#24289,.F.);
#37551=ORIENTED_EDGE('',*,*,#26435,.T.);
#37552=ORIENTED_EDGE('',*,*,#23165,.T.);
#37553=ORIENTED_EDGE('',*,*,#26436,.F.);
#37554=ORIENTED_EDGE('',*,*,#24282,.F.);
#37555=ORIENTED_EDGE('',*,*,#26437,.T.);
#37556=ORIENTED_EDGE('',*,*,#23166,.T.);
#37557=ORIENTED_EDGE('',*,*,#26435,.F.);
#37558=ORIENTED_EDGE('',*,*,#24281,.F.);
#37559=ORIENTED_EDGE('',*,*,#26438,.T.);
#37560=ORIENTED_EDGE('',*,*,#23167,.T.);
#37561=ORIENTED_EDGE('',*,*,#26437,.F.);
#37562=ORIENTED_EDGE('',*,*,#24286,.F.);
#37563=ORIENTED_EDGE('',*,*,#26439,.T.);
#37564=ORIENTED_EDGE('',*,*,#23168,.T.);
#37565=ORIENTED_EDGE('',*,*,#26438,.F.);
#37566=ORIENTED_EDGE('',*,*,#24285,.F.);
#37567=ORIENTED_EDGE('',*,*,#26440,.T.);
#37568=ORIENTED_EDGE('',*,*,#23169,.T.);
#37569=ORIENTED_EDGE('',*,*,#26439,.F.);
#37570=ORIENTED_EDGE('',*,*,#24284,.F.);
#37571=ORIENTED_EDGE('',*,*,#26436,.T.);
#37572=ORIENTED_EDGE('',*,*,#23170,.T.);
#37573=ORIENTED_EDGE('',*,*,#26440,.F.);
#37574=ORIENTED_EDGE('',*,*,#24283,.F.);
#37575=ORIENTED_EDGE('',*,*,#26441,.T.);
#37576=ORIENTED_EDGE('',*,*,#23159,.T.);
#37577=ORIENTED_EDGE('',*,*,#26442,.F.);
#37578=ORIENTED_EDGE('',*,*,#24276,.F.);
#37579=ORIENTED_EDGE('',*,*,#26443,.T.);
#37580=ORIENTED_EDGE('',*,*,#23160,.T.);
#37581=ORIENTED_EDGE('',*,*,#26441,.F.);
#37582=ORIENTED_EDGE('',*,*,#24275,.F.);
#37583=ORIENTED_EDGE('',*,*,#26444,.T.);
#37584=ORIENTED_EDGE('',*,*,#23161,.T.);
#37585=ORIENTED_EDGE('',*,*,#26443,.F.);
#37586=ORIENTED_EDGE('',*,*,#24280,.F.);
#37587=ORIENTED_EDGE('',*,*,#26445,.T.);
#37588=ORIENTED_EDGE('',*,*,#23162,.T.);
#37589=ORIENTED_EDGE('',*,*,#26444,.F.);
#37590=ORIENTED_EDGE('',*,*,#24279,.F.);
#37591=ORIENTED_EDGE('',*,*,#26446,.T.);
#37592=ORIENTED_EDGE('',*,*,#23163,.T.);
#37593=ORIENTED_EDGE('',*,*,#26445,.F.);
#37594=ORIENTED_EDGE('',*,*,#24278,.F.);
#37595=ORIENTED_EDGE('',*,*,#26442,.T.);
#37596=ORIENTED_EDGE('',*,*,#23164,.T.);
#37597=ORIENTED_EDGE('',*,*,#26446,.F.);
#37598=ORIENTED_EDGE('',*,*,#24277,.F.);
#37599=ORIENTED_EDGE('',*,*,#26447,.T.);
#37600=ORIENTED_EDGE('',*,*,#23153,.T.);
#37601=ORIENTED_EDGE('',*,*,#26448,.F.);
#37602=ORIENTED_EDGE('',*,*,#24270,.F.);
#37603=ORIENTED_EDGE('',*,*,#26449,.T.);
#37604=ORIENTED_EDGE('',*,*,#23154,.T.);
#37605=ORIENTED_EDGE('',*,*,#26447,.F.);
#37606=ORIENTED_EDGE('',*,*,#24269,.F.);
#37607=ORIENTED_EDGE('',*,*,#26450,.T.);
#37608=ORIENTED_EDGE('',*,*,#23155,.T.);
#37609=ORIENTED_EDGE('',*,*,#26449,.F.);
#37610=ORIENTED_EDGE('',*,*,#24274,.F.);
#37611=ORIENTED_EDGE('',*,*,#26451,.T.);
#37612=ORIENTED_EDGE('',*,*,#23156,.T.);
#37613=ORIENTED_EDGE('',*,*,#26450,.F.);
#37614=ORIENTED_EDGE('',*,*,#24273,.F.);
#37615=ORIENTED_EDGE('',*,*,#26452,.T.);
#37616=ORIENTED_EDGE('',*,*,#23157,.T.);
#37617=ORIENTED_EDGE('',*,*,#26451,.F.);
#37618=ORIENTED_EDGE('',*,*,#24272,.F.);
#37619=ORIENTED_EDGE('',*,*,#26448,.T.);
#37620=ORIENTED_EDGE('',*,*,#23158,.T.);
#37621=ORIENTED_EDGE('',*,*,#26452,.F.);
#37622=ORIENTED_EDGE('',*,*,#24271,.F.);
#37623=ORIENTED_EDGE('',*,*,#26453,.T.);
#37624=ORIENTED_EDGE('',*,*,#23147,.T.);
#37625=ORIENTED_EDGE('',*,*,#26454,.F.);
#37626=ORIENTED_EDGE('',*,*,#24264,.F.);
#37627=ORIENTED_EDGE('',*,*,#26455,.T.);
#37628=ORIENTED_EDGE('',*,*,#23148,.T.);
#37629=ORIENTED_EDGE('',*,*,#26453,.F.);
#37630=ORIENTED_EDGE('',*,*,#24263,.F.);
#37631=ORIENTED_EDGE('',*,*,#26456,.T.);
#37632=ORIENTED_EDGE('',*,*,#23149,.T.);
#37633=ORIENTED_EDGE('',*,*,#26455,.F.);
#37634=ORIENTED_EDGE('',*,*,#24268,.F.);
#37635=ORIENTED_EDGE('',*,*,#26457,.T.);
#37636=ORIENTED_EDGE('',*,*,#23150,.T.);
#37637=ORIENTED_EDGE('',*,*,#26456,.F.);
#37638=ORIENTED_EDGE('',*,*,#24267,.F.);
#37639=ORIENTED_EDGE('',*,*,#26458,.T.);
#37640=ORIENTED_EDGE('',*,*,#23151,.T.);
#37641=ORIENTED_EDGE('',*,*,#26457,.F.);
#37642=ORIENTED_EDGE('',*,*,#24266,.F.);
#37643=ORIENTED_EDGE('',*,*,#26454,.T.);
#37644=ORIENTED_EDGE('',*,*,#23152,.T.);
#37645=ORIENTED_EDGE('',*,*,#26458,.F.);
#37646=ORIENTED_EDGE('',*,*,#24265,.F.);
#37647=ORIENTED_EDGE('',*,*,#26459,.T.);
#37648=ORIENTED_EDGE('',*,*,#23141,.T.);
#37649=ORIENTED_EDGE('',*,*,#26460,.F.);
#37650=ORIENTED_EDGE('',*,*,#24258,.F.);
#37651=ORIENTED_EDGE('',*,*,#26461,.T.);
#37652=ORIENTED_EDGE('',*,*,#23142,.T.);
#37653=ORIENTED_EDGE('',*,*,#26459,.F.);
#37654=ORIENTED_EDGE('',*,*,#24257,.F.);
#37655=ORIENTED_EDGE('',*,*,#26462,.T.);
#37656=ORIENTED_EDGE('',*,*,#23143,.T.);
#37657=ORIENTED_EDGE('',*,*,#26461,.F.);
#37658=ORIENTED_EDGE('',*,*,#24262,.F.);
#37659=ORIENTED_EDGE('',*,*,#26463,.T.);
#37660=ORIENTED_EDGE('',*,*,#23144,.T.);
#37661=ORIENTED_EDGE('',*,*,#26462,.F.);
#37662=ORIENTED_EDGE('',*,*,#24261,.F.);
#37663=ORIENTED_EDGE('',*,*,#26464,.T.);
#37664=ORIENTED_EDGE('',*,*,#23145,.T.);
#37665=ORIENTED_EDGE('',*,*,#26463,.F.);
#37666=ORIENTED_EDGE('',*,*,#24260,.F.);
#37667=ORIENTED_EDGE('',*,*,#26460,.T.);
#37668=ORIENTED_EDGE('',*,*,#23146,.T.);
#37669=ORIENTED_EDGE('',*,*,#26464,.F.);
#37670=ORIENTED_EDGE('',*,*,#24259,.F.);
#37671=ORIENTED_EDGE('',*,*,#26465,.T.);
#37672=ORIENTED_EDGE('',*,*,#23135,.T.);
#37673=ORIENTED_EDGE('',*,*,#26466,.F.);
#37674=ORIENTED_EDGE('',*,*,#24252,.F.);
#37675=ORIENTED_EDGE('',*,*,#26467,.T.);
#37676=ORIENTED_EDGE('',*,*,#23136,.T.);
#37677=ORIENTED_EDGE('',*,*,#26465,.F.);
#37678=ORIENTED_EDGE('',*,*,#24251,.F.);
#37679=ORIENTED_EDGE('',*,*,#26468,.T.);
#37680=ORIENTED_EDGE('',*,*,#23137,.T.);
#37681=ORIENTED_EDGE('',*,*,#26467,.F.);
#37682=ORIENTED_EDGE('',*,*,#24256,.F.);
#37683=ORIENTED_EDGE('',*,*,#26469,.T.);
#37684=ORIENTED_EDGE('',*,*,#23138,.T.);
#37685=ORIENTED_EDGE('',*,*,#26468,.F.);
#37686=ORIENTED_EDGE('',*,*,#24255,.F.);
#37687=ORIENTED_EDGE('',*,*,#26470,.T.);
#37688=ORIENTED_EDGE('',*,*,#23139,.T.);
#37689=ORIENTED_EDGE('',*,*,#26469,.F.);
#37690=ORIENTED_EDGE('',*,*,#24254,.F.);
#37691=ORIENTED_EDGE('',*,*,#26466,.T.);
#37692=ORIENTED_EDGE('',*,*,#23140,.T.);
#37693=ORIENTED_EDGE('',*,*,#26470,.F.);
#37694=ORIENTED_EDGE('',*,*,#24253,.F.);
#37695=ORIENTED_EDGE('',*,*,#26471,.T.);
#37696=ORIENTED_EDGE('',*,*,#23129,.T.);
#37697=ORIENTED_EDGE('',*,*,#26472,.F.);
#37698=ORIENTED_EDGE('',*,*,#24246,.F.);
#37699=ORIENTED_EDGE('',*,*,#26473,.T.);
#37700=ORIENTED_EDGE('',*,*,#23130,.T.);
#37701=ORIENTED_EDGE('',*,*,#26471,.F.);
#37702=ORIENTED_EDGE('',*,*,#24245,.F.);
#37703=ORIENTED_EDGE('',*,*,#26474,.T.);
#37704=ORIENTED_EDGE('',*,*,#23131,.T.);
#37705=ORIENTED_EDGE('',*,*,#26473,.F.);
#37706=ORIENTED_EDGE('',*,*,#24250,.F.);
#37707=ORIENTED_EDGE('',*,*,#26475,.T.);
#37708=ORIENTED_EDGE('',*,*,#23132,.T.);
#37709=ORIENTED_EDGE('',*,*,#26474,.F.);
#37710=ORIENTED_EDGE('',*,*,#24249,.F.);
#37711=ORIENTED_EDGE('',*,*,#26476,.T.);
#37712=ORIENTED_EDGE('',*,*,#23133,.T.);
#37713=ORIENTED_EDGE('',*,*,#26475,.F.);
#37714=ORIENTED_EDGE('',*,*,#24248,.F.);
#37715=ORIENTED_EDGE('',*,*,#26472,.T.);
#37716=ORIENTED_EDGE('',*,*,#23134,.T.);
#37717=ORIENTED_EDGE('',*,*,#26476,.F.);
#37718=ORIENTED_EDGE('',*,*,#24247,.F.);
#37719=CYLINDRICAL_SURFACE('',#39985,1.75);
#37720=CYLINDRICAL_SURFACE('',#39988,1.75);
#37721=CYLINDRICAL_SURFACE('',#39991,1.75);
#37722=CYLINDRICAL_SURFACE('',#39994,1.75);
#37723=CYLINDRICAL_SURFACE('',#39997,1.25);
#37724=CYLINDRICAL_SURFACE('',#40000,1.25);
#37725=CYLINDRICAL_SURFACE('',#40003,1.5);
#37726=CYLINDRICAL_SURFACE('',#40006,1.5);
#37727=CYLINDRICAL_SURFACE('',#40009,1.5);
#37728=CYLINDRICAL_SURFACE('',#40012,1.5);
#37729=CYLINDRICAL_SURFACE('',#40015,1.5);
#37730=CYLINDRICAL_SURFACE('',#40018,1.5);
#37731=CYLINDRICAL_SURFACE('',#40021,1.5);
#37732=CYLINDRICAL_SURFACE('',#40024,1.5);
#37733=CYLINDRICAL_SURFACE('',#40027,1.5);
#37734=CYLINDRICAL_SURFACE('',#40030,1.5);
#37735=CYLINDRICAL_SURFACE('',#40033,1.5);
#37736=CYLINDRICAL_SURFACE('',#40036,1.5);
#37737=CYLINDRICAL_SURFACE('',#40039,1.5);
#37738=CYLINDRICAL_SURFACE('',#40042,1.5);
#37739=CYLINDRICAL_SURFACE('',#40045,1.5);
#37740=CYLINDRICAL_SURFACE('',#40048,1.5);
#37741=CYLINDRICAL_SURFACE('',#40051,1.5);
#37742=CYLINDRICAL_SURFACE('',#40054,1.5);
#37743=CYLINDRICAL_SURFACE('',#40057,1.5);
#37744=CYLINDRICAL_SURFACE('',#40060,1.5);
#37745=CYLINDRICAL_SURFACE('',#40063,1.5);
#37746=CYLINDRICAL_SURFACE('',#40066,1.5);
#37747=CYLINDRICAL_SURFACE('',#40069,1.5);
#37748=CYLINDRICAL_SURFACE('',#40072,1.5);
#37749=CYLINDRICAL_SURFACE('',#40075,1.5);
#37750=CYLINDRICAL_SURFACE('',#40078,1.5);
#37751=CYLINDRICAL_SURFACE('',#40081,1.5);
#37752=CYLINDRICAL_SURFACE('',#40084,1.5);
#37753=CYLINDRICAL_SURFACE('',#40087,1.5);
#37754=CYLINDRICAL_SURFACE('',#40090,1.5);
#37755=CYLINDRICAL_SURFACE('',#40093,1.5);
#37756=CYLINDRICAL_SURFACE('',#40096,1.5);
#37757=CYLINDRICAL_SURFACE('',#40099,1.5);
#37758=CYLINDRICAL_SURFACE('',#40102,1.5);
#37759=CYLINDRICAL_SURFACE('',#40105,1.5);
#37760=CYLINDRICAL_SURFACE('',#40108,1.5);
#37761=CYLINDRICAL_SURFACE('',#40111,1.5);
#37762=CYLINDRICAL_SURFACE('',#40114,1.5);
#37763=CYLINDRICAL_SURFACE('',#40117,1.5);
#37764=CYLINDRICAL_SURFACE('',#40120,1.5);
#37765=CYLINDRICAL_SURFACE('',#40123,1.5);
#37766=CYLINDRICAL_SURFACE('',#40126,1.5);
#37767=CYLINDRICAL_SURFACE('',#40129,1.5);
#37768=CYLINDRICAL_SURFACE('',#40132,1.5);
#37769=CYLINDRICAL_SURFACE('',#40135,1.5);
#37770=CYLINDRICAL_SURFACE('',#40138,1.5);
#37771=CYLINDRICAL_SURFACE('',#40141,1.5);
#37772=CYLINDRICAL_SURFACE('',#40144,1.5);
#37773=CYLINDRICAL_SURFACE('',#40147,1.5);
#37774=CYLINDRICAL_SURFACE('',#40150,1.5);
#37775=CYLINDRICAL_SURFACE('',#40153,1.5);
#37776=CYLINDRICAL_SURFACE('',#40156,1.5);
#37777=CYLINDRICAL_SURFACE('',#40159,1.5);
#37778=CYLINDRICAL_SURFACE('',#40162,1.5);
#37779=CYLINDRICAL_SURFACE('',#40165,1.5);
#37780=CYLINDRICAL_SURFACE('',#40168,1.5);
#37781=CYLINDRICAL_SURFACE('',#40171,1.5);
#37782=CYLINDRICAL_SURFACE('',#40174,1.5);
#37783=CYLINDRICAL_SURFACE('',#40177,1.5);
#37784=CYLINDRICAL_SURFACE('',#40180,1.5);
#37785=CYLINDRICAL_SURFACE('',#40183,1.5);
#37786=CYLINDRICAL_SURFACE('',#40186,1.5);
#37787=CYLINDRICAL_SURFACE('',#40189,1.5);
#37788=CYLINDRICAL_SURFACE('',#40192,1.5);
#37789=CYLINDRICAL_SURFACE('',#40195,1.5);
#37790=CYLINDRICAL_SURFACE('',#40198,1.5);
#37791=CYLINDRICAL_SURFACE('',#40201,1.74999999999999);
#37792=CYLINDRICAL_SURFACE('',#40204,1.74999999999998);
#37793=CYLINDRICAL_SURFACE('',#40207,1.75);
#37794=CYLINDRICAL_SURFACE('',#40210,1.75);
#37795=CYLINDRICAL_SURFACE('',#40227,1.25);
#37796=CYLINDRICAL_SURFACE('',#40230,1.25);
#37797=CYLINDRICAL_SURFACE('',#40233,1.25);
#37798=CYLINDRICAL_SURFACE('',#40236,1.25);
#37799=CYLINDRICAL_SURFACE('',#40459,1.5);
#37800=CYLINDRICAL_SURFACE('',#40461,1.5);
#37801=CYLINDRICAL_SURFACE('',#40463,1.5);
#37802=CYLINDRICAL_SURFACE('',#40465,1.5);
#37803=CYLINDRICAL_SURFACE('',#40467,1.6);
#37804=CYLINDRICAL_SURFACE('',#40468,0.799999999999995);
#37805=CYLINDRICAL_SURFACE('',#40474,1.5);
#37806=CYLINDRICAL_SURFACE('',#40475,1.5);
#37807=CYLINDRICAL_SURFACE('',#40476,1.6);
#37808=CYLINDRICAL_SURFACE('',#40477,0.799999999999995);
#37809=CYLINDRICAL_SURFACE('',#40483,1.5);
#37810=CYLINDRICAL_SURFACE('',#40484,1.5);
#37811=CYLINDRICAL_SURFACE('',#40491,2.);
#37812=CYLINDRICAL_SURFACE('',#40494,2.);
#37813=CYLINDRICAL_SURFACE('',#40511,1.5);
#37814=CYLINDRICAL_SURFACE('',#40512,1.5);
#37815=CYLINDRICAL_SURFACE('',#40516,2.3);
#37816=CYLINDRICAL_SURFACE('',#40517,2.3);
#37817=CYLINDRICAL_SURFACE('',#40518,1.20000000000001);
#37818=CYLINDRICAL_SURFACE('',#40519,1.2);
#37819=CYLINDRICAL_SURFACE('',#40529,2.);
#37820=CYLINDRICAL_SURFACE('',#40532,2.);
#37821=CYLINDRICAL_SURFACE('',#40549,1.5);
#37822=CYLINDRICAL_SURFACE('',#40550,1.5);
#37823=CYLINDRICAL_SURFACE('',#40554,2.3);
#37824=CYLINDRICAL_SURFACE('',#40555,2.3);
#37825=CYLINDRICAL_SURFACE('',#40556,1.20000000000001);
#37826=CYLINDRICAL_SURFACE('',#40557,1.2);
#37827=CYLINDRICAL_SURFACE('',#40567,2.);
#37828=CYLINDRICAL_SURFACE('',#40570,2.);
#37829=CYLINDRICAL_SURFACE('',#40587,1.5);
#37830=CYLINDRICAL_SURFACE('',#40588,1.5);
#37831=CYLINDRICAL_SURFACE('',#40592,2.3);
#37832=CYLINDRICAL_SURFACE('',#40593,2.3);
#37833=CYLINDRICAL_SURFACE('',#40594,1.2);
#37834=CYLINDRICAL_SURFACE('',#40595,1.2);
#37835=CYLINDRICAL_SURFACE('',#40605,2.);
#37836=CYLINDRICAL_SURFACE('',#40608,2.);
#37837=CYLINDRICAL_SURFACE('',#40625,1.5);
#37838=CYLINDRICAL_SURFACE('',#40626,1.5);
#37839=CYLINDRICAL_SURFACE('',#40630,2.3);
#37840=CYLINDRICAL_SURFACE('',#40631,2.3);
#37841=CYLINDRICAL_SURFACE('',#40632,1.2);
#37842=CYLINDRICAL_SURFACE('',#40633,1.2);
#37843=CYLINDRICAL_SURFACE('',#40703,1.5);
#37844=CYLINDRICAL_SURFACE('',#40704,1.5);
#37845=CYLINDRICAL_SURFACE('',#40705,1.5);
#37846=CYLINDRICAL_SURFACE('',#40706,1.5);
#37847=CYLINDRICAL_SURFACE('',#40707,1.5);
#37848=CYLINDRICAL_SURFACE('',#40708,1.5);
#37849=CYLINDRICAL_SURFACE('',#40709,1.5);
#37850=CYLINDRICAL_SURFACE('',#40710,1.5);
#37851=CYLINDRICAL_SURFACE('',#40711,1.5);
#37852=CYLINDRICAL_SURFACE('',#40712,1.5);
#37853=CYLINDRICAL_SURFACE('',#40713,1.5);
#37854=CYLINDRICAL_SURFACE('',#40714,1.5);
#37855=CYLINDRICAL_SURFACE('',#40715,1.5);
#37856=CYLINDRICAL_SURFACE('',#40716,1.5);
#37857=CYLINDRICAL_SURFACE('',#40717,1.5);
#37858=CYLINDRICAL_SURFACE('',#40718,1.5);
#37859=CYLINDRICAL_SURFACE('',#40719,1.5);
#37860=CYLINDRICAL_SURFACE('',#40720,1.5);
#37861=CYLINDRICAL_SURFACE('',#40721,1.5);
#37862=CYLINDRICAL_SURFACE('',#40722,1.5);
#37863=CYLINDRICAL_SURFACE('',#40723,1.5);
#37864=CYLINDRICAL_SURFACE('',#40724,1.5);
#37865=CYLINDRICAL_SURFACE('',#40725,1.5);
#37866=CYLINDRICAL_SURFACE('',#40726,1.5);
#37867=CYLINDRICAL_SURFACE('',#40727,1.5);
#37868=CYLINDRICAL_SURFACE('',#40728,1.5);
#37869=CYLINDRICAL_SURFACE('',#40729,1.5);
#37870=CYLINDRICAL_SURFACE('',#40730,1.5);
#37871=CYLINDRICAL_SURFACE('',#40731,1.5);
#37872=CYLINDRICAL_SURFACE('',#40732,1.5);
#37873=CYLINDRICAL_SURFACE('',#40733,1.5);
#37874=CYLINDRICAL_SURFACE('',#40734,1.5);
#37875=CYLINDRICAL_SURFACE('',#40735,1.5);
#37876=CYLINDRICAL_SURFACE('',#40736,1.5);
#37877=CYLINDRICAL_SURFACE('',#40737,1.5);
#37878=CYLINDRICAL_SURFACE('',#40738,1.5);
#37879=CYLINDRICAL_SURFACE('',#40739,1.5);
#37880=CYLINDRICAL_SURFACE('',#40740,1.5);
#37881=CYLINDRICAL_SURFACE('',#40741,1.5);
#37882=CYLINDRICAL_SURFACE('',#40742,1.5);
#37883=CYLINDRICAL_SURFACE('',#40743,1.5);
#37884=CYLINDRICAL_SURFACE('',#40744,1.5);
#37885=CYLINDRICAL_SURFACE('',#40745,1.5);
#37886=CYLINDRICAL_SURFACE('',#40746,1.5);
#37887=CYLINDRICAL_SURFACE('',#40747,1.5);
#37888=CYLINDRICAL_SURFACE('',#40748,1.5);
#37889=CYLINDRICAL_SURFACE('',#40749,1.5);
#37890=CYLINDRICAL_SURFACE('',#40750,1.5);
#37891=CYLINDRICAL_SURFACE('',#40751,1.5);
#37892=CYLINDRICAL_SURFACE('',#40752,1.5);
#37893=CYLINDRICAL_SURFACE('',#40753,1.5);
#37894=CYLINDRICAL_SURFACE('',#40754,1.5);
#37895=CYLINDRICAL_SURFACE('',#40755,1.5);
#37896=CYLINDRICAL_SURFACE('',#40756,1.5);
#37897=CYLINDRICAL_SURFACE('',#40757,2.667);
#37898=CYLINDRICAL_SURFACE('',#40759,2.667);
#37899=CYLINDRICAL_SURFACE('',#40761,2.66699999999999);
#37900=CYLINDRICAL_SURFACE('',#40763,2.667);
#37901=CYLINDRICAL_SURFACE('',#40765,2.667);
#37902=CYLINDRICAL_SURFACE('',#40767,2.667);
#37903=CYLINDRICAL_SURFACE('',#40778,1.5);
#37904=CYLINDRICAL_SURFACE('',#40782,1.5);
#37905=CYLINDRICAL_SURFACE('',#40785,1.5);
#37906=CYLINDRICAL_SURFACE('',#40787,1.5);
#37907=CYLINDRICAL_SURFACE('',#40791,1.5);
#37908=CYLINDRICAL_SURFACE('',#40793,1.5);
#37909=CYLINDRICAL_SURFACE('',#40796,1.5);
#37910=CYLINDRICAL_SURFACE('',#40800,1.5);
#37911=CYLINDRICAL_SURFACE('',#40803,1.5);
#37912=CYLINDRICAL_SURFACE('',#40806,1.5);
#37913=CYLINDRICAL_SURFACE('',#40809,1.5);
#37914=CYLINDRICAL_SURFACE('',#40811,1.5);
#37915=CYLINDRICAL_SURFACE('',#40814,1.5);
#37916=CYLINDRICAL_SURFACE('',#40817,1.5);
#37917=CYLINDRICAL_SURFACE('',#40820,1.5);
#37918=CYLINDRICAL_SURFACE('',#40823,1.5);
#37919=CYLINDRICAL_SURFACE('',#40826,1.5);
#37920=CYLINDRICAL_SURFACE('',#40829,1.5);
#37921=CYLINDRICAL_SURFACE('',#40833,1.5);
#37922=CYLINDRICAL_SURFACE('',#40836,1.5);
#37923=CYLINDRICAL_SURFACE('',#40839,1.5);
#37924=CYLINDRICAL_SURFACE('',#40842,1.5);
#37925=CYLINDRICAL_SURFACE('',#40845,1.5);
#37926=CYLINDRICAL_SURFACE('',#40847,1.5);
#37927=CYLINDRICAL_SURFACE('',#40850,1.5);
#37928=CYLINDRICAL_SURFACE('',#40853,1.5);
#37929=CYLINDRICAL_SURFACE('',#40856,1.5);
#37930=CYLINDRICAL_SURFACE('',#40859,1.5);
#37931=CYLINDRICAL_SURFACE('',#40862,1.5);
#37932=CYLINDRICAL_SURFACE('',#40865,1.5);
#37933=CYLINDRICAL_SURFACE('',#40868,1.5);
#37934=CYLINDRICAL_SURFACE('',#40871,1.5);
#37935=CYLINDRICAL_SURFACE('',#40874,1.5);
#37936=CYLINDRICAL_SURFACE('',#40877,1.5);
#37937=CYLINDRICAL_SURFACE('',#40880,1.5);
#37938=CYLINDRICAL_SURFACE('',#40883,1.5);
#37939=CYLINDRICAL_SURFACE('',#40886,1.5);
#37940=CYLINDRICAL_SURFACE('',#40889,1.5);
#37941=CYLINDRICAL_SURFACE('',#40892,1.5);
#37942=CYLINDRICAL_SURFACE('',#40895,1.5);
#37943=CYLINDRICAL_SURFACE('',#40898,1.5);
#37944=CYLINDRICAL_SURFACE('',#40901,1.5);
#37945=CYLINDRICAL_SURFACE('',#40904,1.5);
#37946=CYLINDRICAL_SURFACE('',#40907,1.5);
#37947=CYLINDRICAL_SURFACE('',#40910,1.5);
#37948=CYLINDRICAL_SURFACE('',#40913,1.5);
#37949=CYLINDRICAL_SURFACE('',#40916,1.5);
#37950=CYLINDRICAL_SURFACE('',#40919,1.5);
#37951=CYLINDRICAL_SURFACE('',#40933,1.59999999999999);
#37952=CYLINDRICAL_SURFACE('',#40934,0.799999999999995);
#37953=CYLINDRICAL_SURFACE('',#40937,4.);
#37954=CYLINDRICAL_SURFACE('',#40939,4.);
#37955=CYLINDRICAL_SURFACE('',#40946,2.);
#37956=CYLINDRICAL_SURFACE('',#40949,2.);
#37957=CYLINDRICAL_SURFACE('',#40966,1.5);
#37958=CYLINDRICAL_SURFACE('',#40967,1.5);
#37959=CYLINDRICAL_SURFACE('',#40971,2.3);
#37960=CYLINDRICAL_SURFACE('',#40972,2.3);
#37961=CYLINDRICAL_SURFACE('',#40973,1.2);
#37962=CYLINDRICAL_SURFACE('',#40974,1.2);
#37963=CYLINDRICAL_SURFACE('',#40984,2.);
#37964=CYLINDRICAL_SURFACE('',#40987,2.);
#37965=CYLINDRICAL_SURFACE('',#41004,1.5);
#37966=CYLINDRICAL_SURFACE('',#41005,1.5);
#37967=CYLINDRICAL_SURFACE('',#41009,2.3);
#37968=CYLINDRICAL_SURFACE('',#41010,2.3);
#37969=CYLINDRICAL_SURFACE('',#41011,1.2);
#37970=CYLINDRICAL_SURFACE('',#41012,1.2);
#37971=CYLINDRICAL_SURFACE('',#41028,1.59999999999999);
#37972=CYLINDRICAL_SURFACE('',#41029,0.799999999999995);
#37973=CYLINDRICAL_SURFACE('',#41038,4.);
#37974=CYLINDRICAL_SURFACE('',#41040,4.);
#37975=CYLINDRICAL_SURFACE('',#41042,0.800100000000001);
#37976=CYLINDRICAL_SURFACE('',#41045,0.800100000000001);
#37977=CYLINDRICAL_SURFACE('',#41048,0.800100000000001);
#37978=CYLINDRICAL_SURFACE('',#41059,1.20015);
#37979=CYLINDRICAL_SURFACE('',#41061,3.556);
#37980=CYLINDRICAL_SURFACE('',#41064,1.20015);
#37981=CYLINDRICAL_SURFACE('',#41115,3.556);
#37982=CYLINDRICAL_SURFACE('',#41119,3.556);
#37983=CYLINDRICAL_SURFACE('',#41123,3.556);
#37984=CYLINDRICAL_SURFACE('',#41127,3.556);
#37985=CYLINDRICAL_SURFACE('',#41132,3.556);
#37986=CYLINDRICAL_SURFACE('',#41142,0.3556);
#37987=CYLINDRICAL_SURFACE('',#41144,0.3556);
#37988=CYLINDRICAL_SURFACE('',#41150,0.3556);
#37989=CYLINDRICAL_SURFACE('',#41152,0.3556);
#37990=CYLINDRICAL_SURFACE('',#41155,2.667);
#37991=CYLINDRICAL_SURFACE('',#41157,2.667);
#37992=CYLINDRICAL_SURFACE('',#41159,2.667);
#37993=CYLINDRICAL_SURFACE('',#41161,2.66700000000001);
#37994=CYLINDRICAL_SURFACE('',#41163,2.667);
#37995=CYLINDRICAL_SURFACE('',#41165,2.667);
#37996=CYLINDRICAL_SURFACE('',#41167,1.778);
#37997=CYLINDRICAL_SURFACE('',#41169,1.778);
#37998=CYLINDRICAL_SURFACE('',#41171,1.778);
#37999=CYLINDRICAL_SURFACE('',#41173,1.778);
#38000=CYLINDRICAL_SURFACE('',#41175,1.778);
#38001=CYLINDRICAL_SURFACE('',#41177,1.778);
#38002=CYLINDRICAL_SURFACE('',#41231,1.);
#38003=CYLINDRICAL_SURFACE('',#41234,1.);
#38004=CYLINDRICAL_SURFACE('',#41237,56.);
#38005=CYLINDRICAL_SURFACE('',#41287,1.);
#38006=CYLINDRICAL_SURFACE('',#41288,1.);
#38007=CYLINDRICAL_SURFACE('',#41338,1.6);
#38008=CYLINDRICAL_SURFACE('',#41339,0.799999999999995);
#38009=CYLINDRICAL_SURFACE('',#41346,1.6);
#38010=CYLINDRICAL_SURFACE('',#41347,0.799999999999995);
#38011=CYLINDRICAL_SURFACE('',#41348,5.);
#38012=CYLINDRICAL_SURFACE('',#41352,5.);
#38013=CYLINDRICAL_SURFACE('',#41368,1.6);
#38014=CYLINDRICAL_SURFACE('',#41369,0.799999999999995);
#38015=CYLINDRICAL_SURFACE('',#41376,1.6);
#38016=CYLINDRICAL_SURFACE('',#41377,0.799999999999995);
#38017=CYLINDRICAL_SURFACE('',#41378,5.);
#38018=CYLINDRICAL_SURFACE('',#41382,5.);
#38019=ADVANCED_FACE('',(#2331),#37719,.F.);
#38020=ADVANCED_FACE('',(#2332),#37720,.F.);
#38021=ADVANCED_FACE('',(#2333),#37721,.F.);
#38022=ADVANCED_FACE('',(#2334),#37722,.F.);
#38023=ADVANCED_FACE('',(#2335),#37723,.F.);
#38024=ADVANCED_FACE('',(#2336),#37724,.F.);
#38025=ADVANCED_FACE('',(#2337),#37725,.F.);
#38026=ADVANCED_FACE('',(#2338),#37726,.F.);
#38027=ADVANCED_FACE('',(#2339),#37727,.F.);
#38028=ADVANCED_FACE('',(#2340),#37728,.F.);
#38029=ADVANCED_FACE('',(#2341),#37729,.F.);
#38030=ADVANCED_FACE('',(#2342),#37730,.F.);
#38031=ADVANCED_FACE('',(#2343),#37731,.F.);
#38032=ADVANCED_FACE('',(#2344),#37732,.F.);
#38033=ADVANCED_FACE('',(#2345),#37733,.F.);
#38034=ADVANCED_FACE('',(#2346),#37734,.F.);
#38035=ADVANCED_FACE('',(#2347),#37735,.F.);
#38036=ADVANCED_FACE('',(#2348),#37736,.F.);
#38037=ADVANCED_FACE('',(#2349),#37737,.F.);
#38038=ADVANCED_FACE('',(#2350),#37738,.F.);
#38039=ADVANCED_FACE('',(#2351),#37739,.F.);
#38040=ADVANCED_FACE('',(#2352),#37740,.F.);
#38041=ADVANCED_FACE('',(#2353),#37741,.F.);
#38042=ADVANCED_FACE('',(#2354),#37742,.F.);
#38043=ADVANCED_FACE('',(#2355),#37743,.F.);
#38044=ADVANCED_FACE('',(#2356),#37744,.F.);
#38045=ADVANCED_FACE('',(#2357),#37745,.F.);
#38046=ADVANCED_FACE('',(#2358),#37746,.F.);
#38047=ADVANCED_FACE('',(#2359),#37747,.F.);
#38048=ADVANCED_FACE('',(#2360),#37748,.F.);
#38049=ADVANCED_FACE('',(#2361),#37749,.F.);
#38050=ADVANCED_FACE('',(#2362),#37750,.F.);
#38051=ADVANCED_FACE('',(#2363),#37751,.F.);
#38052=ADVANCED_FACE('',(#2364),#37752,.F.);
#38053=ADVANCED_FACE('',(#2365),#37753,.F.);
#38054=ADVANCED_FACE('',(#2366),#37754,.F.);
#38055=ADVANCED_FACE('',(#2367),#37755,.F.);
#38056=ADVANCED_FACE('',(#2368),#37756,.F.);
#38057=ADVANCED_FACE('',(#2369),#37757,.F.);
#38058=ADVANCED_FACE('',(#2370),#37758,.F.);
#38059=ADVANCED_FACE('',(#2371),#37759,.F.);
#38060=ADVANCED_FACE('',(#2372),#37760,.F.);
#38061=ADVANCED_FACE('',(#2373),#37761,.F.);
#38062=ADVANCED_FACE('',(#2374),#37762,.F.);
#38063=ADVANCED_FACE('',(#2375),#37763,.F.);
#38064=ADVANCED_FACE('',(#2376),#37764,.F.);
#38065=ADVANCED_FACE('',(#2377),#37765,.F.);
#38066=ADVANCED_FACE('',(#2378),#37766,.F.);
#38067=ADVANCED_FACE('',(#2379),#37767,.F.);
#38068=ADVANCED_FACE('',(#2380),#37768,.F.);
#38069=ADVANCED_FACE('',(#2381),#37769,.F.);
#38070=ADVANCED_FACE('',(#2382),#37770,.F.);
#38071=ADVANCED_FACE('',(#2383),#37771,.F.);
#38072=ADVANCED_FACE('',(#2384),#37772,.F.);
#38073=ADVANCED_FACE('',(#2385),#37773,.F.);
#38074=ADVANCED_FACE('',(#2386),#37774,.F.);
#38075=ADVANCED_FACE('',(#2387),#37775,.F.);
#38076=ADVANCED_FACE('',(#2388),#37776,.F.);
#38077=ADVANCED_FACE('',(#2389),#37777,.F.);
#38078=ADVANCED_FACE('',(#2390),#37778,.F.);
#38079=ADVANCED_FACE('',(#2391),#37779,.F.);
#38080=ADVANCED_FACE('',(#2392),#37780,.F.);
#38081=ADVANCED_FACE('',(#2393),#37781,.F.);
#38082=ADVANCED_FACE('',(#2394),#37782,.F.);
#38083=ADVANCED_FACE('',(#2395),#37783,.F.);
#38084=ADVANCED_FACE('',(#2396),#37784,.F.);
#38085=ADVANCED_FACE('',(#2397),#37785,.F.);
#38086=ADVANCED_FACE('',(#2398),#37786,.F.);
#38087=ADVANCED_FACE('',(#2399),#37787,.F.);
#38088=ADVANCED_FACE('',(#2400),#37788,.F.);
#38089=ADVANCED_FACE('',(#2401),#37789,.F.);
#38090=ADVANCED_FACE('',(#2402),#37790,.F.);
#38091=ADVANCED_FACE('',(#2403),#2285,.T.);
#38092=ADVANCED_FACE('',(#2404),#2286,.T.);
#38093=ADVANCED_FACE('',(#2405),#2287,.T.);
#38094=ADVANCED_FACE('',(#2406),#2288,.T.);
#38095=ADVANCED_FACE('',(#2407),#2289,.T.);
#38096=ADVANCED_FACE('',(#2408),#37791,.F.);
#38097=ADVANCED_FACE('',(#2409),#37792,.F.);
#38098=ADVANCED_FACE('',(#2410),#37793,.F.);
#38099=ADVANCED_FACE('',(#2411),#37794,.F.);
#38100=ADVANCED_FACE('',(#2412),#2181,.F.);
#38101=ADVANCED_FACE('',(#2413),#2182,.F.);
#38102=ADVANCED_FACE('',(#2414),#2183,.T.);
#38103=ADVANCED_FACE('',(#2415),#2184,.T.);
#38104=ADVANCED_FACE('',(#2416),#37795,.F.);
#38105=ADVANCED_FACE('',(#2417),#37796,.F.);
#38106=ADVANCED_FACE('',(#2418),#37797,.F.);
#38107=ADVANCED_FACE('',(#2419),#37798,.F.);
#38108=ADVANCED_FACE('',(#2420),#2290,.F.);
#38109=ADVANCED_FACE('',(#2421,#48,#49,#50,#51),#629,.F.);
#38110=ADVANCED_FACE('',(#2422,#52,#53,#54,#55),#630,.T.);
#38111=ADVANCED_FACE('',(#2423),#631,.T.);
#38112=ADVANCED_FACE('',(#2424),#632,.T.);
#38113=ADVANCED_FACE('',(#2425,#56,#57),#633,.T.);
#38114=ADVANCED_FACE('',(#2426,#58,#59),#634,.F.);
#38115=ADVANCED_FACE('',(#2427),#635,.T.);
#38116=ADVANCED_FACE('',(#2428),#636,.T.);
#38117=ADVANCED_FACE('',(#2429,#60,#61,#62,#63,#64,#65,#66,#67,#68,#69,
#70,#71,#72,#73,#74,#75,#76,#77,#78,#79,#80,#81,#82,#83,#84,#85,#86,#87,
#88,#89,#90,#91,#92,#93,#94,#95,#96,#97,#98,#99,#100,#101,#102,#103,#104,
#105,#106,#107),#637,.T.);
#38118=ADVANCED_FACE('',(#2430,#108,#109,#110,#111,#112,#113,#114,#115,
#116,#117,#118,#119,#120,#121,#122,#123,#124,#125,#126,#127,#128,#129,#130,
#131,#132,#133,#134,#135,#136,#137,#138,#139,#140,#141,#142,#143,#144,#145,
#146,#147,#148,#149,#150,#151,#152,#153,#154,#155),#638,.F.);
#38119=ADVANCED_FACE('',(#2431),#639,.T.);
#38120=ADVANCED_FACE('',(#2432),#640,.T.);
#38121=ADVANCED_FACE('',(#2433),#641,.T.);
#38122=ADVANCED_FACE('',(#2434),#642,.T.);
#38123=ADVANCED_FACE('',(#2435),#643,.T.);
#38124=ADVANCED_FACE('',(#2436),#644,.T.);
#38125=ADVANCED_FACE('',(#2437),#645,.T.);
#38126=ADVANCED_FACE('',(#2438),#646,.T.);
#38127=ADVANCED_FACE('',(#2439),#647,.T.);
#38128=ADVANCED_FACE('',(#2440),#648,.T.);
#38129=ADVANCED_FACE('',(#2441),#649,.T.);
#38130=ADVANCED_FACE('',(#2442),#650,.T.);
#38131=ADVANCED_FACE('',(#2443),#651,.T.);
#38132=ADVANCED_FACE('',(#2444),#652,.T.);
#38133=ADVANCED_FACE('',(#2445),#653,.T.);
#38134=ADVANCED_FACE('',(#2446),#654,.T.);
#38135=ADVANCED_FACE('',(#2447),#655,.T.);
#38136=ADVANCED_FACE('',(#2448),#656,.T.);
#38137=ADVANCED_FACE('',(#2449),#657,.T.);
#38138=ADVANCED_FACE('',(#2450),#658,.T.);
#38139=ADVANCED_FACE('',(#2451),#659,.T.);
#38140=ADVANCED_FACE('',(#2452),#660,.T.);
#38141=ADVANCED_FACE('',(#2453),#661,.T.);
#38142=ADVANCED_FACE('',(#2454),#662,.T.);
#38143=ADVANCED_FACE('',(#2455),#2291,.F.);
#38144=ADVANCED_FACE('',(#2456,#156,#157,#158,#159,#160,#161,#162,#163,
#164,#165,#166,#167,#168,#169,#170,#171,#172,#173),#663,.F.);
#38145=ADVANCED_FACE('',(#2457),#2292,.F.);
#38146=ADVANCED_FACE('',(#2458),#664,.T.);
#38147=ADVANCED_FACE('',(#2459),#2293,.F.);
#38148=ADVANCED_FACE('',(#2460),#2294,.F.);
#38149=ADVANCED_FACE('',(#2461),#2295,.F.);
#38150=ADVANCED_FACE('',(#2462,#174,#175,#176,#177,#178,#179,#180,#181,
#182,#183,#184),#665,.T.);
#38151=ADVANCED_FACE('',(#2463,#185,#186,#187,#188,#189,#190,#191,#192,
#193,#194,#195),#666,.F.);
#38152=ADVANCED_FACE('',(#2464),#37799,.F.);
#38153=ADVANCED_FACE('',(#2465),#667,.F.);
#38154=ADVANCED_FACE('',(#2466),#37800,.F.);
#38155=ADVANCED_FACE('',(#2467),#668,.F.);
#38156=ADVANCED_FACE('',(#2468),#37801,.F.);
#38157=ADVANCED_FACE('',(#2469),#669,.F.);
#38158=ADVANCED_FACE('',(#2470),#37802,.F.);
#38159=ADVANCED_FACE('',(#2471),#670,.F.);
#38160=ADVANCED_FACE('',(#2472),#2296,.T.);
#38161=ADVANCED_FACE('',(#2473),#2297,.T.);
#38162=ADVANCED_FACE('',(#2474),#37803,.T.);
#38163=ADVANCED_FACE('',(#2475),#37804,.F.);
#38164=ADVANCED_FACE('',(#2476),#671,.F.);
#38165=ADVANCED_FACE('',(#2477),#672,.T.);
#38166=ADVANCED_FACE('',(#2478),#673,.T.);
#38167=ADVANCED_FACE('',(#2479),#674,.T.);
#38168=ADVANCED_FACE('',(#2480),#675,.F.);
#38169=ADVANCED_FACE('',(#2481),#37805,.F.);
#38170=ADVANCED_FACE('',(#2482),#37806,.F.);
#38171=ADVANCED_FACE('',(#2483),#2298,.T.);
#38172=ADVANCED_FACE('',(#2484),#2299,.T.);
#38173=ADVANCED_FACE('',(#2485),#37807,.T.);
#38174=ADVANCED_FACE('',(#2486),#37808,.F.);
#38175=ADVANCED_FACE('',(#2487),#676,.F.);
#38176=ADVANCED_FACE('',(#2488),#677,.F.);
#38177=ADVANCED_FACE('',(#2489),#678,.T.);
#38178=ADVANCED_FACE('',(#2490),#679,.T.);
#38179=ADVANCED_FACE('',(#2491),#680,.F.);
#38180=ADVANCED_FACE('',(#2492),#37809,.F.);
#38181=ADVANCED_FACE('',(#2493),#37810,.F.);
#38182=ADVANCED_FACE('',(#2494),#681,.T.);
#38183=ADVANCED_FACE('',(#2495),#682,.F.);
#38184=ADVANCED_FACE('',(#2496),#37811,.T.);
#38185=ADVANCED_FACE('',(#2497),#37812,.T.);
#38186=ADVANCED_FACE('',(#2498),#683,.F.);
#38187=ADVANCED_FACE('',(#2499),#684,.T.);
#38188=ADVANCED_FACE('',(#2500),#37813,.F.);
#38189=ADVANCED_FACE('',(#2501),#37814,.F.);
#38190=ADVANCED_FACE('',(#2502),#685,.F.);
#38191=ADVANCED_FACE('',(#2503),#686,.F.);
#38192=ADVANCED_FACE('',(#2504,#196),#687,.F.);
#38193=ADVANCED_FACE('',(#2505),#37815,.T.);
#38194=ADVANCED_FACE('',(#2506),#37816,.T.);
#38195=ADVANCED_FACE('',(#2507),#37817,.F.);
#38196=ADVANCED_FACE('',(#2508),#37818,.F.);
#38197=ADVANCED_FACE('',(#2509),#688,.T.);
#38198=ADVANCED_FACE('',(#2510),#689,.T.);
#38199=ADVANCED_FACE('',(#2511,#197),#690,.T.);
#38200=ADVANCED_FACE('',(#2512),#691,.T.);
#38201=ADVANCED_FACE('',(#2513),#692,.F.);
#38202=ADVANCED_FACE('',(#2514),#37819,.T.);
#38203=ADVANCED_FACE('',(#2515),#37820,.T.);
#38204=ADVANCED_FACE('',(#2516),#693,.F.);
#38205=ADVANCED_FACE('',(#2517),#694,.T.);
#38206=ADVANCED_FACE('',(#2518),#37821,.F.);
#38207=ADVANCED_FACE('',(#2519),#37822,.F.);
#38208=ADVANCED_FACE('',(#2520),#695,.F.);
#38209=ADVANCED_FACE('',(#2521),#696,.F.);
#38210=ADVANCED_FACE('',(#2522,#198),#697,.F.);
#38211=ADVANCED_FACE('',(#2523),#37823,.T.);
#38212=ADVANCED_FACE('',(#2524),#37824,.T.);
#38213=ADVANCED_FACE('',(#2525),#37825,.F.);
#38214=ADVANCED_FACE('',(#2526),#37826,.F.);
#38215=ADVANCED_FACE('',(#2527),#698,.T.);
#38216=ADVANCED_FACE('',(#2528),#699,.T.);
#38217=ADVANCED_FACE('',(#2529,#199),#700,.T.);
#38218=ADVANCED_FACE('',(#2530),#701,.T.);
#38219=ADVANCED_FACE('',(#2531),#702,.F.);
#38220=ADVANCED_FACE('',(#2532),#37827,.T.);
#38221=ADVANCED_FACE('',(#2533),#37828,.T.);
#38222=ADVANCED_FACE('',(#2534),#703,.F.);
#38223=ADVANCED_FACE('',(#2535),#704,.T.);
#38224=ADVANCED_FACE('',(#2536),#37829,.F.);
#38225=ADVANCED_FACE('',(#2537),#37830,.F.);
#38226=ADVANCED_FACE('',(#2538),#705,.F.);
#38227=ADVANCED_FACE('',(#2539),#706,.F.);
#38228=ADVANCED_FACE('',(#2540,#200),#707,.F.);
#38229=ADVANCED_FACE('',(#2541),#37831,.T.);
#38230=ADVANCED_FACE('',(#2542),#37832,.T.);
#38231=ADVANCED_FACE('',(#2543),#37833,.F.);
#38232=ADVANCED_FACE('',(#2544),#37834,.F.);
#38233=ADVANCED_FACE('',(#2545),#708,.T.);
#38234=ADVANCED_FACE('',(#2546),#709,.T.);
#38235=ADVANCED_FACE('',(#2547,#201),#710,.T.);
#38236=ADVANCED_FACE('',(#2548),#711,.T.);
#38237=ADVANCED_FACE('',(#2549),#712,.F.);
#38238=ADVANCED_FACE('',(#2550),#37835,.T.);
#38239=ADVANCED_FACE('',(#2551),#37836,.T.);
#38240=ADVANCED_FACE('',(#2552),#713,.F.);
#38241=ADVANCED_FACE('',(#2553),#714,.T.);
#38242=ADVANCED_FACE('',(#2554),#37837,.F.);
#38243=ADVANCED_FACE('',(#2555),#37838,.F.);
#38244=ADVANCED_FACE('',(#2556),#715,.F.);
#38245=ADVANCED_FACE('',(#2557),#716,.F.);
#38246=ADVANCED_FACE('',(#2558,#202),#717,.F.);
#38247=ADVANCED_FACE('',(#2559),#37839,.T.);
#38248=ADVANCED_FACE('',(#2560),#37840,.T.);
#38249=ADVANCED_FACE('',(#2561),#37841,.F.);
#38250=ADVANCED_FACE('',(#2562),#37842,.F.);
#38251=ADVANCED_FACE('',(#2563),#718,.T.);
#38252=ADVANCED_FACE('',(#2564),#719,.T.);
#38253=ADVANCED_FACE('',(#2565,#203),#720,.T.);
#38254=ADVANCED_FACE('',(#2566,#204,#205,#206,#207,#208,#209,#210,#211,
#212,#213,#214,#215,#216,#217,#218,#219,#220,#221),#721,.T.);
#38255=ADVANCED_FACE('',(#2567),#2300,.F.);
#38256=ADVANCED_FACE('',(#2568),#722,.T.);
#38257=ADVANCED_FACE('',(#2569),#723,.T.);
#38258=ADVANCED_FACE('',(#2570),#724,.T.);
#38259=ADVANCED_FACE('',(#2571),#725,.T.);
#38260=ADVANCED_FACE('',(#2572),#726,.T.);
#38261=ADVANCED_FACE('',(#2573),#727,.T.);
#38262=ADVANCED_FACE('',(#2574),#728,.T.);
#38263=ADVANCED_FACE('',(#2575),#729,.T.);
#38264=ADVANCED_FACE('',(#2576),#730,.T.);
#38265=ADVANCED_FACE('',(#2577),#731,.T.);
#38266=ADVANCED_FACE('',(#2578),#732,.T.);
#38267=ADVANCED_FACE('',(#2579),#2301,.T.);
#38268=ADVANCED_FACE('',(#2580),#2302,.T.);
#38269=ADVANCED_FACE('',(#2581),#2303,.T.);
#38270=ADVANCED_FACE('',(#2582),#2304,.T.);
#38271=ADVANCED_FACE('',(#2583),#2305,.T.);
#38272=ADVANCED_FACE('',(#2584),#2306,.T.);
#38273=ADVANCED_FACE('',(#2585),#2307,.T.);
#38274=ADVANCED_FACE('',(#2586),#2308,.T.);
#38275=ADVANCED_FACE('',(#2587),#2309,.T.);
#38276=ADVANCED_FACE('',(#2588),#2310,.T.);
#38277=ADVANCED_FACE('',(#2589),#2311,.T.);
#38278=ADVANCED_FACE('',(#2590),#2312,.T.);
#38279=ADVANCED_FACE('',(#2591),#2313,.T.);
#38280=ADVANCED_FACE('',(#2592),#2314,.T.);
#38281=ADVANCED_FACE('',(#2593),#2315,.T.);
#38282=ADVANCED_FACE('',(#2594),#2316,.T.);
#38283=ADVANCED_FACE('',(#2595),#2317,.T.);
#38284=ADVANCED_FACE('',(#2596),#2318,.T.);
#38285=ADVANCED_FACE('',(#2597),#2319,.T.);
#38286=ADVANCED_FACE('',(#2598),#2320,.T.);
#38287=ADVANCED_FACE('',(#2599),#2321,.T.);
#38288=ADVANCED_FACE('',(#2600),#2322,.T.);
#38289=ADVANCED_FACE('',(#2601),#2323,.T.);
#38290=ADVANCED_FACE('',(#2602),#2324,.T.);
#38291=ADVANCED_FACE('',(#2603),#2325,.T.);
#38292=ADVANCED_FACE('',(#2604),#2326,.T.);
#38293=ADVANCED_FACE('',(#2605),#2327,.T.);
#38294=ADVANCED_FACE('',(#2606),#2328,.T.);
#38295=ADVANCED_FACE('',(#2607),#2329,.T.);
#38296=ADVANCED_FACE('',(#2608),#2330,.T.);
#38297=ADVANCED_FACE('',(#2609),#37843,.F.);
#38298=ADVANCED_FACE('',(#2610),#37844,.F.);
#38299=ADVANCED_FACE('',(#2611),#37845,.F.);
#38300=ADVANCED_FACE('',(#2612),#37846,.F.);
#38301=ADVANCED_FACE('',(#2613),#37847,.F.);
#38302=ADVANCED_FACE('',(#2614),#37848,.F.);
#38303=ADVANCED_FACE('',(#2615),#37849,.F.);
#38304=ADVANCED_FACE('',(#2616),#37850,.F.);
#38305=ADVANCED_FACE('',(#2617),#37851,.F.);
#38306=ADVANCED_FACE('',(#2618),#37852,.F.);
#38307=ADVANCED_FACE('',(#2619),#37853,.F.);
#38308=ADVANCED_FACE('',(#2620),#37854,.F.);
#38309=ADVANCED_FACE('',(#2621),#37855,.F.);
#38310=ADVANCED_FACE('',(#2622),#37856,.F.);
#38311=ADVANCED_FACE('',(#2623),#37857,.F.);
#38312=ADVANCED_FACE('',(#2624),#37858,.F.);
#38313=ADVANCED_FACE('',(#2625),#37859,.F.);
#38314=ADVANCED_FACE('',(#2626),#37860,.F.);
#38315=ADVANCED_FACE('',(#2627),#37861,.F.);
#38316=ADVANCED_FACE('',(#2628),#37862,.F.);
#38317=ADVANCED_FACE('',(#2629),#37863,.F.);
#38318=ADVANCED_FACE('',(#2630),#37864,.F.);
#38319=ADVANCED_FACE('',(#2631),#37865,.F.);
#38320=ADVANCED_FACE('',(#2632),#37866,.F.);
#38321=ADVANCED_FACE('',(#2633),#37867,.F.);
#38322=ADVANCED_FACE('',(#2634),#37868,.F.);
#38323=ADVANCED_FACE('',(#2635),#37869,.F.);
#38324=ADVANCED_FACE('',(#2636),#37870,.F.);
#38325=ADVANCED_FACE('',(#2637),#37871,.F.);
#38326=ADVANCED_FACE('',(#2638),#37872,.F.);
#38327=ADVANCED_FACE('',(#2639),#37873,.F.);
#38328=ADVANCED_FACE('',(#2640),#37874,.F.);
#38329=ADVANCED_FACE('',(#2641),#37875,.F.);
#38330=ADVANCED_FACE('',(#2642),#37876,.F.);
#38331=ADVANCED_FACE('',(#2643),#37877,.F.);
#38332=ADVANCED_FACE('',(#2644),#37878,.F.);
#38333=ADVANCED_FACE('',(#2645),#37879,.F.);
#38334=ADVANCED_FACE('',(#2646),#37880,.F.);
#38335=ADVANCED_FACE('',(#2647),#37881,.F.);
#38336=ADVANCED_FACE('',(#2648),#37882,.F.);
#38337=ADVANCED_FACE('',(#2649),#37883,.F.);
#38338=ADVANCED_FACE('',(#2650),#37884,.F.);
#38339=ADVANCED_FACE('',(#2651),#37885,.F.);
#38340=ADVANCED_FACE('',(#2652),#37886,.F.);
#38341=ADVANCED_FACE('',(#2653),#37887,.F.);
#38342=ADVANCED_FACE('',(#2654),#37888,.F.);
#38343=ADVANCED_FACE('',(#2655),#37889,.F.);
#38344=ADVANCED_FACE('',(#2656),#37890,.F.);
#38345=ADVANCED_FACE('',(#2657),#37891,.F.);
#38346=ADVANCED_FACE('',(#2658),#37892,.F.);
#38347=ADVANCED_FACE('',(#2659),#37893,.F.);
#38348=ADVANCED_FACE('',(#2660),#37894,.F.);
#38349=ADVANCED_FACE('',(#2661),#37895,.F.);
#38350=ADVANCED_FACE('',(#2662),#37896,.F.);
#38351=ADVANCED_FACE('',(#2663),#37897,.F.);
#38352=ADVANCED_FACE('',(#2664),#733,.F.);
#38353=ADVANCED_FACE('',(#2665),#37898,.F.);
#38354=ADVANCED_FACE('',(#2666),#734,.F.);
#38355=ADVANCED_FACE('',(#2667),#37899,.F.);
#38356=ADVANCED_FACE('',(#2668),#735,.F.);
#38357=ADVANCED_FACE('',(#2669),#37900,.F.);
#38358=ADVANCED_FACE('',(#2670),#736,.F.);
#38359=ADVANCED_FACE('',(#2671),#37901,.F.);
#38360=ADVANCED_FACE('',(#2672),#737,.F.);
#38361=ADVANCED_FACE('',(#2673),#37902,.F.);
#38362=ADVANCED_FACE('',(#2674),#738,.F.);
#38363=ADVANCED_FACE('',(#2675),#739,.F.);
#38364=ADVANCED_FACE('',(#2676),#740,.F.);
#38365=ADVANCED_FACE('',(#2677),#741,.F.);
#38366=ADVANCED_FACE('',(#2678),#742,.F.);
#38367=ADVANCED_FACE('',(#2679),#743,.F.);
#38368=ADVANCED_FACE('',(#2680),#744,.T.);
#38369=ADVANCED_FACE('',(#2681),#745,.F.);
#38370=ADVANCED_FACE('',(#2682),#746,.F.);
#38371=ADVANCED_FACE('',(#2683),#747,.F.);
#38372=ADVANCED_FACE('',(#2684),#37903,.F.);
#38373=ADVANCED_FACE('',(#2685),#748,.T.);
#38374=ADVANCED_FACE('',(#2686),#749,.F.);
#38375=ADVANCED_FACE('',(#2687),#750,.T.);
#38376=ADVANCED_FACE('',(#2688),#37904,.F.);
#38377=ADVANCED_FACE('',(#2689),#751,.F.);
#38378=ADVANCED_FACE('',(#2690),#752,.T.);
#38379=ADVANCED_FACE('',(#2691),#37905,.F.);
#38380=ADVANCED_FACE('',(#2692),#753,.F.);
#38381=ADVANCED_FACE('',(#2693),#37906,.F.);
#38382=ADVANCED_FACE('',(#2694),#754,.T.);
#38383=ADVANCED_FACE('',(#2695),#755,.F.);
#38384=ADVANCED_FACE('',(#2696),#756,.T.);
#38385=ADVANCED_FACE('',(#2697),#37907,.F.);
#38386=ADVANCED_FACE('',(#2698),#757,.F.);
#38387=ADVANCED_FACE('',(#2699),#37908,.F.);
#38388=ADVANCED_FACE('',(#2700),#758,.T.);
#38389=ADVANCED_FACE('',(#2701),#759,.F.);
#38390=ADVANCED_FACE('',(#2702),#37909,.F.);
#38391=ADVANCED_FACE('',(#2703),#760,.T.);
#38392=ADVANCED_FACE('',(#2704),#761,.F.);
#38393=ADVANCED_FACE('',(#2705),#762,.T.);
#38394=ADVANCED_FACE('',(#2706),#37910,.F.);
#38395=ADVANCED_FACE('',(#2707),#763,.F.);
#38396=ADVANCED_FACE('',(#2708),#764,.T.);
#38397=ADVANCED_FACE('',(#2709),#37911,.F.);
#38398=ADVANCED_FACE('',(#2710),#765,.F.);
#38399=ADVANCED_FACE('',(#2711),#766,.T.);
#38400=ADVANCED_FACE('',(#2712),#37912,.F.);
#38401=ADVANCED_FACE('',(#2713),#767,.F.);
#38402=ADVANCED_FACE('',(#2714),#768,.T.);
#38403=ADVANCED_FACE('',(#2715),#37913,.F.);
#38404=ADVANCED_FACE('',(#2716),#769,.F.);
#38405=ADVANCED_FACE('',(#2717),#37914,.F.);
#38406=ADVANCED_FACE('',(#2718),#770,.T.);
#38407=ADVANCED_FACE('',(#2719),#771,.F.);
#38408=ADVANCED_FACE('',(#2720),#37915,.F.);
#38409=ADVANCED_FACE('',(#2721),#772,.T.);
#38410=ADVANCED_FACE('',(#2722),#773,.F.);
#38411=ADVANCED_FACE('',(#2723),#37916,.F.);
#38412=ADVANCED_FACE('',(#2724),#774,.T.);
#38413=ADVANCED_FACE('',(#2725),#775,.F.);
#38414=ADVANCED_FACE('',(#2726),#37917,.F.);
#38415=ADVANCED_FACE('',(#2727),#776,.T.);
#38416=ADVANCED_FACE('',(#2728),#777,.F.);
#38417=ADVANCED_FACE('',(#2729),#37918,.F.);
#38418=ADVANCED_FACE('',(#2730),#778,.T.);
#38419=ADVANCED_FACE('',(#2731),#779,.F.);
#38420=ADVANCED_FACE('',(#2732),#37919,.F.);
#38421=ADVANCED_FACE('',(#2733),#780,.T.);
#38422=ADVANCED_FACE('',(#2734),#781,.F.);
#38423=ADVANCED_FACE('',(#2735),#37920,.F.);
#38424=ADVANCED_FACE('',(#2736),#782,.T.);
#38425=ADVANCED_FACE('',(#2737),#783,.F.);
#38426=ADVANCED_FACE('',(#2738),#784,.T.);
#38427=ADVANCED_FACE('',(#2739),#37921,.F.);
#38428=ADVANCED_FACE('',(#2740),#785,.F.);
#38429=ADVANCED_FACE('',(#2741),#786,.T.);
#38430=ADVANCED_FACE('',(#2742),#37922,.F.);
#38431=ADVANCED_FACE('',(#2743),#787,.F.);
#38432=ADVANCED_FACE('',(#2744),#788,.T.);
#38433=ADVANCED_FACE('',(#2745),#37923,.F.);
#38434=ADVANCED_FACE('',(#2746),#789,.F.);
#38435=ADVANCED_FACE('',(#2747),#790,.T.);
#38436=ADVANCED_FACE('',(#2748),#37924,.F.);
#38437=ADVANCED_FACE('',(#2749),#791,.F.);
#38438=ADVANCED_FACE('',(#2750),#792,.T.);
#38439=ADVANCED_FACE('',(#2751),#37925,.F.);
#38440=ADVANCED_FACE('',(#2752),#793,.F.);
#38441=ADVANCED_FACE('',(#2753),#37926,.F.);
#38442=ADVANCED_FACE('',(#2754),#794,.T.);
#38443=ADVANCED_FACE('',(#2755),#795,.F.);
#38444=ADVANCED_FACE('',(#2756),#37927,.F.);
#38445=ADVANCED_FACE('',(#2757),#796,.T.);
#38446=ADVANCED_FACE('',(#2758),#797,.T.);
#38447=ADVANCED_FACE('',(#2759),#37928,.F.);
#38448=ADVANCED_FACE('',(#2760),#798,.F.);
#38449=ADVANCED_FACE('',(#2761),#799,.T.);
#38450=ADVANCED_FACE('',(#2762),#37929,.F.);
#38451=ADVANCED_FACE('',(#2763),#800,.F.);
#38452=ADVANCED_FACE('',(#2764),#801,.F.);
#38453=ADVANCED_FACE('',(#2765),#37930,.F.);
#38454=ADVANCED_FACE('',(#2766),#802,.T.);
#38455=ADVANCED_FACE('',(#2767),#803,.T.);
#38456=ADVANCED_FACE('',(#2768),#37931,.F.);
#38457=ADVANCED_FACE('',(#2769),#804,.F.);
#38458=ADVANCED_FACE('',(#2770),#805,.F.);
#38459=ADVANCED_FACE('',(#2771),#37932,.F.);
#38460=ADVANCED_FACE('',(#2772),#806,.T.);
#38461=ADVANCED_FACE('',(#2773),#807,.F.);
#38462=ADVANCED_FACE('',(#2774),#37933,.F.);
#38463=ADVANCED_FACE('',(#2775),#808,.T.);
#38464=ADVANCED_FACE('',(#2776),#809,.T.);
#38465=ADVANCED_FACE('',(#2777),#37934,.F.);
#38466=ADVANCED_FACE('',(#2778),#810,.F.);
#38467=ADVANCED_FACE('',(#2779),#811,.T.);
#38468=ADVANCED_FACE('',(#2780),#37935,.F.);
#38469=ADVANCED_FACE('',(#2781),#812,.F.);
#38470=ADVANCED_FACE('',(#2782),#813,.T.);
#38471=ADVANCED_FACE('',(#2783),#37936,.F.);
#38472=ADVANCED_FACE('',(#2784),#814,.F.);
#38473=ADVANCED_FACE('',(#2785),#815,.T.);
#38474=ADVANCED_FACE('',(#2786),#37937,.F.);
#38475=ADVANCED_FACE('',(#2787),#816,.F.);
#38476=ADVANCED_FACE('',(#2788),#817,.F.);
#38477=ADVANCED_FACE('',(#2789),#37938,.F.);
#38478=ADVANCED_FACE('',(#2790),#818,.T.);
#38479=ADVANCED_FACE('',(#2791),#819,.F.);
#38480=ADVANCED_FACE('',(#2792),#37939,.F.);
#38481=ADVANCED_FACE('',(#2793),#820,.T.);
#38482=ADVANCED_FACE('',(#2794),#821,.F.);
#38483=ADVANCED_FACE('',(#2795),#37940,.F.);
#38484=ADVANCED_FACE('',(#2796),#822,.T.);
#38485=ADVANCED_FACE('',(#2797),#823,.F.);
#38486=ADVANCED_FACE('',(#2798),#37941,.F.);
#38487=ADVANCED_FACE('',(#2799),#824,.T.);
#38488=ADVANCED_FACE('',(#2800),#825,.F.);
#38489=ADVANCED_FACE('',(#2801),#37942,.F.);
#38490=ADVANCED_FACE('',(#2802),#826,.T.);
#38491=ADVANCED_FACE('',(#2803),#827,.F.);
#38492=ADVANCED_FACE('',(#2804),#37943,.F.);
#38493=ADVANCED_FACE('',(#2805),#828,.T.);
#38494=ADVANCED_FACE('',(#2806),#829,.F.);
#38495=ADVANCED_FACE('',(#2807),#37944,.F.);
#38496=ADVANCED_FACE('',(#2808),#830,.T.);
#38497=ADVANCED_FACE('',(#2809),#831,.T.);
#38498=ADVANCED_FACE('',(#2810),#37945,.F.);
#38499=ADVANCED_FACE('',(#2811),#832,.F.);
#38500=ADVANCED_FACE('',(#2812),#833,.T.);
#38501=ADVANCED_FACE('',(#2813),#37946,.F.);
#38502=ADVANCED_FACE('',(#2814),#834,.F.);
#38503=ADVANCED_FACE('',(#2815),#835,.T.);
#38504=ADVANCED_FACE('',(#2816),#37947,.F.);
#38505=ADVANCED_FACE('',(#2817),#836,.F.);
#38506=ADVANCED_FACE('',(#2818),#837,.T.);
#38507=ADVANCED_FACE('',(#2819),#37948,.F.);
#38508=ADVANCED_FACE('',(#2820),#838,.F.);
#38509=ADVANCED_FACE('',(#2821),#839,.T.);
#38510=ADVANCED_FACE('',(#2822),#37949,.F.);
#38511=ADVANCED_FACE('',(#2823),#840,.F.);
#38512=ADVANCED_FACE('',(#2824),#841,.F.);
#38513=ADVANCED_FACE('',(#2825),#37950,.F.);
#38514=ADVANCED_FACE('',(#2826),#842,.T.);
#38515=ADVANCED_FACE('',(#2827),#843,.T.);
#38516=ADVANCED_FACE('',(#2828),#844,.T.);
#38517=ADVANCED_FACE('',(#2829),#845,.T.);
#38518=ADVANCED_FACE('',(#2830),#846,.T.);
#38519=ADVANCED_FACE('',(#2831),#847,.T.);
#38520=ADVANCED_FACE('',(#2832),#848,.T.);
#38521=ADVANCED_FACE('',(#2833),#849,.T.);
#38522=ADVANCED_FACE('',(#2834),#850,.F.);
#38523=ADVANCED_FACE('',(#2835),#37951,.T.);
#38524=ADVANCED_FACE('',(#2836),#37952,.F.);
#38525=ADVANCED_FACE('',(#2837),#851,.F.);
#38526=ADVANCED_FACE('',(#2838),#852,.F.);
#38527=ADVANCED_FACE('',(#2839),#37953,.T.);
#38528=ADVANCED_FACE('',(#2840),#853,.F.);
#38529=ADVANCED_FACE('',(#2841),#37954,.T.);
#38530=ADVANCED_FACE('',(#2842),#854,.T.);
#38531=ADVANCED_FACE('',(#2843),#855,.F.);
#38532=ADVANCED_FACE('',(#2844),#37955,.T.);
#38533=ADVANCED_FACE('',(#2845),#37956,.T.);
#38534=ADVANCED_FACE('',(#2846),#856,.F.);
#38535=ADVANCED_FACE('',(#2847),#857,.T.);
#38536=ADVANCED_FACE('',(#2848),#37957,.F.);
#38537=ADVANCED_FACE('',(#2849),#37958,.F.);
#38538=ADVANCED_FACE('',(#2850),#858,.F.);
#38539=ADVANCED_FACE('',(#2851),#859,.F.);
#38540=ADVANCED_FACE('',(#2852,#222),#860,.F.);
#38541=ADVANCED_FACE('',(#2853),#37959,.T.);
#38542=ADVANCED_FACE('',(#2854),#37960,.T.);
#38543=ADVANCED_FACE('',(#2855),#37961,.F.);
#38544=ADVANCED_FACE('',(#2856),#37962,.F.);
#38545=ADVANCED_FACE('',(#2857),#861,.T.);
#38546=ADVANCED_FACE('',(#2858),#862,.T.);
#38547=ADVANCED_FACE('',(#2859,#223),#863,.T.);
#38548=ADVANCED_FACE('',(#2860),#864,.T.);
#38549=ADVANCED_FACE('',(#2861),#865,.F.);
#38550=ADVANCED_FACE('',(#2862),#37963,.T.);
#38551=ADVANCED_FACE('',(#2863),#37964,.T.);
#38552=ADVANCED_FACE('',(#2864),#866,.T.);
#38553=ADVANCED_FACE('',(#2865),#867,.F.);
#38554=ADVANCED_FACE('',(#2866),#37965,.F.);
#38555=ADVANCED_FACE('',(#2867),#37966,.F.);
#38556=ADVANCED_FACE('',(#2868),#868,.F.);
#38557=ADVANCED_FACE('',(#2869),#869,.F.);
#38558=ADVANCED_FACE('',(#2870,#224),#870,.F.);
#38559=ADVANCED_FACE('',(#2871),#37967,.T.);
#38560=ADVANCED_FACE('',(#2872),#37968,.T.);
#38561=ADVANCED_FACE('',(#2873),#37969,.F.);
#38562=ADVANCED_FACE('',(#2874),#37970,.F.);
#38563=ADVANCED_FACE('',(#2875),#871,.T.);
#38564=ADVANCED_FACE('',(#2876),#872,.T.);
#38565=ADVANCED_FACE('',(#2877,#225),#873,.T.);
#38566=ADVANCED_FACE('',(#2878),#874,.T.);
#38567=ADVANCED_FACE('',(#2879),#875,.T.);
#38568=ADVANCED_FACE('',(#2880),#876,.T.);
#38569=ADVANCED_FACE('',(#2881),#877,.T.);
#38570=ADVANCED_FACE('',(#2882),#878,.T.);
#38571=ADVANCED_FACE('',(#2883),#879,.T.);
#38572=ADVANCED_FACE('',(#2884),#880,.T.);
#38573=ADVANCED_FACE('',(#2885),#881,.F.);
#38574=ADVANCED_FACE('',(#2886),#37971,.T.);
#38575=ADVANCED_FACE('',(#2887),#37972,.F.);
#38576=ADVANCED_FACE('',(#2888),#882,.T.);
#38577=ADVANCED_FACE('',(#2889),#883,.T.);
#38578=ADVANCED_FACE('',(#2890),#884,.F.);
#38579=ADVANCED_FACE('',(#2891),#885,.T.);
#38580=ADVANCED_FACE('',(#2892),#37973,.T.);
#38581=ADVANCED_FACE('',(#2893),#886,.T.);
#38582=ADVANCED_FACE('',(#2894),#37974,.T.);
#38583=ADVANCED_FACE('',(#2895),#37975,.F.);
#38584=ADVANCED_FACE('',(#2896),#37976,.F.);
#38585=ADVANCED_FACE('',(#2897),#37977,.F.);
#38586=ADVANCED_FACE('',(#2898),#31,.F.);
#38587=ADVANCED_FACE('',(#2899),#32,.F.);
#38588=ADVANCED_FACE('',(#2900),#37978,.F.);
#38589=ADVANCED_FACE('',(#2901),#37979,.T.);
#38590=ADVANCED_FACE('',(#2902),#37980,.F.);
#38591=ADVANCED_FACE('',(#2903,#226,#227,#228),#887,.T.);
#38592=ADVANCED_FACE('',(#2904),#888,.F.);
#38593=ADVANCED_FACE('',(#2905),#889,.T.);
#38594=ADVANCED_FACE('',(#2906),#890,.T.);
#38595=ADVANCED_FACE('',(#2907),#891,.F.);
#38596=ADVANCED_FACE('',(#2908),#892,.F.);
#38597=ADVANCED_FACE('',(#2909),#893,.T.);
#38598=ADVANCED_FACE('',(#2910),#894,.F.);
#38599=ADVANCED_FACE('',(#2911),#895,.T.);
#38600=ADVANCED_FACE('',(#2912),#896,.F.);
#38601=ADVANCED_FACE('',(#2913),#897,.T.);
#38602=ADVANCED_FACE('',(#2914),#898,.T.);
#38603=ADVANCED_FACE('',(#2915),#899,.F.);
#38604=ADVANCED_FACE('',(#2916,#229,#230,#231),#900,.F.);
#38605=ADVANCED_FACE('',(#2917,#232),#901,.F.);
#38606=ADVANCED_FACE('',(#2918,#233,#234,#235),#902,.T.);
#38607=ADVANCED_FACE('',(#2919),#37981,.T.);
#38608=ADVANCED_FACE('',(#2920),#903,.F.);
#38609=ADVANCED_FACE('',(#2921),#37982,.T.);
#38610=ADVANCED_FACE('',(#2922),#904,.F.);
#38611=ADVANCED_FACE('',(#2923),#37983,.T.);
#38612=ADVANCED_FACE('',(#2924),#905,.T.);
#38613=ADVANCED_FACE('',(#2925),#37984,.T.);
#38614=ADVANCED_FACE('',(#2926),#906,.T.);
#38615=ADVANCED_FACE('',(#2927),#907,.T.);
#38616=ADVANCED_FACE('',(#2928),#37985,.T.);
#38617=ADVANCED_FACE('',(#2929),#908,.T.);
#38618=ADVANCED_FACE('',(#2930,#236),#909,.F.);
#38619=ADVANCED_FACE('',(#2931),#910,.F.);
#38620=ADVANCED_FACE('',(#2932),#911,.F.);
#38621=ADVANCED_FACE('',(#2933,#237),#912,.F.);
#38622=ADVANCED_FACE('',(#2934),#2185,.T.);
#38623=ADVANCED_FACE('',(#2935),#37986,.T.);
#38624=ADVANCED_FACE('',(#2936),#37987,.T.);
#38625=ADVANCED_FACE('',(#2937),#2186,.T.);
#38626=ADVANCED_FACE('',(#2938),#2187,.T.);
#38627=ADVANCED_FACE('',(#2939),#37988,.T.);
#38628=ADVANCED_FACE('',(#2940),#37989,.T.);
#38629=ADVANCED_FACE('',(#2941),#2188,.T.);
#38630=ADVANCED_FACE('',(#2942),#37990,.T.);
#38631=ADVANCED_FACE('',(#2943),#913,.F.);
#38632=ADVANCED_FACE('',(#2944),#37991,.T.);
#38633=ADVANCED_FACE('',(#2945),#914,.T.);
#38634=ADVANCED_FACE('',(#2946),#37992,.T.);
#38635=ADVANCED_FACE('',(#2947),#915,.F.);
#38636=ADVANCED_FACE('',(#2948),#37993,.T.);
#38637=ADVANCED_FACE('',(#2949),#916,.F.);
#38638=ADVANCED_FACE('',(#2950),#37994,.T.);
#38639=ADVANCED_FACE('',(#2951),#917,.T.);
#38640=ADVANCED_FACE('',(#2952),#37995,.T.);
#38641=ADVANCED_FACE('',(#2953),#918,.T.);
#38642=ADVANCED_FACE('',(#2954),#37996,.F.);
#38643=ADVANCED_FACE('',(#2955),#919,.F.);
#38644=ADVANCED_FACE('',(#2956),#37997,.F.);
#38645=ADVANCED_FACE('',(#2957),#920,.F.);
#38646=ADVANCED_FACE('',(#2958),#37998,.F.);
#38647=ADVANCED_FACE('',(#2959),#921,.T.);
#38648=ADVANCED_FACE('',(#2960),#37999,.F.);
#38649=ADVANCED_FACE('',(#2961),#922,.F.);
#38650=ADVANCED_FACE('',(#2962),#38000,.F.);
#38651=ADVANCED_FACE('',(#2963),#923,.T.);
#38652=ADVANCED_FACE('',(#2964),#38001,.F.);
#38653=ADVANCED_FACE('',(#2965),#924,.T.);
#38654=ADVANCED_FACE('',(#2966),#925,.F.);
#38655=ADVANCED_FACE('',(#2967),#926,.F.);
#38656=ADVANCED_FACE('',(#2968),#927,.T.);
#38657=ADVANCED_FACE('',(#2969),#928,.F.);
#38658=ADVANCED_FACE('',(#2970),#929,.T.);
#38659=ADVANCED_FACE('',(#2971),#930,.F.);
#38660=ADVANCED_FACE('',(#2972),#931,.T.);
#38661=ADVANCED_FACE('',(#2973),#932,.T.);
#38662=ADVANCED_FACE('',(#2974),#933,.F.);
#38663=ADVANCED_FACE('',(#2975,#238),#934,.F.);
#38664=ADVANCED_FACE('',(#2976),#935,.F.);
#38665=ADVANCED_FACE('',(#2977),#936,.T.);
#38666=ADVANCED_FACE('',(#2978),#937,.F.);
#38667=ADVANCED_FACE('',(#2979),#938,.T.);
#38668=ADVANCED_FACE('',(#2980),#939,.T.);
#38669=ADVANCED_FACE('',(#2981),#940,.F.);
#38670=ADVANCED_FACE('',(#2982),#941,.F.);
#38671=ADVANCED_FACE('',(#2983),#942,.F.);
#38672=ADVANCED_FACE('',(#2984,#239),#943,.T.);
#38673=ADVANCED_FACE('',(#2985),#944,.F.);
#38674=ADVANCED_FACE('',(#2986,#240),#945,.F.);
#38675=ADVANCED_FACE('',(#2987),#946,.T.);
#38676=ADVANCED_FACE('',(#2988),#947,.F.);
#38677=ADVANCED_FACE('',(#2989),#948,.T.);
#38678=ADVANCED_FACE('',(#2990),#949,.F.);
#38679=ADVANCED_FACE('',(#2991,#241),#950,.T.);
#38680=ADVANCED_FACE('',(#2992),#951,.F.);
#38681=ADVANCED_FACE('',(#2993),#952,.T.);
#38682=ADVANCED_FACE('',(#2994),#953,.F.);
#38683=ADVANCED_FACE('',(#2995),#954,.T.);
#38684=ADVANCED_FACE('',(#2996),#955,.T.);
#38685=ADVANCED_FACE('',(#2997,#242),#956,.T.);
#38686=ADVANCED_FACE('',(#2998,#243),#957,.F.);
#38687=ADVANCED_FACE('',(#2999,#244),#958,.F.);
#38688=ADVANCED_FACE('',(#3000),#959,.T.);
#38689=ADVANCED_FACE('',(#3001),#960,.F.);
#38690=ADVANCED_FACE('',(#3002),#961,.T.);
#38691=ADVANCED_FACE('',(#3003),#962,.F.);
#38692=ADVANCED_FACE('',(#3004),#963,.T.);
#38693=ADVANCED_FACE('',(#3005),#964,.T.);
#38694=ADVANCED_FACE('',(#3006),#965,.F.);
#38695=ADVANCED_FACE('',(#3007),#966,.F.);
#38696=ADVANCED_FACE('',(#3008),#967,.F.);
#38697=ADVANCED_FACE('',(#3009,#245),#968,.F.);
#38698=ADVANCED_FACE('',(#3010,#246),#969,.T.);
#38699=ADVANCED_FACE('',(#3011),#970,.F.);
#38700=ADVANCED_FACE('',(#3012),#971,.F.);
#38701=ADVANCED_FACE('',(#3013),#972,.F.);
#38702=ADVANCED_FACE('',(#3014),#973,.F.);
#38703=ADVANCED_FACE('',(#3015),#974,.F.);
#38704=ADVANCED_FACE('',(#3016),#975,.F.);
#38705=ADVANCED_FACE('',(#3017),#38002,.F.);
#38706=ADVANCED_FACE('',(#3018),#38003,.F.);
#38707=ADVANCED_FACE('',(#3019),#38004,.F.);
#38708=ADVANCED_FACE('',(#3020),#976,.F.);
#38709=ADVANCED_FACE('',(#3021),#977,.T.);
#38710=ADVANCED_FACE('',(#3022),#978,.F.);
#38711=ADVANCED_FACE('',(#3023),#979,.T.);
#38712=ADVANCED_FACE('',(#3024),#980,.T.);
#38713=ADVANCED_FACE('',(#3025),#981,.F.);
#38714=ADVANCED_FACE('',(#3026),#982,.T.);
#38715=ADVANCED_FACE('',(#3027),#983,.F.);
#38716=ADVANCED_FACE('',(#3028,#247,#248),#984,.T.);
#38717=ADVANCED_FACE('',(#3029,#249),#985,.F.);
#38718=ADVANCED_FACE('',(#3030),#986,.F.);
#38719=ADVANCED_FACE('',(#3031),#987,.F.);
#38720=ADVANCED_FACE('',(#3032),#988,.T.);
#38721=ADVANCED_FACE('',(#3033),#989,.T.);
#38722=ADVANCED_FACE('',(#3034,#250),#990,.T.);
#38723=ADVANCED_FACE('',(#3035),#991,.F.);
#38724=ADVANCED_FACE('',(#3036),#992,.F.);
#38725=ADVANCED_FACE('',(#3037),#993,.F.);
#38726=ADVANCED_FACE('',(#3038),#994,.F.);
#38727=ADVANCED_FACE('',(#3039),#995,.T.);
#38728=ADVANCED_FACE('',(#3040),#996,.F.);
#38729=ADVANCED_FACE('',(#3041),#997,.T.);
#38730=ADVANCED_FACE('',(#3042),#998,.F.);
#38731=ADVANCED_FACE('',(#3043),#999,.F.);
#38732=ADVANCED_FACE('',(#3044),#1000,.T.);
#38733=ADVANCED_FACE('',(#3045),#1001,.F.);
#38734=ADVANCED_FACE('',(#3046),#1002,.T.);
#38735=ADVANCED_FACE('',(#3047),#1003,.F.);
#38736=ADVANCED_FACE('',(#3048),#1004,.F.);
#38737=ADVANCED_FACE('',(#3049,#251),#1005,.T.);
#38738=ADVANCED_FACE('',(#3050,#252),#1006,.F.);
#38739=ADVANCED_FACE('',(#3051),#1007,.T.);
#38740=ADVANCED_FACE('',(#3052,#253),#1008,.T.);
#38741=ADVANCED_FACE('',(#3053,#254),#1009,.F.);
#38742=ADVANCED_FACE('',(#3054),#1010,.T.);
#38743=ADVANCED_FACE('',(#3055),#1011,.F.);
#38744=ADVANCED_FACE('',(#3056),#1012,.F.);
#38745=ADVANCED_FACE('',(#3057),#1013,.F.);
#38746=ADVANCED_FACE('',(#3058),#1014,.F.);
#38747=ADVANCED_FACE('',(#3059),#38005,.F.);
#38748=ADVANCED_FACE('',(#3060),#38006,.F.);
#38749=ADVANCED_FACE('',(#3061),#1015,.F.);
#38750=ADVANCED_FACE('',(#3062),#1016,.F.);
#38751=ADVANCED_FACE('',(#3063),#1017,.T.);
#38752=ADVANCED_FACE('',(#3064),#1018,.T.);
#38753=ADVANCED_FACE('',(#3065),#1019,.T.);
#38754=ADVANCED_FACE('',(#3066),#1020,.T.);
#38755=ADVANCED_FACE('',(#3067),#1021,.F.);
#38756=ADVANCED_FACE('',(#3068),#1022,.F.);
#38757=ADVANCED_FACE('',(#3069),#1023,.F.);
#38758=ADVANCED_FACE('',(#3070),#1024,.F.);
#38759=ADVANCED_FACE('',(#3071),#1025,.F.);
#38760=ADVANCED_FACE('',(#3072),#1026,.F.);
#38761=ADVANCED_FACE('',(#3073),#1027,.F.);
#38762=ADVANCED_FACE('',(#3074),#1028,.F.);
#38763=ADVANCED_FACE('',(#3075),#27,.T.);
#38764=ADVANCED_FACE('',(#3076),#28,.T.);
#38765=ADVANCED_FACE('',(#3077),#2189,.F.);
#38766=ADVANCED_FACE('',(#3078),#2190,.F.);
#38767=ADVANCED_FACE('',(#3079),#2191,.T.);
#38768=ADVANCED_FACE('',(#3080),#2192,.T.);
#38769=ADVANCED_FACE('',(#3081,#255),#1029,.T.);
#38770=ADVANCED_FACE('',(#3082,#256),#1030,.F.);
#38771=ADVANCED_FACE('',(#3083),#1031,.T.);
#38772=ADVANCED_FACE('',(#3084),#1032,.T.);
#38773=ADVANCED_FACE('',(#3085),#1033,.F.);
#38774=ADVANCED_FACE('',(#3086),#1034,.T.);
#38775=ADVANCED_FACE('',(#3087),#1035,.F.);
#38776=ADVANCED_FACE('',(#3088),#1036,.T.);
#38777=ADVANCED_FACE('',(#3089),#1037,.T.);
#38778=ADVANCED_FACE('',(#3090),#1038,.F.);
#38779=ADVANCED_FACE('',(#3091),#1039,.T.);
#38780=ADVANCED_FACE('',(#3092),#1040,.T.);
#38781=ADVANCED_FACE('',(#3093),#38007,.T.);
#38782=ADVANCED_FACE('',(#3094),#38008,.F.);
#38783=ADVANCED_FACE('',(#3095),#1041,.T.);
#38784=ADVANCED_FACE('',(#3096),#1042,.T.);
#38785=ADVANCED_FACE('',(#3097),#38009,.T.);
#38786=ADVANCED_FACE('',(#3098),#38010,.F.);
#38787=ADVANCED_FACE('',(#3099),#38011,.T.);
#38788=ADVANCED_FACE('',(#3100),#1043,.F.);
#38789=ADVANCED_FACE('',(#3101),#38012,.T.);
#38790=ADVANCED_FACE('',(#3102),#1044,.F.);
#38791=ADVANCED_FACE('',(#3103),#1045,.F.);
#38792=ADVANCED_FACE('',(#3104),#1046,.F.);
#38793=ADVANCED_FACE('',(#3105),#1047,.T.);
#38794=ADVANCED_FACE('',(#3106),#1048,.T.);
#38795=ADVANCED_FACE('',(#3107),#1049,.T.);
#38796=ADVANCED_FACE('',(#3108),#1050,.T.);
#38797=ADVANCED_FACE('',(#3109),#1051,.T.);
#38798=ADVANCED_FACE('',(#3110),#1052,.T.);
#38799=ADVANCED_FACE('',(#3111),#38013,.T.);
#38800=ADVANCED_FACE('',(#3112),#38014,.F.);
#38801=ADVANCED_FACE('',(#3113),#1053,.T.);
#38802=ADVANCED_FACE('',(#3114),#1054,.T.);
#38803=ADVANCED_FACE('',(#3115),#38015,.T.);
#38804=ADVANCED_FACE('',(#3116),#38016,.F.);
#38805=ADVANCED_FACE('',(#3117),#38017,.T.);
#38806=ADVANCED_FACE('',(#3118),#1055,.T.);
#38807=ADVANCED_FACE('',(#3119),#38018,.T.);
#38808=ADVANCED_FACE('',(#3120),#1056,.F.);
#38809=ADVANCED_FACE('',(#3121),#1057,.F.);
#38810=ADVANCED_FACE('',(#3122),#1058,.F.);
#38811=ADVANCED_FACE('',(#3123),#1059,.T.);
#38812=ADVANCED_FACE('',(#3124),#1060,.T.);
#38813=ADVANCED_FACE('',(#3125),#1061,.F.);
#38814=ADVANCED_FACE('',(#3126),#1062,.T.);
#38815=ADVANCED_FACE('',(#3127,#257,#258,#259,#260,#261,#262,#263,#264,
#265,#266,#267,#268,#269,#270,#271,#272,#273,#274,#275,#276,#277,#278,#279,
#280,#281,#282,#283,#284,#285,#286,#287,#288,#289,#290,#291,#292,#293,#294,
#295,#296,#297,#298,#299,#300,#301,#302,#303,#304,#305,#306,#307,#308,#309,
#310,#311,#312,#313,#314,#315,#316,#317,#318,#319,#320,#321,#322,#323,#324,
#325,#326,#327,#328,#329,#330,#331,#332,#333,#334,#335,#336,#337,#338,#339,
#340,#341,#342,#343,#344,#345,#346,#347,#348,#349,#350,#351,#352,#353,#354,
#355,#356,#357,#358,#359,#360,#361,#362,#363,#364,#365,#366,#367,#368,#369,
#370,#371,#372,#373,#374,#375,#376,#377,#378,#379,#380,#381,#382,#383,#384,
#385,#386,#387,#388,#389,#390,#391,#392,#393,#394,#395,#396,#397,#398,#399,
#400,#401,#402,#403,#404,#405,#406,#407,#408,#409,#410,#411,#412,#413,#414,
#415,#416,#417,#418,#419,#420,#421,#422,#423,#424,#425,#426,#427,#428,#429,
#430,#431,#432,#433,#434,#435,#436,#437,#438,#439,#440,#441,#442),#1063,
 .T.);
#38816=ADVANCED_FACE('',(#3128,#443,#444,#445,#446,#447,#448,#449,#450,
#451,#452,#453,#454,#455,#456,#457,#458,#459,#460,#461,#462,#463,#464,#465,
#466,#467,#468,#469,#470,#471,#472,#473,#474,#475,#476,#477,#478,#479,#480,
#481,#482,#483,#484,#485,#486,#487,#488,#489,#490,#491,#492,#493,#494,#495,
#496,#497,#498,#499,#500,#501,#502,#503,#504,#505,#506,#507,#508,#509,#510,
#511,#512,#513,#514,#515,#516,#517,#518,#519,#520,#521,#522,#523,#524,#525,
#526,#527,#528,#529,#530,#531,#532,#533,#534,#535,#536,#537,#538,#539,#540,
#541,#542,#543,#544,#545,#546,#547,#548,#549,#550,#551,#552,#553,#554,#555,
#556,#557,#558,#559,#560,#561,#562,#563,#564,#565,#566,#567,#568,#569,#570,
#571,#572,#573,#574,#575,#576,#577,#578,#579,#580,#581,#582,#583,#584,#585,
#586,#587,#588,#589,#590,#591,#592,#593,#594,#595,#596,#597,#598,#599,#600,
#601,#602,#603,#604,#605,#606,#607,#608,#609,#610,#611,#612,#613,#614,#615,
#616,#617,#618,#619,#620,#621,#622,#623,#624,#625,#626,#627,#628),#1064,
 .F.);
#38817=ADVANCED_FACE('',(#3129),#1065,.F.);
#38818=ADVANCED_FACE('',(#3130),#1066,.F.);
#38819=ADVANCED_FACE('',(#3131),#1067,.F.);
#38820=ADVANCED_FACE('',(#3132),#1068,.F.);
#38821=ADVANCED_FACE('',(#3133),#1069,.F.);
#38822=ADVANCED_FACE('',(#3134),#1070,.F.);
#38823=ADVANCED_FACE('',(#3135),#1071,.F.);
#38824=ADVANCED_FACE('',(#3136),#1072,.F.);
#38825=ADVANCED_FACE('',(#3137),#1073,.F.);
#38826=ADVANCED_FACE('',(#3138),#1074,.F.);
#38827=ADVANCED_FACE('',(#3139),#1075,.F.);
#38828=ADVANCED_FACE('',(#3140),#1076,.F.);
#38829=ADVANCED_FACE('',(#3141),#1077,.F.);
#38830=ADVANCED_FACE('',(#3142),#1078,.F.);
#38831=ADVANCED_FACE('',(#3143),#1079,.F.);
#38832=ADVANCED_FACE('',(#3144),#1080,.F.);
#38833=ADVANCED_FACE('',(#3145),#1081,.F.);
#38834=ADVANCED_FACE('',(#3146),#1082,.F.);
#38835=ADVANCED_FACE('',(#3147),#1083,.F.);
#38836=ADVANCED_FACE('',(#3148),#1084,.F.);
#38837=ADVANCED_FACE('',(#3149),#1085,.F.);
#38838=ADVANCED_FACE('',(#3150),#1086,.F.);
#38839=ADVANCED_FACE('',(#3151),#1087,.F.);
#38840=ADVANCED_FACE('',(#3152),#1088,.F.);
#38841=ADVANCED_FACE('',(#3153),#1089,.F.);
#38842=ADVANCED_FACE('',(#3154),#1090,.F.);
#38843=ADVANCED_FACE('',(#3155),#1091,.F.);
#38844=ADVANCED_FACE('',(#3156),#1092,.F.);
#38845=ADVANCED_FACE('',(#3157),#1093,.F.);
#38846=ADVANCED_FACE('',(#3158),#1094,.F.);
#38847=ADVANCED_FACE('',(#3159),#1095,.F.);
#38848=ADVANCED_FACE('',(#3160),#1096,.F.);
#38849=ADVANCED_FACE('',(#3161),#1097,.F.);
#38850=ADVANCED_FACE('',(#3162),#1098,.F.);
#38851=ADVANCED_FACE('',(#3163),#1099,.F.);
#38852=ADVANCED_FACE('',(#3164),#1100,.F.);
#38853=ADVANCED_FACE('',(#3165),#1101,.F.);
#38854=ADVANCED_FACE('',(#3166),#1102,.F.);
#38855=ADVANCED_FACE('',(#3167),#1103,.F.);
#38856=ADVANCED_FACE('',(#3168),#1104,.F.);
#38857=ADVANCED_FACE('',(#3169),#1105,.F.);
#38858=ADVANCED_FACE('',(#3170),#1106,.F.);
#38859=ADVANCED_FACE('',(#3171),#1107,.F.);
#38860=ADVANCED_FACE('',(#3172),#1108,.F.);
#38861=ADVANCED_FACE('',(#3173),#1109,.F.);
#38862=ADVANCED_FACE('',(#3174),#1110,.F.);
#38863=ADVANCED_FACE('',(#3175),#1111,.F.);
#38864=ADVANCED_FACE('',(#3176),#1112,.F.);
#38865=ADVANCED_FACE('',(#3177),#1113,.F.);
#38866=ADVANCED_FACE('',(#3178),#1114,.F.);
#38867=ADVANCED_FACE('',(#3179),#1115,.F.);
#38868=ADVANCED_FACE('',(#3180),#1116,.F.);
#38869=ADVANCED_FACE('',(#3181),#1117,.F.);
#38870=ADVANCED_FACE('',(#3182),#1118,.F.);
#38871=ADVANCED_FACE('',(#3183),#1119,.F.);
#38872=ADVANCED_FACE('',(#3184),#1120,.F.);
#38873=ADVANCED_FACE('',(#3185),#1121,.F.);
#38874=ADVANCED_FACE('',(#3186),#1122,.F.);
#38875=ADVANCED_FACE('',(#3187),#1123,.F.);
#38876=ADVANCED_FACE('',(#3188),#1124,.F.);
#38877=ADVANCED_FACE('',(#3189),#1125,.F.);
#38878=ADVANCED_FACE('',(#3190),#1126,.F.);
#38879=ADVANCED_FACE('',(#3191),#1127,.F.);
#38880=ADVANCED_FACE('',(#3192),#1128,.F.);
#38881=ADVANCED_FACE('',(#3193),#1129,.F.);
#38882=ADVANCED_FACE('',(#3194),#1130,.F.);
#38883=ADVANCED_FACE('',(#3195),#1131,.F.);
#38884=ADVANCED_FACE('',(#3196),#1132,.F.);
#38885=ADVANCED_FACE('',(#3197),#1133,.F.);
#38886=ADVANCED_FACE('',(#3198),#1134,.F.);
#38887=ADVANCED_FACE('',(#3199),#1135,.F.);
#38888=ADVANCED_FACE('',(#3200),#1136,.F.);
#38889=ADVANCED_FACE('',(#3201),#1137,.F.);
#38890=ADVANCED_FACE('',(#3202),#1138,.F.);
#38891=ADVANCED_FACE('',(#3203),#1139,.F.);
#38892=ADVANCED_FACE('',(#3204),#1140,.F.);
#38893=ADVANCED_FACE('',(#3205),#1141,.F.);
#38894=ADVANCED_FACE('',(#3206),#1142,.F.);
#38895=ADVANCED_FACE('',(#3207),#1143,.F.);
#38896=ADVANCED_FACE('',(#3208),#1144,.F.);
#38897=ADVANCED_FACE('',(#3209),#1145,.F.);
#38898=ADVANCED_FACE('',(#3210),#1146,.F.);
#38899=ADVANCED_FACE('',(#3211),#1147,.F.);
#38900=ADVANCED_FACE('',(#3212),#1148,.F.);
#38901=ADVANCED_FACE('',(#3213),#1149,.F.);
#38902=ADVANCED_FACE('',(#3214),#1150,.F.);
#38903=ADVANCED_FACE('',(#3215),#1151,.F.);
#38904=ADVANCED_FACE('',(#3216),#1152,.F.);
#38905=ADVANCED_FACE('',(#3217),#1153,.F.);
#38906=ADVANCED_FACE('',(#3218),#1154,.F.);
#38907=ADVANCED_FACE('',(#3219),#1155,.F.);
#38908=ADVANCED_FACE('',(#3220),#1156,.F.);
#38909=ADVANCED_FACE('',(#3221),#1157,.F.);
#38910=ADVANCED_FACE('',(#3222),#1158,.F.);
#38911=ADVANCED_FACE('',(#3223),#1159,.F.);
#38912=ADVANCED_FACE('',(#3224),#1160,.F.);
#38913=ADVANCED_FACE('',(#3225),#1161,.F.);
#38914=ADVANCED_FACE('',(#3226),#1162,.F.);
#38915=ADVANCED_FACE('',(#3227),#1163,.F.);
#38916=ADVANCED_FACE('',(#3228),#1164,.F.);
#38917=ADVANCED_FACE('',(#3229),#1165,.F.);
#38918=ADVANCED_FACE('',(#3230),#1166,.F.);
#38919=ADVANCED_FACE('',(#3231),#1167,.F.);
#38920=ADVANCED_FACE('',(#3232),#1168,.F.);
#38921=ADVANCED_FACE('',(#3233),#1169,.F.);
#38922=ADVANCED_FACE('',(#3234),#1170,.F.);
#38923=ADVANCED_FACE('',(#3235),#1171,.F.);
#38924=ADVANCED_FACE('',(#3236),#1172,.F.);
#38925=ADVANCED_FACE('',(#3237),#1173,.F.);
#38926=ADVANCED_FACE('',(#3238),#1174,.F.);
#38927=ADVANCED_FACE('',(#3239),#1175,.F.);
#38928=ADVANCED_FACE('',(#3240),#1176,.F.);
#38929=ADVANCED_FACE('',(#3241),#1177,.F.);
#38930=ADVANCED_FACE('',(#3242),#1178,.F.);
#38931=ADVANCED_FACE('',(#3243),#1179,.F.);
#38932=ADVANCED_FACE('',(#3244),#1180,.F.);
#38933=ADVANCED_FACE('',(#3245),#1181,.F.);
#38934=ADVANCED_FACE('',(#3246),#1182,.F.);
#38935=ADVANCED_FACE('',(#3247),#1183,.F.);
#38936=ADVANCED_FACE('',(#3248),#1184,.F.);
#38937=ADVANCED_FACE('',(#3249),#1185,.F.);
#38938=ADVANCED_FACE('',(#3250),#1186,.F.);
#38939=ADVANCED_FACE('',(#3251),#1187,.F.);
#38940=ADVANCED_FACE('',(#3252),#1188,.F.);
#38941=ADVANCED_FACE('',(#3253),#1189,.F.);
#38942=ADVANCED_FACE('',(#3254),#1190,.F.);
#38943=ADVANCED_FACE('',(#3255),#1191,.F.);
#38944=ADVANCED_FACE('',(#3256),#1192,.F.);
#38945=ADVANCED_FACE('',(#3257),#1193,.F.);
#38946=ADVANCED_FACE('',(#3258),#1194,.F.);
#38947=ADVANCED_FACE('',(#3259),#1195,.F.);
#38948=ADVANCED_FACE('',(#3260),#1196,.F.);
#38949=ADVANCED_FACE('',(#3261),#1197,.F.);
#38950=ADVANCED_FACE('',(#3262),#1198,.F.);
#38951=ADVANCED_FACE('',(#3263),#1199,.F.);
#38952=ADVANCED_FACE('',(#3264),#1200,.F.);
#38953=ADVANCED_FACE('',(#3265),#1201,.F.);
#38954=ADVANCED_FACE('',(#3266),#1202,.F.);
#38955=ADVANCED_FACE('',(#3267),#1203,.F.);
#38956=ADVANCED_FACE('',(#3268),#1204,.F.);
#38957=ADVANCED_FACE('',(#3269),#1205,.F.);
#38958=ADVANCED_FACE('',(#3270),#1206,.F.);
#38959=ADVANCED_FACE('',(#3271),#1207,.F.);
#38960=ADVANCED_FACE('',(#3272),#1208,.F.);
#38961=ADVANCED_FACE('',(#3273),#1209,.F.);
#38962=ADVANCED_FACE('',(#3274),#1210,.F.);
#38963=ADVANCED_FACE('',(#3275),#1211,.F.);
#38964=ADVANCED_FACE('',(#3276),#1212,.F.);
#38965=ADVANCED_FACE('',(#3277),#1213,.F.);
#38966=ADVANCED_FACE('',(#3278),#1214,.F.);
#38967=ADVANCED_FACE('',(#3279),#1215,.F.);
#38968=ADVANCED_FACE('',(#3280),#1216,.F.);
#38969=ADVANCED_FACE('',(#3281),#1217,.F.);
#38970=ADVANCED_FACE('',(#3282),#1218,.F.);
#38971=ADVANCED_FACE('',(#3283),#1219,.F.);
#38972=ADVANCED_FACE('',(#3284),#1220,.F.);
#38973=ADVANCED_FACE('',(#3285),#1221,.F.);
#38974=ADVANCED_FACE('',(#3286),#1222,.F.);
#38975=ADVANCED_FACE('',(#3287),#1223,.F.);
#38976=ADVANCED_FACE('',(#3288),#1224,.F.);
#38977=ADVANCED_FACE('',(#3289),#1225,.F.);
#38978=ADVANCED_FACE('',(#3290),#1226,.F.);
#38979=ADVANCED_FACE('',(#3291),#1227,.F.);
#38980=ADVANCED_FACE('',(#3292),#1228,.F.);
#38981=ADVANCED_FACE('',(#3293),#1229,.F.);
#38982=ADVANCED_FACE('',(#3294),#1230,.F.);
#38983=ADVANCED_FACE('',(#3295),#1231,.F.);
#38984=ADVANCED_FACE('',(#3296),#1232,.F.);
#38985=ADVANCED_FACE('',(#3297),#1233,.F.);
#38986=ADVANCED_FACE('',(#3298),#1234,.F.);
#38987=ADVANCED_FACE('',(#3299),#1235,.F.);
#38988=ADVANCED_FACE('',(#3300),#1236,.F.);
#38989=ADVANCED_FACE('',(#3301),#1237,.F.);
#38990=ADVANCED_FACE('',(#3302),#1238,.F.);
#38991=ADVANCED_FACE('',(#3303),#1239,.F.);
#38992=ADVANCED_FACE('',(#3304),#1240,.F.);
#38993=ADVANCED_FACE('',(#3305),#1241,.F.);
#38994=ADVANCED_FACE('',(#3306),#1242,.F.);
#38995=ADVANCED_FACE('',(#3307),#1243,.F.);
#38996=ADVANCED_FACE('',(#3308),#1244,.F.);
#38997=ADVANCED_FACE('',(#3309),#1245,.F.);
#38998=ADVANCED_FACE('',(#3310),#1246,.F.);
#38999=ADVANCED_FACE('',(#3311),#1247,.F.);
#39000=ADVANCED_FACE('',(#3312),#1248,.F.);
#39001=ADVANCED_FACE('',(#3313),#1249,.F.);
#39002=ADVANCED_FACE('',(#3314),#1250,.F.);
#39003=ADVANCED_FACE('',(#3315),#1251,.F.);
#39004=ADVANCED_FACE('',(#3316),#1252,.F.);
#39005=ADVANCED_FACE('',(#3317),#1253,.F.);
#39006=ADVANCED_FACE('',(#3318),#1254,.F.);
#39007=ADVANCED_FACE('',(#3319),#1255,.F.);
#39008=ADVANCED_FACE('',(#3320),#1256,.F.);
#39009=ADVANCED_FACE('',(#3321),#1257,.F.);
#39010=ADVANCED_FACE('',(#3322),#1258,.F.);
#39011=ADVANCED_FACE('',(#3323),#1259,.F.);
#39012=ADVANCED_FACE('',(#3324),#1260,.F.);
#39013=ADVANCED_FACE('',(#3325),#1261,.F.);
#39014=ADVANCED_FACE('',(#3326),#1262,.F.);
#39015=ADVANCED_FACE('',(#3327),#1263,.F.);
#39016=ADVANCED_FACE('',(#3328),#1264,.F.);
#39017=ADVANCED_FACE('',(#3329),#1265,.F.);
#39018=ADVANCED_FACE('',(#3330),#1266,.F.);
#39019=ADVANCED_FACE('',(#3331),#1267,.F.);
#39020=ADVANCED_FACE('',(#3332),#1268,.F.);
#39021=ADVANCED_FACE('',(#3333),#1269,.F.);
#39022=ADVANCED_FACE('',(#3334),#1270,.F.);
#39023=ADVANCED_FACE('',(#3335),#1271,.F.);
#39024=ADVANCED_FACE('',(#3336),#1272,.F.);
#39025=ADVANCED_FACE('',(#3337),#1273,.F.);
#39026=ADVANCED_FACE('',(#3338),#1274,.F.);
#39027=ADVANCED_FACE('',(#3339),#1275,.F.);
#39028=ADVANCED_FACE('',(#3340),#1276,.F.);
#39029=ADVANCED_FACE('',(#3341),#1277,.F.);
#39030=ADVANCED_FACE('',(#3342),#1278,.F.);
#39031=ADVANCED_FACE('',(#3343),#1279,.F.);
#39032=ADVANCED_FACE('',(#3344),#1280,.F.);
#39033=ADVANCED_FACE('',(#3345),#1281,.F.);
#39034=ADVANCED_FACE('',(#3346),#1282,.F.);
#39035=ADVANCED_FACE('',(#3347),#1283,.F.);
#39036=ADVANCED_FACE('',(#3348),#1284,.F.);
#39037=ADVANCED_FACE('',(#3349),#1285,.F.);
#39038=ADVANCED_FACE('',(#3350),#1286,.F.);
#39039=ADVANCED_FACE('',(#3351),#1287,.F.);
#39040=ADVANCED_FACE('',(#3352),#1288,.F.);
#39041=ADVANCED_FACE('',(#3353),#1289,.F.);
#39042=ADVANCED_FACE('',(#3354),#1290,.F.);
#39043=ADVANCED_FACE('',(#3355),#1291,.F.);
#39044=ADVANCED_FACE('',(#3356),#1292,.F.);
#39045=ADVANCED_FACE('',(#3357),#1293,.F.);
#39046=ADVANCED_FACE('',(#3358),#1294,.F.);
#39047=ADVANCED_FACE('',(#3359),#1295,.F.);
#39048=ADVANCED_FACE('',(#3360),#1296,.F.);
#39049=ADVANCED_FACE('',(#3361),#1297,.F.);
#39050=ADVANCED_FACE('',(#3362),#1298,.F.);
#39051=ADVANCED_FACE('',(#3363),#1299,.F.);
#39052=ADVANCED_FACE('',(#3364),#1300,.F.);
#39053=ADVANCED_FACE('',(#3365),#1301,.F.);
#39054=ADVANCED_FACE('',(#3366),#1302,.F.);
#39055=ADVANCED_FACE('',(#3367),#1303,.F.);
#39056=ADVANCED_FACE('',(#3368),#1304,.F.);
#39057=ADVANCED_FACE('',(#3369),#1305,.F.);
#39058=ADVANCED_FACE('',(#3370),#1306,.F.);
#39059=ADVANCED_FACE('',(#3371),#1307,.F.);
#39060=ADVANCED_FACE('',(#3372),#1308,.F.);
#39061=ADVANCED_FACE('',(#3373),#1309,.F.);
#39062=ADVANCED_FACE('',(#3374),#1310,.F.);
#39063=ADVANCED_FACE('',(#3375),#1311,.F.);
#39064=ADVANCED_FACE('',(#3376),#1312,.F.);
#39065=ADVANCED_FACE('',(#3377),#1313,.F.);
#39066=ADVANCED_FACE('',(#3378),#1314,.F.);
#39067=ADVANCED_FACE('',(#3379),#1315,.F.);
#39068=ADVANCED_FACE('',(#3380),#1316,.F.);
#39069=ADVANCED_FACE('',(#3381),#1317,.F.);
#39070=ADVANCED_FACE('',(#3382),#1318,.F.);
#39071=ADVANCED_FACE('',(#3383),#1319,.F.);
#39072=ADVANCED_FACE('',(#3384),#1320,.F.);
#39073=ADVANCED_FACE('',(#3385),#1321,.F.);
#39074=ADVANCED_FACE('',(#3386),#1322,.F.);
#39075=ADVANCED_FACE('',(#3387),#1323,.F.);
#39076=ADVANCED_FACE('',(#3388),#1324,.F.);
#39077=ADVANCED_FACE('',(#3389),#1325,.F.);
#39078=ADVANCED_FACE('',(#3390),#1326,.F.);
#39079=ADVANCED_FACE('',(#3391),#1327,.F.);
#39080=ADVANCED_FACE('',(#3392),#1328,.F.);
#39081=ADVANCED_FACE('',(#3393),#1329,.F.);
#39082=ADVANCED_FACE('',(#3394),#1330,.F.);
#39083=ADVANCED_FACE('',(#3395),#1331,.F.);
#39084=ADVANCED_FACE('',(#3396),#1332,.F.);
#39085=ADVANCED_FACE('',(#3397),#1333,.F.);
#39086=ADVANCED_FACE('',(#3398),#1334,.F.);
#39087=ADVANCED_FACE('',(#3399),#1335,.F.);
#39088=ADVANCED_FACE('',(#3400),#1336,.F.);
#39089=ADVANCED_FACE('',(#3401),#1337,.F.);
#39090=ADVANCED_FACE('',(#3402),#1338,.F.);
#39091=ADVANCED_FACE('',(#3403),#1339,.F.);
#39092=ADVANCED_FACE('',(#3404),#1340,.F.);
#39093=ADVANCED_FACE('',(#3405),#1341,.F.);
#39094=ADVANCED_FACE('',(#3406),#1342,.F.);
#39095=ADVANCED_FACE('',(#3407),#1343,.F.);
#39096=ADVANCED_FACE('',(#3408),#1344,.F.);
#39097=ADVANCED_FACE('',(#3409),#1345,.F.);
#39098=ADVANCED_FACE('',(#3410),#1346,.F.);
#39099=ADVANCED_FACE('',(#3411),#1347,.F.);
#39100=ADVANCED_FACE('',(#3412),#1348,.F.);
#39101=ADVANCED_FACE('',(#3413),#1349,.F.);
#39102=ADVANCED_FACE('',(#3414),#1350,.F.);
#39103=ADVANCED_FACE('',(#3415),#1351,.F.);
#39104=ADVANCED_FACE('',(#3416),#1352,.F.);
#39105=ADVANCED_FACE('',(#3417),#1353,.F.);
#39106=ADVANCED_FACE('',(#3418),#1354,.F.);
#39107=ADVANCED_FACE('',(#3419),#1355,.F.);
#39108=ADVANCED_FACE('',(#3420),#1356,.F.);
#39109=ADVANCED_FACE('',(#3421),#1357,.F.);
#39110=ADVANCED_FACE('',(#3422),#1358,.F.);
#39111=ADVANCED_FACE('',(#3423),#1359,.F.);
#39112=ADVANCED_FACE('',(#3424),#1360,.F.);
#39113=ADVANCED_FACE('',(#3425),#1361,.F.);
#39114=ADVANCED_FACE('',(#3426),#1362,.F.);
#39115=ADVANCED_FACE('',(#3427),#1363,.F.);
#39116=ADVANCED_FACE('',(#3428),#1364,.F.);
#39117=ADVANCED_FACE('',(#3429),#1365,.F.);
#39118=ADVANCED_FACE('',(#3430),#1366,.F.);
#39119=ADVANCED_FACE('',(#3431),#1367,.F.);
#39120=ADVANCED_FACE('',(#3432),#1368,.F.);
#39121=ADVANCED_FACE('',(#3433),#1369,.F.);
#39122=ADVANCED_FACE('',(#3434),#1370,.F.);
#39123=ADVANCED_FACE('',(#3435),#1371,.F.);
#39124=ADVANCED_FACE('',(#3436),#1372,.F.);
#39125=ADVANCED_FACE('',(#3437),#1373,.F.);
#39126=ADVANCED_FACE('',(#3438),#1374,.F.);
#39127=ADVANCED_FACE('',(#3439),#1375,.F.);
#39128=ADVANCED_FACE('',(#3440),#1376,.F.);
#39129=ADVANCED_FACE('',(#3441),#1377,.F.);
#39130=ADVANCED_FACE('',(#3442),#1378,.F.);
#39131=ADVANCED_FACE('',(#3443),#1379,.F.);
#39132=ADVANCED_FACE('',(#3444),#1380,.F.);
#39133=ADVANCED_FACE('',(#3445),#1381,.F.);
#39134=ADVANCED_FACE('',(#3446),#1382,.F.);
#39135=ADVANCED_FACE('',(#3447),#1383,.F.);
#39136=ADVANCED_FACE('',(#3448),#1384,.F.);
#39137=ADVANCED_FACE('',(#3449),#1385,.F.);
#39138=ADVANCED_FACE('',(#3450),#1386,.F.);
#39139=ADVANCED_FACE('',(#3451),#1387,.F.);
#39140=ADVANCED_FACE('',(#3452),#1388,.F.);
#39141=ADVANCED_FACE('',(#3453),#1389,.F.);
#39142=ADVANCED_FACE('',(#3454),#1390,.F.);
#39143=ADVANCED_FACE('',(#3455),#1391,.F.);
#39144=ADVANCED_FACE('',(#3456),#1392,.F.);
#39145=ADVANCED_FACE('',(#3457),#1393,.F.);
#39146=ADVANCED_FACE('',(#3458),#1394,.F.);
#39147=ADVANCED_FACE('',(#3459),#1395,.F.);
#39148=ADVANCED_FACE('',(#3460),#1396,.F.);
#39149=ADVANCED_FACE('',(#3461),#1397,.F.);
#39150=ADVANCED_FACE('',(#3462),#1398,.F.);
#39151=ADVANCED_FACE('',(#3463),#1399,.F.);
#39152=ADVANCED_FACE('',(#3464),#1400,.F.);
#39153=ADVANCED_FACE('',(#3465),#1401,.F.);
#39154=ADVANCED_FACE('',(#3466),#1402,.F.);
#39155=ADVANCED_FACE('',(#3467),#1403,.F.);
#39156=ADVANCED_FACE('',(#3468),#1404,.F.);
#39157=ADVANCED_FACE('',(#3469),#1405,.F.);
#39158=ADVANCED_FACE('',(#3470),#1406,.F.);
#39159=ADVANCED_FACE('',(#3471),#1407,.F.);
#39160=ADVANCED_FACE('',(#3472),#1408,.F.);
#39161=ADVANCED_FACE('',(#3473),#1409,.F.);
#39162=ADVANCED_FACE('',(#3474),#1410,.F.);
#39163=ADVANCED_FACE('',(#3475),#1411,.F.);
#39164=ADVANCED_FACE('',(#3476),#1412,.F.);
#39165=ADVANCED_FACE('',(#3477),#1413,.F.);
#39166=ADVANCED_FACE('',(#3478),#1414,.F.);
#39167=ADVANCED_FACE('',(#3479),#1415,.F.);
#39168=ADVANCED_FACE('',(#3480),#1416,.F.);
#39169=ADVANCED_FACE('',(#3481),#1417,.F.);
#39170=ADVANCED_FACE('',(#3482),#1418,.F.);
#39171=ADVANCED_FACE('',(#3483),#1419,.F.);
#39172=ADVANCED_FACE('',(#3484),#1420,.F.);
#39173=ADVANCED_FACE('',(#3485),#1421,.F.);
#39174=ADVANCED_FACE('',(#3486),#1422,.F.);
#39175=ADVANCED_FACE('',(#3487),#1423,.F.);
#39176=ADVANCED_FACE('',(#3488),#1424,.F.);
#39177=ADVANCED_FACE('',(#3489),#1425,.F.);
#39178=ADVANCED_FACE('',(#3490),#1426,.F.);
#39179=ADVANCED_FACE('',(#3491),#1427,.F.);
#39180=ADVANCED_FACE('',(#3492),#1428,.F.);
#39181=ADVANCED_FACE('',(#3493),#1429,.F.);
#39182=ADVANCED_FACE('',(#3494),#1430,.F.);
#39183=ADVANCED_FACE('',(#3495),#1431,.F.);
#39184=ADVANCED_FACE('',(#3496),#1432,.F.);
#39185=ADVANCED_FACE('',(#3497),#1433,.F.);
#39186=ADVANCED_FACE('',(#3498),#1434,.F.);
#39187=ADVANCED_FACE('',(#3499),#1435,.F.);
#39188=ADVANCED_FACE('',(#3500),#1436,.F.);
#39189=ADVANCED_FACE('',(#3501),#1437,.F.);
#39190=ADVANCED_FACE('',(#3502),#1438,.F.);
#39191=ADVANCED_FACE('',(#3503),#1439,.F.);
#39192=ADVANCED_FACE('',(#3504),#1440,.F.);
#39193=ADVANCED_FACE('',(#3505),#1441,.F.);
#39194=ADVANCED_FACE('',(#3506),#1442,.F.);
#39195=ADVANCED_FACE('',(#3507),#1443,.F.);
#39196=ADVANCED_FACE('',(#3508),#1444,.F.);
#39197=ADVANCED_FACE('',(#3509),#1445,.F.);
#39198=ADVANCED_FACE('',(#3510),#1446,.F.);
#39199=ADVANCED_FACE('',(#3511),#1447,.F.);
#39200=ADVANCED_FACE('',(#3512),#1448,.F.);
#39201=ADVANCED_FACE('',(#3513),#1449,.F.);
#39202=ADVANCED_FACE('',(#3514),#1450,.F.);
#39203=ADVANCED_FACE('',(#3515),#1451,.F.);
#39204=ADVANCED_FACE('',(#3516),#1452,.F.);
#39205=ADVANCED_FACE('',(#3517),#1453,.F.);
#39206=ADVANCED_FACE('',(#3518),#1454,.F.);
#39207=ADVANCED_FACE('',(#3519),#1455,.F.);
#39208=ADVANCED_FACE('',(#3520),#1456,.F.);
#39209=ADVANCED_FACE('',(#3521),#1457,.F.);
#39210=ADVANCED_FACE('',(#3522),#1458,.F.);
#39211=ADVANCED_FACE('',(#3523),#1459,.F.);
#39212=ADVANCED_FACE('',(#3524),#1460,.F.);
#39213=ADVANCED_FACE('',(#3525),#1461,.F.);
#39214=ADVANCED_FACE('',(#3526),#1462,.F.);
#39215=ADVANCED_FACE('',(#3527),#1463,.F.);
#39216=ADVANCED_FACE('',(#3528),#1464,.F.);
#39217=ADVANCED_FACE('',(#3529),#1465,.F.);
#39218=ADVANCED_FACE('',(#3530),#1466,.F.);
#39219=ADVANCED_FACE('',(#3531),#1467,.F.);
#39220=ADVANCED_FACE('',(#3532),#1468,.F.);
#39221=ADVANCED_FACE('',(#3533),#1469,.F.);
#39222=ADVANCED_FACE('',(#3534),#1470,.F.);
#39223=ADVANCED_FACE('',(#3535),#1471,.F.);
#39224=ADVANCED_FACE('',(#3536),#1472,.F.);
#39225=ADVANCED_FACE('',(#3537),#1473,.F.);
#39226=ADVANCED_FACE('',(#3538),#1474,.F.);
#39227=ADVANCED_FACE('',(#3539),#1475,.F.);
#39228=ADVANCED_FACE('',(#3540),#1476,.F.);
#39229=ADVANCED_FACE('',(#3541),#1477,.F.);
#39230=ADVANCED_FACE('',(#3542),#1478,.F.);
#39231=ADVANCED_FACE('',(#3543),#1479,.F.);
#39232=ADVANCED_FACE('',(#3544),#1480,.F.);
#39233=ADVANCED_FACE('',(#3545),#1481,.F.);
#39234=ADVANCED_FACE('',(#3546),#1482,.F.);
#39235=ADVANCED_FACE('',(#3547),#1483,.F.);
#39236=ADVANCED_FACE('',(#3548),#1484,.F.);
#39237=ADVANCED_FACE('',(#3549),#1485,.F.);
#39238=ADVANCED_FACE('',(#3550),#1486,.F.);
#39239=ADVANCED_FACE('',(#3551),#1487,.F.);
#39240=ADVANCED_FACE('',(#3552),#1488,.F.);
#39241=ADVANCED_FACE('',(#3553),#1489,.F.);
#39242=ADVANCED_FACE('',(#3554),#1490,.F.);
#39243=ADVANCED_FACE('',(#3555),#1491,.F.);
#39244=ADVANCED_FACE('',(#3556),#1492,.F.);
#39245=ADVANCED_FACE('',(#3557),#1493,.F.);
#39246=ADVANCED_FACE('',(#3558),#1494,.F.);
#39247=ADVANCED_FACE('',(#3559),#1495,.F.);
#39248=ADVANCED_FACE('',(#3560),#1496,.F.);
#39249=ADVANCED_FACE('',(#3561),#1497,.F.);
#39250=ADVANCED_FACE('',(#3562),#1498,.F.);
#39251=ADVANCED_FACE('',(#3563),#1499,.F.);
#39252=ADVANCED_FACE('',(#3564),#1500,.F.);
#39253=ADVANCED_FACE('',(#3565),#1501,.F.);
#39254=ADVANCED_FACE('',(#3566),#1502,.F.);
#39255=ADVANCED_FACE('',(#3567),#1503,.F.);
#39256=ADVANCED_FACE('',(#3568),#1504,.F.);
#39257=ADVANCED_FACE('',(#3569),#1505,.F.);
#39258=ADVANCED_FACE('',(#3570),#1506,.F.);
#39259=ADVANCED_FACE('',(#3571),#1507,.F.);
#39260=ADVANCED_FACE('',(#3572),#1508,.F.);
#39261=ADVANCED_FACE('',(#3573),#1509,.F.);
#39262=ADVANCED_FACE('',(#3574),#1510,.F.);
#39263=ADVANCED_FACE('',(#3575),#1511,.F.);
#39264=ADVANCED_FACE('',(#3576),#1512,.F.);
#39265=ADVANCED_FACE('',(#3577),#1513,.F.);
#39266=ADVANCED_FACE('',(#3578),#1514,.F.);
#39267=ADVANCED_FACE('',(#3579),#1515,.F.);
#39268=ADVANCED_FACE('',(#3580),#1516,.F.);
#39269=ADVANCED_FACE('',(#3581),#1517,.F.);
#39270=ADVANCED_FACE('',(#3582),#1518,.F.);
#39271=ADVANCED_FACE('',(#3583),#1519,.F.);
#39272=ADVANCED_FACE('',(#3584),#1520,.F.);
#39273=ADVANCED_FACE('',(#3585),#1521,.F.);
#39274=ADVANCED_FACE('',(#3586),#1522,.F.);
#39275=ADVANCED_FACE('',(#3587),#1523,.F.);
#39276=ADVANCED_FACE('',(#3588),#1524,.F.);
#39277=ADVANCED_FACE('',(#3589),#1525,.F.);
#39278=ADVANCED_FACE('',(#3590),#1526,.F.);
#39279=ADVANCED_FACE('',(#3591),#1527,.F.);
#39280=ADVANCED_FACE('',(#3592),#1528,.F.);
#39281=ADVANCED_FACE('',(#3593),#1529,.F.);
#39282=ADVANCED_FACE('',(#3594),#1530,.F.);
#39283=ADVANCED_FACE('',(#3595),#1531,.F.);
#39284=ADVANCED_FACE('',(#3596),#1532,.F.);
#39285=ADVANCED_FACE('',(#3597),#1533,.F.);
#39286=ADVANCED_FACE('',(#3598),#1534,.F.);
#39287=ADVANCED_FACE('',(#3599),#1535,.F.);
#39288=ADVANCED_FACE('',(#3600),#1536,.F.);
#39289=ADVANCED_FACE('',(#3601),#1537,.F.);
#39290=ADVANCED_FACE('',(#3602),#1538,.F.);
#39291=ADVANCED_FACE('',(#3603),#1539,.F.);
#39292=ADVANCED_FACE('',(#3604),#1540,.F.);
#39293=ADVANCED_FACE('',(#3605),#1541,.F.);
#39294=ADVANCED_FACE('',(#3606),#1542,.F.);
#39295=ADVANCED_FACE('',(#3607),#1543,.F.);
#39296=ADVANCED_FACE('',(#3608),#1544,.F.);
#39297=ADVANCED_FACE('',(#3609),#1545,.F.);
#39298=ADVANCED_FACE('',(#3610),#1546,.F.);
#39299=ADVANCED_FACE('',(#3611),#1547,.F.);
#39300=ADVANCED_FACE('',(#3612),#1548,.F.);
#39301=ADVANCED_FACE('',(#3613),#1549,.F.);
#39302=ADVANCED_FACE('',(#3614),#1550,.F.);
#39303=ADVANCED_FACE('',(#3615),#1551,.F.);
#39304=ADVANCED_FACE('',(#3616),#1552,.F.);
#39305=ADVANCED_FACE('',(#3617),#1553,.F.);
#39306=ADVANCED_FACE('',(#3618),#1554,.F.);
#39307=ADVANCED_FACE('',(#3619),#1555,.F.);
#39308=ADVANCED_FACE('',(#3620),#1556,.F.);
#39309=ADVANCED_FACE('',(#3621),#1557,.F.);
#39310=ADVANCED_FACE('',(#3622),#1558,.F.);
#39311=ADVANCED_FACE('',(#3623),#1559,.F.);
#39312=ADVANCED_FACE('',(#3624),#1560,.F.);
#39313=ADVANCED_FACE('',(#3625),#1561,.F.);
#39314=ADVANCED_FACE('',(#3626),#1562,.F.);
#39315=ADVANCED_FACE('',(#3627),#1563,.F.);
#39316=ADVANCED_FACE('',(#3628),#1564,.F.);
#39317=ADVANCED_FACE('',(#3629),#1565,.F.);
#39318=ADVANCED_FACE('',(#3630),#1566,.F.);
#39319=ADVANCED_FACE('',(#3631),#1567,.F.);
#39320=ADVANCED_FACE('',(#3632),#1568,.F.);
#39321=ADVANCED_FACE('',(#3633),#1569,.F.);
#39322=ADVANCED_FACE('',(#3634),#1570,.F.);
#39323=ADVANCED_FACE('',(#3635),#1571,.F.);
#39324=ADVANCED_FACE('',(#3636),#1572,.F.);
#39325=ADVANCED_FACE('',(#3637),#1573,.F.);
#39326=ADVANCED_FACE('',(#3638),#1574,.F.);
#39327=ADVANCED_FACE('',(#3639),#1575,.F.);
#39328=ADVANCED_FACE('',(#3640),#1576,.F.);
#39329=ADVANCED_FACE('',(#3641),#1577,.F.);
#39330=ADVANCED_FACE('',(#3642),#1578,.F.);
#39331=ADVANCED_FACE('',(#3643),#1579,.F.);
#39332=ADVANCED_FACE('',(#3644),#1580,.F.);
#39333=ADVANCED_FACE('',(#3645),#1581,.F.);
#39334=ADVANCED_FACE('',(#3646),#1582,.F.);
#39335=ADVANCED_FACE('',(#3647),#1583,.F.);
#39336=ADVANCED_FACE('',(#3648),#1584,.F.);
#39337=ADVANCED_FACE('',(#3649),#1585,.F.);
#39338=ADVANCED_FACE('',(#3650),#1586,.F.);
#39339=ADVANCED_FACE('',(#3651),#1587,.F.);
#39340=ADVANCED_FACE('',(#3652),#1588,.F.);
#39341=ADVANCED_FACE('',(#3653),#1589,.F.);
#39342=ADVANCED_FACE('',(#3654),#1590,.F.);
#39343=ADVANCED_FACE('',(#3655),#1591,.F.);
#39344=ADVANCED_FACE('',(#3656),#1592,.F.);
#39345=ADVANCED_FACE('',(#3657),#1593,.F.);
#39346=ADVANCED_FACE('',(#3658),#1594,.F.);
#39347=ADVANCED_FACE('',(#3659),#1595,.F.);
#39348=ADVANCED_FACE('',(#3660),#1596,.F.);
#39349=ADVANCED_FACE('',(#3661),#1597,.F.);
#39350=ADVANCED_FACE('',(#3662),#1598,.F.);
#39351=ADVANCED_FACE('',(#3663),#1599,.F.);
#39352=ADVANCED_FACE('',(#3664),#1600,.F.);
#39353=ADVANCED_FACE('',(#3665),#1601,.F.);
#39354=ADVANCED_FACE('',(#3666),#1602,.F.);
#39355=ADVANCED_FACE('',(#3667),#1603,.F.);
#39356=ADVANCED_FACE('',(#3668),#1604,.F.);
#39357=ADVANCED_FACE('',(#3669),#1605,.F.);
#39358=ADVANCED_FACE('',(#3670),#1606,.F.);
#39359=ADVANCED_FACE('',(#3671),#1607,.F.);
#39360=ADVANCED_FACE('',(#3672),#1608,.F.);
#39361=ADVANCED_FACE('',(#3673),#1609,.F.);
#39362=ADVANCED_FACE('',(#3674),#1610,.F.);
#39363=ADVANCED_FACE('',(#3675),#1611,.F.);
#39364=ADVANCED_FACE('',(#3676),#1612,.F.);
#39365=ADVANCED_FACE('',(#3677),#1613,.F.);
#39366=ADVANCED_FACE('',(#3678),#1614,.F.);
#39367=ADVANCED_FACE('',(#3679),#1615,.F.);
#39368=ADVANCED_FACE('',(#3680),#1616,.F.);
#39369=ADVANCED_FACE('',(#3681),#1617,.F.);
#39370=ADVANCED_FACE('',(#3682),#1618,.F.);
#39371=ADVANCED_FACE('',(#3683),#1619,.F.);
#39372=ADVANCED_FACE('',(#3684),#1620,.F.);
#39373=ADVANCED_FACE('',(#3685),#1621,.F.);
#39374=ADVANCED_FACE('',(#3686),#1622,.F.);
#39375=ADVANCED_FACE('',(#3687),#1623,.F.);
#39376=ADVANCED_FACE('',(#3688),#1624,.F.);
#39377=ADVANCED_FACE('',(#3689),#1625,.F.);
#39378=ADVANCED_FACE('',(#3690),#1626,.F.);
#39379=ADVANCED_FACE('',(#3691),#1627,.F.);
#39380=ADVANCED_FACE('',(#3692),#1628,.F.);
#39381=ADVANCED_FACE('',(#3693),#1629,.F.);
#39382=ADVANCED_FACE('',(#3694),#1630,.F.);
#39383=ADVANCED_FACE('',(#3695),#1631,.F.);
#39384=ADVANCED_FACE('',(#3696),#1632,.F.);
#39385=ADVANCED_FACE('',(#3697),#1633,.F.);
#39386=ADVANCED_FACE('',(#3698),#1634,.F.);
#39387=ADVANCED_FACE('',(#3699),#1635,.F.);
#39388=ADVANCED_FACE('',(#3700),#1636,.F.);
#39389=ADVANCED_FACE('',(#3701),#1637,.F.);
#39390=ADVANCED_FACE('',(#3702),#1638,.F.);
#39391=ADVANCED_FACE('',(#3703),#1639,.F.);
#39392=ADVANCED_FACE('',(#3704),#1640,.F.);
#39393=ADVANCED_FACE('',(#3705),#1641,.F.);
#39394=ADVANCED_FACE('',(#3706),#1642,.F.);
#39395=ADVANCED_FACE('',(#3707),#1643,.F.);
#39396=ADVANCED_FACE('',(#3708),#1644,.F.);
#39397=ADVANCED_FACE('',(#3709),#1645,.F.);
#39398=ADVANCED_FACE('',(#3710),#1646,.F.);
#39399=ADVANCED_FACE('',(#3711),#1647,.F.);
#39400=ADVANCED_FACE('',(#3712),#1648,.F.);
#39401=ADVANCED_FACE('',(#3713),#1649,.F.);
#39402=ADVANCED_FACE('',(#3714),#1650,.F.);
#39403=ADVANCED_FACE('',(#3715),#1651,.F.);
#39404=ADVANCED_FACE('',(#3716),#1652,.F.);
#39405=ADVANCED_FACE('',(#3717),#1653,.F.);
#39406=ADVANCED_FACE('',(#3718),#1654,.F.);
#39407=ADVANCED_FACE('',(#3719),#1655,.F.);
#39408=ADVANCED_FACE('',(#3720),#1656,.F.);
#39409=ADVANCED_FACE('',(#3721),#1657,.F.);
#39410=ADVANCED_FACE('',(#3722),#1658,.F.);
#39411=ADVANCED_FACE('',(#3723),#1659,.F.);
#39412=ADVANCED_FACE('',(#3724),#1660,.F.);
#39413=ADVANCED_FACE('',(#3725),#1661,.F.);
#39414=ADVANCED_FACE('',(#3726),#1662,.F.);
#39415=ADVANCED_FACE('',(#3727),#1663,.F.);
#39416=ADVANCED_FACE('',(#3728),#1664,.F.);
#39417=ADVANCED_FACE('',(#3729),#1665,.F.);
#39418=ADVANCED_FACE('',(#3730),#1666,.F.);
#39419=ADVANCED_FACE('',(#3731),#1667,.F.);
#39420=ADVANCED_FACE('',(#3732),#1668,.F.);
#39421=ADVANCED_FACE('',(#3733),#1669,.F.);
#39422=ADVANCED_FACE('',(#3734),#1670,.F.);
#39423=ADVANCED_FACE('',(#3735),#1671,.F.);
#39424=ADVANCED_FACE('',(#3736),#1672,.F.);
#39425=ADVANCED_FACE('',(#3737),#1673,.F.);
#39426=ADVANCED_FACE('',(#3738),#1674,.F.);
#39427=ADVANCED_FACE('',(#3739),#1675,.F.);
#39428=ADVANCED_FACE('',(#3740),#1676,.F.);
#39429=ADVANCED_FACE('',(#3741),#1677,.F.);
#39430=ADVANCED_FACE('',(#3742),#1678,.F.);
#39431=ADVANCED_FACE('',(#3743),#1679,.F.);
#39432=ADVANCED_FACE('',(#3744),#1680,.F.);
#39433=ADVANCED_FACE('',(#3745),#1681,.F.);
#39434=ADVANCED_FACE('',(#3746),#1682,.F.);
#39435=ADVANCED_FACE('',(#3747),#1683,.F.);
#39436=ADVANCED_FACE('',(#3748),#1684,.F.);
#39437=ADVANCED_FACE('',(#3749),#1685,.F.);
#39438=ADVANCED_FACE('',(#3750),#1686,.F.);
#39439=ADVANCED_FACE('',(#3751),#1687,.F.);
#39440=ADVANCED_FACE('',(#3752),#1688,.F.);
#39441=ADVANCED_FACE('',(#3753),#1689,.F.);
#39442=ADVANCED_FACE('',(#3754),#1690,.F.);
#39443=ADVANCED_FACE('',(#3755),#1691,.F.);
#39444=ADVANCED_FACE('',(#3756),#1692,.F.);
#39445=ADVANCED_FACE('',(#3757),#1693,.F.);
#39446=ADVANCED_FACE('',(#3758),#1694,.F.);
#39447=ADVANCED_FACE('',(#3759),#1695,.F.);
#39448=ADVANCED_FACE('',(#3760),#1696,.F.);
#39449=ADVANCED_FACE('',(#3761),#1697,.F.);
#39450=ADVANCED_FACE('',(#3762),#1698,.F.);
#39451=ADVANCED_FACE('',(#3763),#1699,.F.);
#39452=ADVANCED_FACE('',(#3764),#1700,.F.);
#39453=ADVANCED_FACE('',(#3765),#1701,.F.);
#39454=ADVANCED_FACE('',(#3766),#1702,.F.);
#39455=ADVANCED_FACE('',(#3767),#1703,.F.);
#39456=ADVANCED_FACE('',(#3768),#1704,.F.);
#39457=ADVANCED_FACE('',(#3769),#1705,.F.);
#39458=ADVANCED_FACE('',(#3770),#1706,.F.);
#39459=ADVANCED_FACE('',(#3771),#1707,.F.);
#39460=ADVANCED_FACE('',(#3772),#1708,.F.);
#39461=ADVANCED_FACE('',(#3773),#1709,.F.);
#39462=ADVANCED_FACE('',(#3774),#1710,.F.);
#39463=ADVANCED_FACE('',(#3775),#1711,.F.);
#39464=ADVANCED_FACE('',(#3776),#1712,.F.);
#39465=ADVANCED_FACE('',(#3777),#1713,.F.);
#39466=ADVANCED_FACE('',(#3778),#1714,.F.);
#39467=ADVANCED_FACE('',(#3779),#1715,.F.);
#39468=ADVANCED_FACE('',(#3780),#1716,.F.);
#39469=ADVANCED_FACE('',(#3781),#1717,.F.);
#39470=ADVANCED_FACE('',(#3782),#1718,.F.);
#39471=ADVANCED_FACE('',(#3783),#1719,.F.);
#39472=ADVANCED_FACE('',(#3784),#1720,.F.);
#39473=ADVANCED_FACE('',(#3785),#1721,.F.);
#39474=ADVANCED_FACE('',(#3786),#1722,.F.);
#39475=ADVANCED_FACE('',(#3787),#1723,.F.);
#39476=ADVANCED_FACE('',(#3788),#1724,.F.);
#39477=ADVANCED_FACE('',(#3789),#1725,.F.);
#39478=ADVANCED_FACE('',(#3790),#1726,.F.);
#39479=ADVANCED_FACE('',(#3791),#1727,.F.);
#39480=ADVANCED_FACE('',(#3792),#1728,.F.);
#39481=ADVANCED_FACE('',(#3793),#1729,.F.);
#39482=ADVANCED_FACE('',(#3794),#1730,.F.);
#39483=ADVANCED_FACE('',(#3795),#1731,.F.);
#39484=ADVANCED_FACE('',(#3796),#1732,.F.);
#39485=ADVANCED_FACE('',(#3797),#1733,.F.);
#39486=ADVANCED_FACE('',(#3798),#1734,.F.);
#39487=ADVANCED_FACE('',(#3799),#1735,.F.);
#39488=ADVANCED_FACE('',(#3800),#1736,.F.);
#39489=ADVANCED_FACE('',(#3801),#1737,.F.);
#39490=ADVANCED_FACE('',(#3802),#1738,.F.);
#39491=ADVANCED_FACE('',(#3803),#1739,.F.);
#39492=ADVANCED_FACE('',(#3804),#1740,.F.);
#39493=ADVANCED_FACE('',(#3805),#1741,.F.);
#39494=ADVANCED_FACE('',(#3806),#1742,.F.);
#39495=ADVANCED_FACE('',(#3807),#1743,.F.);
#39496=ADVANCED_FACE('',(#3808),#1744,.F.);
#39497=ADVANCED_FACE('',(#3809),#1745,.F.);
#39498=ADVANCED_FACE('',(#3810),#1746,.F.);
#39499=ADVANCED_FACE('',(#3811),#1747,.F.);
#39500=ADVANCED_FACE('',(#3812),#1748,.F.);
#39501=ADVANCED_FACE('',(#3813),#1749,.F.);
#39502=ADVANCED_FACE('',(#3814),#1750,.F.);
#39503=ADVANCED_FACE('',(#3815),#1751,.F.);
#39504=ADVANCED_FACE('',(#3816),#1752,.F.);
#39505=ADVANCED_FACE('',(#3817),#1753,.F.);
#39506=ADVANCED_FACE('',(#3818),#1754,.F.);
#39507=ADVANCED_FACE('',(#3819),#1755,.F.);
#39508=ADVANCED_FACE('',(#3820),#1756,.F.);
#39509=ADVANCED_FACE('',(#3821),#1757,.F.);
#39510=ADVANCED_FACE('',(#3822),#1758,.F.);
#39511=ADVANCED_FACE('',(#3823),#1759,.F.);
#39512=ADVANCED_FACE('',(#3824),#1760,.F.);
#39513=ADVANCED_FACE('',(#3825),#1761,.F.);
#39514=ADVANCED_FACE('',(#3826),#1762,.F.);
#39515=ADVANCED_FACE('',(#3827),#1763,.F.);
#39516=ADVANCED_FACE('',(#3828),#1764,.F.);
#39517=ADVANCED_FACE('',(#3829),#1765,.F.);
#39518=ADVANCED_FACE('',(#3830),#1766,.F.);
#39519=ADVANCED_FACE('',(#3831),#1767,.F.);
#39520=ADVANCED_FACE('',(#3832),#1768,.F.);
#39521=ADVANCED_FACE('',(#3833),#1769,.F.);
#39522=ADVANCED_FACE('',(#3834),#1770,.F.);
#39523=ADVANCED_FACE('',(#3835),#1771,.F.);
#39524=ADVANCED_FACE('',(#3836),#1772,.F.);
#39525=ADVANCED_FACE('',(#3837),#1773,.F.);
#39526=ADVANCED_FACE('',(#3838),#1774,.F.);
#39527=ADVANCED_FACE('',(#3839),#1775,.F.);
#39528=ADVANCED_FACE('',(#3840),#1776,.F.);
#39529=ADVANCED_FACE('',(#3841),#1777,.F.);
#39530=ADVANCED_FACE('',(#3842),#1778,.F.);
#39531=ADVANCED_FACE('',(#3843),#1779,.F.);
#39532=ADVANCED_FACE('',(#3844),#1780,.F.);
#39533=ADVANCED_FACE('',(#3845),#1781,.F.);
#39534=ADVANCED_FACE('',(#3846),#1782,.F.);
#39535=ADVANCED_FACE('',(#3847),#1783,.F.);
#39536=ADVANCED_FACE('',(#3848),#1784,.F.);
#39537=ADVANCED_FACE('',(#3849),#1785,.F.);
#39538=ADVANCED_FACE('',(#3850),#1786,.F.);
#39539=ADVANCED_FACE('',(#3851),#1787,.F.);
#39540=ADVANCED_FACE('',(#3852),#1788,.F.);
#39541=ADVANCED_FACE('',(#3853),#1789,.F.);
#39542=ADVANCED_FACE('',(#3854),#1790,.F.);
#39543=ADVANCED_FACE('',(#3855),#1791,.F.);
#39544=ADVANCED_FACE('',(#3856),#1792,.F.);
#39545=ADVANCED_FACE('',(#3857),#1793,.F.);
#39546=ADVANCED_FACE('',(#3858),#1794,.F.);
#39547=ADVANCED_FACE('',(#3859),#1795,.F.);
#39548=ADVANCED_FACE('',(#3860),#1796,.F.);
#39549=ADVANCED_FACE('',(#3861),#1797,.F.);
#39550=ADVANCED_FACE('',(#3862),#1798,.F.);
#39551=ADVANCED_FACE('',(#3863),#1799,.F.);
#39552=ADVANCED_FACE('',(#3864),#1800,.F.);
#39553=ADVANCED_FACE('',(#3865),#1801,.F.);
#39554=ADVANCED_FACE('',(#3866),#1802,.F.);
#39555=ADVANCED_FACE('',(#3867),#1803,.F.);
#39556=ADVANCED_FACE('',(#3868),#1804,.F.);
#39557=ADVANCED_FACE('',(#3869),#1805,.F.);
#39558=ADVANCED_FACE('',(#3870),#1806,.F.);
#39559=ADVANCED_FACE('',(#3871),#1807,.F.);
#39560=ADVANCED_FACE('',(#3872),#1808,.F.);
#39561=ADVANCED_FACE('',(#3873),#1809,.F.);
#39562=ADVANCED_FACE('',(#3874),#1810,.F.);
#39563=ADVANCED_FACE('',(#3875),#1811,.F.);
#39564=ADVANCED_FACE('',(#3876),#1812,.F.);
#39565=ADVANCED_FACE('',(#3877),#1813,.F.);
#39566=ADVANCED_FACE('',(#3878),#1814,.F.);
#39567=ADVANCED_FACE('',(#3879),#1815,.F.);
#39568=ADVANCED_FACE('',(#3880),#1816,.F.);
#39569=ADVANCED_FACE('',(#3881),#1817,.F.);
#39570=ADVANCED_FACE('',(#3882),#1818,.F.);
#39571=ADVANCED_FACE('',(#3883),#1819,.F.);
#39572=ADVANCED_FACE('',(#3884),#1820,.F.);
#39573=ADVANCED_FACE('',(#3885),#1821,.F.);
#39574=ADVANCED_FACE('',(#3886),#1822,.F.);
#39575=ADVANCED_FACE('',(#3887),#1823,.F.);
#39576=ADVANCED_FACE('',(#3888),#1824,.F.);
#39577=ADVANCED_FACE('',(#3889),#1825,.F.);
#39578=ADVANCED_FACE('',(#3890),#1826,.F.);
#39579=ADVANCED_FACE('',(#3891),#1827,.F.);
#39580=ADVANCED_FACE('',(#3892),#1828,.F.);
#39581=ADVANCED_FACE('',(#3893),#1829,.F.);
#39582=ADVANCED_FACE('',(#3894),#1830,.F.);
#39583=ADVANCED_FACE('',(#3895),#1831,.F.);
#39584=ADVANCED_FACE('',(#3896),#1832,.F.);
#39585=ADVANCED_FACE('',(#3897),#1833,.F.);
#39586=ADVANCED_FACE('',(#3898),#1834,.F.);
#39587=ADVANCED_FACE('',(#3899),#1835,.F.);
#39588=ADVANCED_FACE('',(#3900),#1836,.F.);
#39589=ADVANCED_FACE('',(#3901),#1837,.F.);
#39590=ADVANCED_FACE('',(#3902),#1838,.F.);
#39591=ADVANCED_FACE('',(#3903),#1839,.F.);
#39592=ADVANCED_FACE('',(#3904),#1840,.F.);
#39593=ADVANCED_FACE('',(#3905),#1841,.F.);
#39594=ADVANCED_FACE('',(#3906),#1842,.F.);
#39595=ADVANCED_FACE('',(#3907),#1843,.F.);
#39596=ADVANCED_FACE('',(#3908),#1844,.F.);
#39597=ADVANCED_FACE('',(#3909),#1845,.F.);
#39598=ADVANCED_FACE('',(#3910),#1846,.F.);
#39599=ADVANCED_FACE('',(#3911),#1847,.F.);
#39600=ADVANCED_FACE('',(#3912),#1848,.F.);
#39601=ADVANCED_FACE('',(#3913),#1849,.F.);
#39602=ADVANCED_FACE('',(#3914),#1850,.F.);
#39603=ADVANCED_FACE('',(#3915),#1851,.F.);
#39604=ADVANCED_FACE('',(#3916),#1852,.F.);
#39605=ADVANCED_FACE('',(#3917),#1853,.F.);
#39606=ADVANCED_FACE('',(#3918),#1854,.F.);
#39607=ADVANCED_FACE('',(#3919),#1855,.F.);
#39608=ADVANCED_FACE('',(#3920),#1856,.F.);
#39609=ADVANCED_FACE('',(#3921),#1857,.F.);
#39610=ADVANCED_FACE('',(#3922),#1858,.F.);
#39611=ADVANCED_FACE('',(#3923),#1859,.F.);
#39612=ADVANCED_FACE('',(#3924),#1860,.F.);
#39613=ADVANCED_FACE('',(#3925),#1861,.F.);
#39614=ADVANCED_FACE('',(#3926),#1862,.F.);
#39615=ADVANCED_FACE('',(#3927),#1863,.F.);
#39616=ADVANCED_FACE('',(#3928),#1864,.F.);
#39617=ADVANCED_FACE('',(#3929),#1865,.F.);
#39618=ADVANCED_FACE('',(#3930),#1866,.F.);
#39619=ADVANCED_FACE('',(#3931),#1867,.F.);
#39620=ADVANCED_FACE('',(#3932),#1868,.F.);
#39621=ADVANCED_FACE('',(#3933),#1869,.F.);
#39622=ADVANCED_FACE('',(#3934),#1870,.F.);
#39623=ADVANCED_FACE('',(#3935),#1871,.F.);
#39624=ADVANCED_FACE('',(#3936),#1872,.F.);
#39625=ADVANCED_FACE('',(#3937),#1873,.F.);
#39626=ADVANCED_FACE('',(#3938),#1874,.F.);
#39627=ADVANCED_FACE('',(#3939),#1875,.F.);
#39628=ADVANCED_FACE('',(#3940),#1876,.F.);
#39629=ADVANCED_FACE('',(#3941),#1877,.F.);
#39630=ADVANCED_FACE('',(#3942),#1878,.F.);
#39631=ADVANCED_FACE('',(#3943),#1879,.F.);
#39632=ADVANCED_FACE('',(#3944),#1880,.F.);
#39633=ADVANCED_FACE('',(#3945),#1881,.F.);
#39634=ADVANCED_FACE('',(#3946),#1882,.F.);
#39635=ADVANCED_FACE('',(#3947),#1883,.F.);
#39636=ADVANCED_FACE('',(#3948),#1884,.F.);
#39637=ADVANCED_FACE('',(#3949),#1885,.F.);
#39638=ADVANCED_FACE('',(#3950),#1886,.F.);
#39639=ADVANCED_FACE('',(#3951),#1887,.F.);
#39640=ADVANCED_FACE('',(#3952),#1888,.F.);
#39641=ADVANCED_FACE('',(#3953),#1889,.F.);
#39642=ADVANCED_FACE('',(#3954),#1890,.F.);
#39643=ADVANCED_FACE('',(#3955),#1891,.F.);
#39644=ADVANCED_FACE('',(#3956),#1892,.F.);
#39645=ADVANCED_FACE('',(#3957),#1893,.F.);
#39646=ADVANCED_FACE('',(#3958),#1894,.F.);
#39647=ADVANCED_FACE('',(#3959),#1895,.F.);
#39648=ADVANCED_FACE('',(#3960),#1896,.F.);
#39649=ADVANCED_FACE('',(#3961),#1897,.F.);
#39650=ADVANCED_FACE('',(#3962),#1898,.F.);
#39651=ADVANCED_FACE('',(#3963),#1899,.F.);
#39652=ADVANCED_FACE('',(#3964),#1900,.F.);
#39653=ADVANCED_FACE('',(#3965),#1901,.F.);
#39654=ADVANCED_FACE('',(#3966),#1902,.F.);
#39655=ADVANCED_FACE('',(#3967),#1903,.F.);
#39656=ADVANCED_FACE('',(#3968),#1904,.F.);
#39657=ADVANCED_FACE('',(#3969),#1905,.F.);
#39658=ADVANCED_FACE('',(#3970),#1906,.F.);
#39659=ADVANCED_FACE('',(#3971),#1907,.F.);
#39660=ADVANCED_FACE('',(#3972),#1908,.F.);
#39661=ADVANCED_FACE('',(#3973),#1909,.F.);
#39662=ADVANCED_FACE('',(#3974),#1910,.F.);
#39663=ADVANCED_FACE('',(#3975),#1911,.F.);
#39664=ADVANCED_FACE('',(#3976),#1912,.F.);
#39665=ADVANCED_FACE('',(#3977),#1913,.F.);
#39666=ADVANCED_FACE('',(#3978),#1914,.F.);
#39667=ADVANCED_FACE('',(#3979),#1915,.F.);
#39668=ADVANCED_FACE('',(#3980),#1916,.F.);
#39669=ADVANCED_FACE('',(#3981),#1917,.F.);
#39670=ADVANCED_FACE('',(#3982),#1918,.F.);
#39671=ADVANCED_FACE('',(#3983),#1919,.F.);
#39672=ADVANCED_FACE('',(#3984),#1920,.F.);
#39673=ADVANCED_FACE('',(#3985),#1921,.F.);
#39674=ADVANCED_FACE('',(#3986),#1922,.F.);
#39675=ADVANCED_FACE('',(#3987),#1923,.F.);
#39676=ADVANCED_FACE('',(#3988),#1924,.F.);
#39677=ADVANCED_FACE('',(#3989),#1925,.F.);
#39678=ADVANCED_FACE('',(#3990),#1926,.F.);
#39679=ADVANCED_FACE('',(#3991),#1927,.F.);
#39680=ADVANCED_FACE('',(#3992),#1928,.F.);
#39681=ADVANCED_FACE('',(#3993),#1929,.F.);
#39682=ADVANCED_FACE('',(#3994),#1930,.F.);
#39683=ADVANCED_FACE('',(#3995),#1931,.F.);
#39684=ADVANCED_FACE('',(#3996),#1932,.F.);
#39685=ADVANCED_FACE('',(#3997),#1933,.F.);
#39686=ADVANCED_FACE('',(#3998),#1934,.F.);
#39687=ADVANCED_FACE('',(#3999),#1935,.F.);
#39688=ADVANCED_FACE('',(#4000),#1936,.F.);
#39689=ADVANCED_FACE('',(#4001),#1937,.F.);
#39690=ADVANCED_FACE('',(#4002),#1938,.F.);
#39691=ADVANCED_FACE('',(#4003),#1939,.F.);
#39692=ADVANCED_FACE('',(#4004),#1940,.F.);
#39693=ADVANCED_FACE('',(#4005),#1941,.F.);
#39694=ADVANCED_FACE('',(#4006),#1942,.F.);
#39695=ADVANCED_FACE('',(#4007),#1943,.F.);
#39696=ADVANCED_FACE('',(#4008),#1944,.F.);
#39697=ADVANCED_FACE('',(#4009),#1945,.F.);
#39698=ADVANCED_FACE('',(#4010),#1946,.F.);
#39699=ADVANCED_FACE('',(#4011),#1947,.F.);
#39700=ADVANCED_FACE('',(#4012),#1948,.F.);
#39701=ADVANCED_FACE('',(#4013),#1949,.F.);
#39702=ADVANCED_FACE('',(#4014),#1950,.F.);
#39703=ADVANCED_FACE('',(#4015),#1951,.F.);
#39704=ADVANCED_FACE('',(#4016),#1952,.F.);
#39705=ADVANCED_FACE('',(#4017),#1953,.F.);
#39706=ADVANCED_FACE('',(#4018),#1954,.F.);
#39707=ADVANCED_FACE('',(#4019),#1955,.F.);
#39708=ADVANCED_FACE('',(#4020),#1956,.F.);
#39709=ADVANCED_FACE('',(#4021),#1957,.F.);
#39710=ADVANCED_FACE('',(#4022),#1958,.F.);
#39711=ADVANCED_FACE('',(#4023),#1959,.F.);
#39712=ADVANCED_FACE('',(#4024),#1960,.F.);
#39713=ADVANCED_FACE('',(#4025),#1961,.F.);
#39714=ADVANCED_FACE('',(#4026),#1962,.F.);
#39715=ADVANCED_FACE('',(#4027),#1963,.F.);
#39716=ADVANCED_FACE('',(#4028),#1964,.F.);
#39717=ADVANCED_FACE('',(#4029),#1965,.F.);
#39718=ADVANCED_FACE('',(#4030),#1966,.F.);
#39719=ADVANCED_FACE('',(#4031),#1967,.F.);
#39720=ADVANCED_FACE('',(#4032),#1968,.F.);
#39721=ADVANCED_FACE('',(#4033),#1969,.F.);
#39722=ADVANCED_FACE('',(#4034),#1970,.F.);
#39723=ADVANCED_FACE('',(#4035),#1971,.F.);
#39724=ADVANCED_FACE('',(#4036),#1972,.F.);
#39725=ADVANCED_FACE('',(#4037),#1973,.F.);
#39726=ADVANCED_FACE('',(#4038),#1974,.F.);
#39727=ADVANCED_FACE('',(#4039),#1975,.F.);
#39728=ADVANCED_FACE('',(#4040),#1976,.F.);
#39729=ADVANCED_FACE('',(#4041),#1977,.F.);
#39730=ADVANCED_FACE('',(#4042),#1978,.F.);
#39731=ADVANCED_FACE('',(#4043),#1979,.F.);
#39732=ADVANCED_FACE('',(#4044),#1980,.F.);
#39733=ADVANCED_FACE('',(#4045),#1981,.F.);
#39734=ADVANCED_FACE('',(#4046),#1982,.F.);
#39735=ADVANCED_FACE('',(#4047),#1983,.F.);
#39736=ADVANCED_FACE('',(#4048),#1984,.F.);
#39737=ADVANCED_FACE('',(#4049),#1985,.F.);
#39738=ADVANCED_FACE('',(#4050),#1986,.F.);
#39739=ADVANCED_FACE('',(#4051),#1987,.F.);
#39740=ADVANCED_FACE('',(#4052),#1988,.F.);
#39741=ADVANCED_FACE('',(#4053),#1989,.F.);
#39742=ADVANCED_FACE('',(#4054),#1990,.F.);
#39743=ADVANCED_FACE('',(#4055),#1991,.F.);
#39744=ADVANCED_FACE('',(#4056),#1992,.F.);
#39745=ADVANCED_FACE('',(#4057),#1993,.F.);
#39746=ADVANCED_FACE('',(#4058),#1994,.F.);
#39747=ADVANCED_FACE('',(#4059),#1995,.F.);
#39748=ADVANCED_FACE('',(#4060),#1996,.F.);
#39749=ADVANCED_FACE('',(#4061),#1997,.F.);
#39750=ADVANCED_FACE('',(#4062),#1998,.F.);
#39751=ADVANCED_FACE('',(#4063),#1999,.F.);
#39752=ADVANCED_FACE('',(#4064),#2000,.F.);
#39753=ADVANCED_FACE('',(#4065),#2001,.F.);
#39754=ADVANCED_FACE('',(#4066),#2002,.F.);
#39755=ADVANCED_FACE('',(#4067),#2003,.F.);
#39756=ADVANCED_FACE('',(#4068),#2004,.F.);
#39757=ADVANCED_FACE('',(#4069),#2005,.F.);
#39758=ADVANCED_FACE('',(#4070),#2006,.F.);
#39759=ADVANCED_FACE('',(#4071),#2007,.F.);
#39760=ADVANCED_FACE('',(#4072),#2008,.F.);
#39761=ADVANCED_FACE('',(#4073),#2009,.F.);
#39762=ADVANCED_FACE('',(#4074),#2010,.F.);
#39763=ADVANCED_FACE('',(#4075),#2011,.F.);
#39764=ADVANCED_FACE('',(#4076),#2012,.F.);
#39765=ADVANCED_FACE('',(#4077),#2013,.F.);
#39766=ADVANCED_FACE('',(#4078),#2014,.F.);
#39767=ADVANCED_FACE('',(#4079),#2015,.F.);
#39768=ADVANCED_FACE('',(#4080),#2016,.F.);
#39769=ADVANCED_FACE('',(#4081),#2017,.F.);
#39770=ADVANCED_FACE('',(#4082),#2018,.F.);
#39771=ADVANCED_FACE('',(#4083),#2019,.F.);
#39772=ADVANCED_FACE('',(#4084),#2020,.F.);
#39773=ADVANCED_FACE('',(#4085),#2021,.F.);
#39774=ADVANCED_FACE('',(#4086),#2022,.F.);
#39775=ADVANCED_FACE('',(#4087),#2023,.F.);
#39776=ADVANCED_FACE('',(#4088),#2024,.F.);
#39777=ADVANCED_FACE('',(#4089),#2025,.F.);
#39778=ADVANCED_FACE('',(#4090),#2026,.F.);
#39779=ADVANCED_FACE('',(#4091),#2027,.F.);
#39780=ADVANCED_FACE('',(#4092),#2028,.F.);
#39781=ADVANCED_FACE('',(#4093),#2029,.F.);
#39782=ADVANCED_FACE('',(#4094),#2030,.F.);
#39783=ADVANCED_FACE('',(#4095),#2031,.F.);
#39784=ADVANCED_FACE('',(#4096),#2032,.F.);
#39785=ADVANCED_FACE('',(#4097),#2033,.F.);
#39786=ADVANCED_FACE('',(#4098),#2034,.F.);
#39787=ADVANCED_FACE('',(#4099),#2035,.F.);
#39788=ADVANCED_FACE('',(#4100),#2036,.F.);
#39789=ADVANCED_FACE('',(#4101),#2037,.F.);
#39790=ADVANCED_FACE('',(#4102),#2038,.F.);
#39791=ADVANCED_FACE('',(#4103),#2039,.F.);
#39792=ADVANCED_FACE('',(#4104),#2040,.F.);
#39793=ADVANCED_FACE('',(#4105),#2041,.F.);
#39794=ADVANCED_FACE('',(#4106),#2042,.F.);
#39795=ADVANCED_FACE('',(#4107),#2043,.F.);
#39796=ADVANCED_FACE('',(#4108),#2044,.F.);
#39797=ADVANCED_FACE('',(#4109),#2045,.F.);
#39798=ADVANCED_FACE('',(#4110),#2046,.F.);
#39799=ADVANCED_FACE('',(#4111),#2047,.F.);
#39800=ADVANCED_FACE('',(#4112),#2048,.F.);
#39801=ADVANCED_FACE('',(#4113),#2049,.F.);
#39802=ADVANCED_FACE('',(#4114),#2050,.F.);
#39803=ADVANCED_FACE('',(#4115),#2051,.F.);
#39804=ADVANCED_FACE('',(#4116),#2052,.F.);
#39805=ADVANCED_FACE('',(#4117),#2053,.F.);
#39806=ADVANCED_FACE('',(#4118),#2054,.F.);
#39807=ADVANCED_FACE('',(#4119),#2055,.F.);
#39808=ADVANCED_FACE('',(#4120),#2056,.F.);
#39809=ADVANCED_FACE('',(#4121),#2057,.F.);
#39810=ADVANCED_FACE('',(#4122),#2058,.F.);
#39811=ADVANCED_FACE('',(#4123),#2059,.F.);
#39812=ADVANCED_FACE('',(#4124),#2060,.F.);
#39813=ADVANCED_FACE('',(#4125),#2061,.F.);
#39814=ADVANCED_FACE('',(#4126),#2062,.F.);
#39815=ADVANCED_FACE('',(#4127),#2063,.F.);
#39816=ADVANCED_FACE('',(#4128),#2064,.F.);
#39817=ADVANCED_FACE('',(#4129),#2065,.F.);
#39818=ADVANCED_FACE('',(#4130),#2066,.F.);
#39819=ADVANCED_FACE('',(#4131),#2067,.F.);
#39820=ADVANCED_FACE('',(#4132),#2068,.F.);
#39821=ADVANCED_FACE('',(#4133),#2069,.F.);
#39822=ADVANCED_FACE('',(#4134),#2070,.F.);
#39823=ADVANCED_FACE('',(#4135),#2071,.F.);
#39824=ADVANCED_FACE('',(#4136),#2072,.F.);
#39825=ADVANCED_FACE('',(#4137),#2073,.F.);
#39826=ADVANCED_FACE('',(#4138),#2074,.F.);
#39827=ADVANCED_FACE('',(#4139),#2075,.F.);
#39828=ADVANCED_FACE('',(#4140),#2076,.F.);
#39829=ADVANCED_FACE('',(#4141),#2077,.F.);
#39830=ADVANCED_FACE('',(#4142),#2078,.F.);
#39831=ADVANCED_FACE('',(#4143),#2079,.F.);
#39832=ADVANCED_FACE('',(#4144),#2080,.F.);
#39833=ADVANCED_FACE('',(#4145),#2081,.F.);
#39834=ADVANCED_FACE('',(#4146),#2082,.F.);
#39835=ADVANCED_FACE('',(#4147),#2083,.F.);
#39836=ADVANCED_FACE('',(#4148),#2084,.F.);
#39837=ADVANCED_FACE('',(#4149),#2085,.F.);
#39838=ADVANCED_FACE('',(#4150),#2086,.F.);
#39839=ADVANCED_FACE('',(#4151),#2087,.F.);
#39840=ADVANCED_FACE('',(#4152),#2088,.F.);
#39841=ADVANCED_FACE('',(#4153),#2089,.F.);
#39842=ADVANCED_FACE('',(#4154),#2090,.F.);
#39843=ADVANCED_FACE('',(#4155),#2091,.F.);
#39844=ADVANCED_FACE('',(#4156),#2092,.F.);
#39845=ADVANCED_FACE('',(#4157),#2093,.F.);
#39846=ADVANCED_FACE('',(#4158),#2094,.F.);
#39847=ADVANCED_FACE('',(#4159),#2095,.F.);
#39848=ADVANCED_FACE('',(#4160),#2096,.F.);
#39849=ADVANCED_FACE('',(#4161),#2097,.F.);
#39850=ADVANCED_FACE('',(#4162),#2098,.F.);
#39851=ADVANCED_FACE('',(#4163),#2099,.F.);
#39852=ADVANCED_FACE('',(#4164),#2100,.F.);
#39853=ADVANCED_FACE('',(#4165),#2101,.F.);
#39854=ADVANCED_FACE('',(#4166),#2102,.F.);
#39855=ADVANCED_FACE('',(#4167),#2103,.F.);
#39856=ADVANCED_FACE('',(#4168),#2104,.F.);
#39857=ADVANCED_FACE('',(#4169),#2105,.F.);
#39858=ADVANCED_FACE('',(#4170),#2106,.F.);
#39859=ADVANCED_FACE('',(#4171),#2107,.F.);
#39860=ADVANCED_FACE('',(#4172),#2108,.F.);
#39861=ADVANCED_FACE('',(#4173),#2109,.F.);
#39862=ADVANCED_FACE('',(#4174),#2110,.F.);
#39863=ADVANCED_FACE('',(#4175),#2111,.F.);
#39864=ADVANCED_FACE('',(#4176),#2112,.F.);
#39865=ADVANCED_FACE('',(#4177),#2113,.F.);
#39866=ADVANCED_FACE('',(#4178),#2114,.F.);
#39867=ADVANCED_FACE('',(#4179),#2115,.F.);
#39868=ADVANCED_FACE('',(#4180),#2116,.F.);
#39869=ADVANCED_FACE('',(#4181),#2117,.F.);
#39870=ADVANCED_FACE('',(#4182),#2118,.F.);
#39871=ADVANCED_FACE('',(#4183),#2119,.F.);
#39872=ADVANCED_FACE('',(#4184),#2120,.F.);
#39873=ADVANCED_FACE('',(#4185),#2121,.F.);
#39874=ADVANCED_FACE('',(#4186),#2122,.F.);
#39875=ADVANCED_FACE('',(#4187),#2123,.F.);
#39876=ADVANCED_FACE('',(#4188),#2124,.F.);
#39877=ADVANCED_FACE('',(#4189),#2125,.F.);
#39878=ADVANCED_FACE('',(#4190),#2126,.F.);
#39879=ADVANCED_FACE('',(#4191),#2127,.F.);
#39880=ADVANCED_FACE('',(#4192),#2128,.F.);
#39881=ADVANCED_FACE('',(#4193),#2129,.F.);
#39882=ADVANCED_FACE('',(#4194),#2130,.F.);
#39883=ADVANCED_FACE('',(#4195),#2131,.F.);
#39884=ADVANCED_FACE('',(#4196),#2132,.F.);
#39885=ADVANCED_FACE('',(#4197),#2133,.F.);
#39886=ADVANCED_FACE('',(#4198),#2134,.F.);
#39887=ADVANCED_FACE('',(#4199),#2135,.F.);
#39888=ADVANCED_FACE('',(#4200),#2136,.F.);
#39889=ADVANCED_FACE('',(#4201),#2137,.F.);
#39890=ADVANCED_FACE('',(#4202),#2138,.F.);
#39891=ADVANCED_FACE('',(#4203),#2139,.F.);
#39892=ADVANCED_FACE('',(#4204),#2140,.F.);
#39893=ADVANCED_FACE('',(#4205),#2141,.F.);
#39894=ADVANCED_FACE('',(#4206),#2142,.F.);
#39895=ADVANCED_FACE('',(#4207),#2143,.F.);
#39896=ADVANCED_FACE('',(#4208),#2144,.F.);
#39897=ADVANCED_FACE('',(#4209),#2145,.F.);
#39898=ADVANCED_FACE('',(#4210),#2146,.F.);
#39899=ADVANCED_FACE('',(#4211),#2147,.F.);
#39900=ADVANCED_FACE('',(#4212),#2148,.F.);
#39901=ADVANCED_FACE('',(#4213),#2149,.F.);
#39902=ADVANCED_FACE('',(#4214),#2150,.F.);
#39903=ADVANCED_FACE('',(#4215),#2151,.F.);
#39904=ADVANCED_FACE('',(#4216),#2152,.F.);
#39905=ADVANCED_FACE('',(#4217),#2153,.F.);
#39906=ADVANCED_FACE('',(#4218),#2154,.F.);
#39907=ADVANCED_FACE('',(#4219),#2155,.F.);
#39908=ADVANCED_FACE('',(#4220),#2156,.F.);
#39909=ADVANCED_FACE('',(#4221),#2157,.F.);
#39910=ADVANCED_FACE('',(#4222),#2158,.F.);
#39911=ADVANCED_FACE('',(#4223),#2159,.F.);
#39912=ADVANCED_FACE('',(#4224),#2160,.F.);
#39913=ADVANCED_FACE('',(#4225),#2161,.F.);
#39914=ADVANCED_FACE('',(#4226),#2162,.F.);
#39915=ADVANCED_FACE('',(#4227),#2163,.F.);
#39916=ADVANCED_FACE('',(#4228),#2164,.F.);
#39917=ADVANCED_FACE('',(#4229),#2165,.F.);
#39918=ADVANCED_FACE('',(#4230),#2166,.F.);
#39919=ADVANCED_FACE('',(#4231),#2167,.F.);
#39920=ADVANCED_FACE('',(#4232),#2168,.F.);
#39921=ADVANCED_FACE('',(#4233),#2169,.F.);
#39922=ADVANCED_FACE('',(#4234),#2170,.F.);
#39923=ADVANCED_FACE('',(#4235),#2171,.F.);
#39924=ADVANCED_FACE('',(#4236),#2172,.F.);
#39925=ADVANCED_FACE('',(#4237),#2173,.F.);
#39926=ADVANCED_FACE('',(#4238),#2174,.F.);
#39927=ADVANCED_FACE('',(#4239),#2175,.F.);
#39928=ADVANCED_FACE('',(#4240),#2176,.F.);
#39929=ADVANCED_FACE('',(#4241),#2177,.F.);
#39930=ADVANCED_FACE('',(#4242),#2178,.F.);
#39931=ADVANCED_FACE('',(#4243),#2179,.F.);
#39932=ADVANCED_FACE('',(#4244),#2180,.F.);
#39933=CLOSED_SHELL('',(#38019,#38020,#38021,#38022,#38023,#38024,#38025,
#38026,#38027,#38028,#38029,#38030,#38031,#38032,#38033,#38034,#38035,#38036,
#38037,#38038,#38039,#38040,#38041,#38042,#38043,#38044,#38045,#38046,#38047,
#38048,#38049,#38050,#38051,#38052,#38053,#38054,#38055,#38056,#38057,#38058,
#38059,#38060,#38061,#38062,#38063,#38064,#38065,#38066,#38067,#38068,#38069,
#38070,#38071,#38072,#38073,#38074,#38075,#38076,#38077,#38078,#38079,#38080,
#38081,#38082,#38083,#38084,#38085,#38086,#38087,#38088,#38089,#38090,#38091,
#38092,#38093,#38094,#38095,#38096,#38097,#38098,#38099,#38100,#38101,#38102,
#38103,#38104,#38105,#38106,#38107,#38108,#38109,#38110,#38111,#38112,#38113,
#38114,#38115,#38116,#38117,#38118,#38119,#38120,#38121,#38122,#38123,#38124,
#38125,#38126,#38127,#38128,#38129,#38130,#38131,#38132,#38133,#38134,#38135,
#38136,#38137,#38138,#38139,#38140,#38141,#38142,#38143,#38144,#38145,#38146,
#38147,#38148,#38149,#38150,#38151,#38152,#38153,#38154,#38155,#38156,#38157,
#38158,#38159,#38160,#38161,#38162,#38163,#38164,#38165,#38166,#38167,#38168,
#38169,#38170,#38171,#38172,#38173,#38174,#38175,#38176,#38177,#38178,#38179,
#38180,#38181,#38182,#38183,#38184,#38185,#38186,#38187,#38188,#38189,#38190,
#38191,#38192,#38193,#38194,#38195,#38196,#38197,#38198,#38199,#38200,#38201,
#38202,#38203,#38204,#38205,#38206,#38207,#38208,#38209,#38210,#38211,#38212,
#38213,#38214,#38215,#38216,#38217,#38218,#38219,#38220,#38221,#38222,#38223,
#38224,#38225,#38226,#38227,#38228,#38229,#38230,#38231,#38232,#38233,#38234,
#38235,#38236,#38237,#38238,#38239,#38240,#38241,#38242,#38243,#38244,#38245,
#38246,#38247,#38248,#38249,#38250,#38251,#38252,#38253,#38254,#38255,#38256,
#38257,#38258,#38259,#38260,#38261,#38262,#38263,#38264,#38265,#38266,#38267,
#38268,#38269,#38270,#38271,#38272,#38273,#38274,#38275,#38276,#38277,#38278,
#38279,#38280,#38281,#38282,#38283,#38284,#38285,#38286,#38287,#38288,#38289,
#38290,#38291,#38292,#38293,#38294,#38295,#38296,#38297,#38298,#38299,#38300,
#38301,#38302,#38303,#38304,#38305,#38306,#38307,#38308,#38309,#38310,#38311,
#38312,#38313,#38314,#38315,#38316,#38317,#38318,#38319,#38320,#38321,#38322,
#38323,#38324,#38325,#38326,#38327,#38328,#38329,#38330,#38331,#38332,#38333,
#38334,#38335,#38336,#38337,#38338,#38339,#38340,#38341,#38342,#38343,#38344,
#38345,#38346,#38347,#38348,#38349,#38350,#38351,#38352,#38353,#38354,#38355,
#38356,#38357,#38358,#38359,#38360,#38361,#38362,#38363,#38364,#38365,#38366,
#38367,#38368,#38369,#38370,#38371,#38372,#38373,#38374,#38375,#38376,#38377,
#38378,#38379,#38380,#38381,#38382,#38383,#38384,#38385,#38386,#38387,#38388,
#38389,#38390,#38391,#38392,#38393,#38394,#38395,#38396,#38397,#38398,#38399,
#38400,#38401,#38402,#38403,#38404,#38405,#38406,#38407,#38408,#38409,#38410,
#38411,#38412,#38413,#38414,#38415,#38416,#38417,#38418,#38419,#38420,#38421,
#38422,#38423,#38424,#38425,#38426,#38427,#38428,#38429,#38430,#38431,#38432,
#38433,#38434,#38435,#38436,#38437,#38438,#38439,#38440,#38441,#38442,#38443,
#38444,#38445,#38446,#38447,#38448,#38449,#38450,#38451,#38452,#38453,#38454,
#38455,#38456,#38457,#38458,#38459,#38460,#38461,#38462,#38463,#38464,#38465,
#38466,#38467,#38468,#38469,#38470,#38471,#38472,#38473,#38474,#38475,#38476,
#38477,#38478,#38479,#38480,#38481,#38482,#38483,#38484,#38485,#38486,#38487,
#38488,#38489,#38490,#38491,#38492,#38493,#38494,#38495,#38496,#38497,#38498,
#38499,#38500,#38501,#38502,#38503,#38504,#38505,#38506,#38507,#38508,#38509,
#38510,#38511,#38512,#38513,#38514,#38515,#38516,#38517,#38518,#38519,#38520,
#38521,#38522,#38523,#38524,#38525,#38526,#38527,#38528,#38529,#38530,#38531,
#38532,#38533,#38534,#38535,#38536,#38537,#38538,#38539,#38540,#38541,#38542,
#38543,#38544,#38545,#38546,#38547,#38548,#38549,#38550,#38551,#38552,#38553,
#38554,#38555,#38556,#38557,#38558,#38559,#38560,#38561,#38562,#38563,#38564,
#38565,#38566,#38567,#38568,#38569,#38570,#38571,#38572,#38573,#38574,#38575,
#38576,#38577,#38578,#38579,#38580,#38581,#38582));
#39934=CLOSED_SHELL('',(#38583,#38584,#38585,#38586,#38587,#38588,#38589,
#38590,#38591,#38592,#38593,#38594,#38595,#38596,#38597,#38598,#38599,#38600,
#38601,#38602,#38603,#38604,#38605,#38606,#38607,#38608,#38609,#38610,#38611,
#38612,#38613,#38614,#38615,#38616,#38617,#38618,#38619,#38620,#38621,#38622,
#38623,#38624,#38625,#38626,#38627,#38628,#38629,#38630,#38631,#38632,#38633,
#38634,#38635,#38636,#38637,#38638,#38639,#38640,#38641,#38642,#38643,#38644,
#38645,#38646,#38647,#38648,#38649,#38650,#38651,#38652,#38653,#38654,#38655,
#38656,#38657,#38658,#38659,#38660,#38661,#38662,#38663,#38664,#38665,#38666,
#38667,#38668,#38669,#38670,#38671,#38672,#38673,#38674,#38675,#38676,#38677,
#38678,#38679,#38680,#38681,#38682,#38683,#38684,#38685,#38686,#38687,#38688,
#38689,#38690,#38691,#38692,#38693,#38694,#38695,#38696,#38697,#38698));
#39935=CLOSED_SHELL('',(#38699,#38700,#38701,#38702,#38703,#38704));
#39936=CLOSED_SHELL('',(#38705,#38706,#38707,#38708,#38709,#38710,#38711,
#38712,#38713,#38714,#38715,#38716,#38717,#38718,#38719,#38720,#38721,#38722,
#38723,#38724,#38725,#38726,#38727,#38728,#38729,#38730,#38731,#38732,#38733,
#38734,#38735,#38736,#38737,#38738,#38739,#38740,#38741,#38742,#38743,#38744,
#38745,#38746,#38747,#38748,#38749,#38750,#38751,#38752,#38753,#38754,#38755,
#38756,#38757,#38758,#38759,#38760,#38761,#38762,#38763,#38764));
#39937=CLOSED_SHELL('',(#38765,#38766,#38767,#38768,#38769,#38770,#38771,
#38772,#38773,#38774,#38775,#38776,#38777,#38778,#38779,#38780,#38781,#38782,
#38783,#38784,#38785,#38786,#38787,#38788,#38789,#38790,#38791,#38792,#38793,
#38794,#38795,#38796,#38797,#38798,#38799,#38800,#38801,#38802,#38803,#38804,
#38805,#38806,#38807,#38808,#38809,#38810,#38811,#38812,#38813,#38814,#38815,
#38816,#38817,#38818,#38819,#38820,#38821,#38822,#38823,#38824,#38825,#38826,
#38827,#38828,#38829,#38830,#38831,#38832,#38833,#38834,#38835,#38836,#38837,
#38838,#38839,#38840,#38841,#38842,#38843,#38844,#38845,#38846,#38847,#38848,
#38849,#38850,#38851,#38852,#38853,#38854,#38855,#38856,#38857,#38858,#38859,
#38860,#38861,#38862,#38863,#38864,#38865,#38866,#38867,#38868,#38869,#38870,
#38871,#38872,#38873,#38874,#38875,#38876,#38877,#38878,#38879,#38880,#38881,
#38882,#38883,#38884,#38885,#38886,#38887,#38888,#38889,#38890,#38891,#38892,
#38893,#38894,#38895,#38896,#38897,#38898,#38899,#38900,#38901,#38902,#38903,
#38904,#38905,#38906,#38907,#38908,#38909,#38910,#38911,#38912,#38913,#38914,
#38915,#38916,#38917,#38918,#38919,#38920,#38921,#38922,#38923,#38924,#38925,
#38926,#38927,#38928,#38929,#38930,#38931,#38932,#38933,#38934,#38935,#38936,
#38937,#38938,#38939,#38940,#38941,#38942,#38943,#38944,#38945,#38946,#38947,
#38948,#38949,#38950,#38951,#38952,#38953,#38954,#38955,#38956,#38957,#38958,
#38959,#38960,#38961,#38962,#38963,#38964,#38965,#38966,#38967,#38968,#38969,
#38970,#38971,#38972,#38973,#38974,#38975,#38976,#38977,#38978,#38979,#38980,
#38981,#38982,#38983,#38984,#38985,#38986,#38987,#38988,#38989,#38990,#38991,
#38992,#38993,#38994,#38995,#38996,#38997,#38998,#38999,#39000,#39001,#39002,
#39003,#39004,#39005,#39006,#39007,#39008,#39009,#39010,#39011,#39012,#39013,
#39014,#39015,#39016,#39017,#39018,#39019,#39020,#39021,#39022,#39023,#39024,
#39025,#39026,#39027,#39028,#39029,#39030,#39031,#39032,#39033,#39034,#39035,
#39036,#39037,#39038,#39039,#39040,#39041,#39042,#39043,#39044,#39045,#39046,
#39047,#39048,#39049,#39050,#39051,#39052,#39053,#39054,#39055,#39056,#39057,
#39058,#39059,#39060,#39061,#39062,#39063,#39064,#39065,#39066,#39067,#39068,
#39069,#39070,#39071,#39072,#39073,#39074,#39075,#39076,#39077,#39078,#39079,
#39080,#39081,#39082,#39083,#39084,#39085,#39086,#39087,#39088,#39089,#39090,
#39091,#39092,#39093,#39094,#39095,#39096,#39097,#39098,#39099,#39100,#39101,
#39102,#39103,#39104,#39105,#39106,#39107,#39108,#39109,#39110,#39111,#39112,
#39113,#39114,#39115,#39116,#39117,#39118,#39119,#39120,#39121,#39122,#39123,
#39124,#39125,#39126,#39127,#39128,#39129,#39130,#39131,#39132,#39133,#39134,
#39135,#39136,#39137,#39138,#39139,#39140,#39141,#39142,#39143,#39144,#39145,
#39146,#39147,#39148,#39149,#39150,#39151,#39152,#39153,#39154,#39155,#39156,
#39157,#39158,#39159,#39160,#39161,#39162,#39163,#39164,#39165,#39166,#39167,
#39168,#39169,#39170,#39171,#39172,#39173,#39174,#39175,#39176,#39177,#39178,
#39179,#39180,#39181,#39182,#39183,#39184,#39185,#39186,#39187,#39188,#39189,
#39190,#39191,#39192,#39193,#39194,#39195,#39196,#39197,#39198,#39199,#39200,
#39201,#39202,#39203,#39204,#39205,#39206,#39207,#39208,#39209,#39210,#39211,
#39212,#39213,#39214,#39215,#39216,#39217,#39218,#39219,#39220,#39221,#39222,
#39223,#39224,#39225,#39226,#39227,#39228,#39229,#39230,#39231,#39232,#39233,
#39234,#39235,#39236,#39237,#39238,#39239,#39240,#39241,#39242,#39243,#39244,
#39245,#39246,#39247,#39248,#39249,#39250,#39251,#39252,#39253,#39254,#39255,
#39256,#39257,#39258,#39259,#39260,#39261,#39262,#39263,#39264,#39265,#39266,
#39267,#39268,#39269,#39270,#39271,#39272,#39273,#39274,#39275,#39276,#39277,
#39278,#39279,#39280,#39281,#39282,#39283,#39284,#39285,#39286,#39287,#39288,
#39289,#39290,#39291,#39292,#39293,#39294,#39295,#39296,#39297,#39298,#39299,
#39300,#39301,#39302,#39303,#39304,#39305,#39306,#39307,#39308,#39309,#39310,
#39311,#39312,#39313,#39314,#39315,#39316,#39317,#39318,#39319,#39320,#39321,
#39322,#39323,#39324,#39325,#39326,#39327,#39328,#39329,#39330,#39331,#39332,
#39333,#39334,#39335,#39336,#39337,#39338,#39339,#39340,#39341,#39342,#39343,
#39344,#39345,#39346,#39347,#39348,#39349,#39350,#39351,#39352,#39353,#39354,
#39355,#39356,#39357,#39358,#39359,#39360,#39361,#39362,#39363,#39364,#39365,
#39366,#39367,#39368,#39369,#39370,#39371,#39372,#39373,#39374,#39375,#39376,
#39377,#39378,#39379,#39380,#39381,#39382,#39383,#39384,#39385,#39386,#39387,
#39388,#39389,#39390,#39391,#39392,#39393,#39394,#39395,#39396,#39397,#39398,
#39399,#39400,#39401,#39402,#39403,#39404,#39405,#39406,#39407,#39408,#39409,
#39410,#39411,#39412,#39413,#39414,#39415,#39416,#39417,#39418,#39419,#39420,
#39421,#39422,#39423,#39424,#39425,#39426,#39427,#39428,#39429,#39430,#39431,
#39432,#39433,#39434,#39435,#39436,#39437,#39438,#39439,#39440,#39441,#39442,
#39443,#39444,#39445,#39446,#39447,#39448,#39449,#39450,#39451,#39452,#39453,
#39454,#39455,#39456,#39457,#39458,#39459,#39460,#39461,#39462,#39463,#39464,
#39465,#39466,#39467,#39468,#39469,#39470,#39471,#39472,#39473,#39474,#39475,
#39476,#39477,#39478,#39479,#39480,#39481,#39482,#39483,#39484,#39485,#39486,
#39487,#39488,#39489,#39490,#39491,#39492,#39493,#39494,#39495,#39496,#39497,
#39498,#39499,#39500,#39501,#39502,#39503,#39504,#39505,#39506,#39507,#39508,
#39509,#39510,#39511,#39512,#39513,#39514,#39515,#39516,#39517,#39518,#39519,
#39520,#39521,#39522,#39523,#39524,#39525,#39526,#39527,#39528,#39529,#39530,
#39531,#39532,#39533,#39534,#39535,#39536,#39537,#39538,#39539,#39540,#39541,
#39542,#39543,#39544,#39545,#39546,#39547,#39548,#39549,#39550,#39551,#39552,
#39553,#39554,#39555,#39556,#39557,#39558,#39559,#39560,#39561,#39562,#39563,
#39564,#39565,#39566,#39567,#39568,#39569,#39570,#39571,#39572,#39573,#39574,
#39575,#39576,#39577,#39578,#39579,#39580,#39581,#39582,#39583,#39584,#39585,
#39586,#39587,#39588,#39589,#39590,#39591,#39592,#39593,#39594,#39595,#39596,
#39597,#39598,#39599,#39600,#39601,#39602,#39603,#39604,#39605,#39606,#39607,
#39608,#39609,#39610,#39611,#39612,#39613,#39614,#39615,#39616,#39617,#39618,
#39619,#39620,#39621,#39622,#39623,#39624,#39625,#39626,#39627,#39628,#39629,
#39630,#39631,#39632,#39633,#39634,#39635,#39636,#39637,#39638,#39639,#39640,
#39641,#39642,#39643,#39644,#39645,#39646,#39647,#39648,#39649,#39650,#39651,
#39652,#39653,#39654,#39655,#39656,#39657,#39658,#39659,#39660,#39661,#39662,
#39663,#39664,#39665,#39666,#39667,#39668,#39669,#39670,#39671,#39672,#39673,
#39674,#39675,#39676,#39677,#39678,#39679,#39680,#39681,#39682,#39683,#39684,
#39685,#39686,#39687,#39688,#39689,#39690,#39691,#39692,#39693,#39694,#39695,
#39696,#39697,#39698,#39699,#39700,#39701,#39702,#39703,#39704,#39705,#39706,
#39707,#39708,#39709,#39710,#39711,#39712,#39713,#39714,#39715,#39716,#39717,
#39718,#39719,#39720,#39721,#39722,#39723,#39724,#39725,#39726,#39727,#39728,
#39729,#39730,#39731,#39732,#39733,#39734,#39735,#39736,#39737,#39738,#39739,
#39740,#39741,#39742,#39743,#39744,#39745,#39746,#39747,#39748,#39749,#39750,
#39751,#39752,#39753,#39754,#39755,#39756,#39757,#39758,#39759,#39760,#39761,
#39762,#39763,#39764,#39765,#39766,#39767,#39768,#39769,#39770,#39771,#39772,
#39773,#39774,#39775,#39776,#39777,#39778,#39779,#39780,#39781,#39782,#39783,
#39784,#39785,#39786,#39787,#39788,#39789,#39790,#39791,#39792,#39793,#39794,
#39795,#39796,#39797,#39798,#39799,#39800,#39801,#39802,#39803,#39804,#39805,
#39806,#39807,#39808,#39809,#39810,#39811,#39812,#39813,#39814,#39815,#39816,
#39817,#39818,#39819,#39820,#39821,#39822,#39823,#39824,#39825,#39826,#39827,
#39828,#39829,#39830,#39831,#39832,#39833,#39834,#39835,#39836,#39837,#39838,
#39839,#39840,#39841,#39842,#39843,#39844,#39845,#39846,#39847,#39848,#39849,
#39850,#39851,#39852,#39853,#39854,#39855,#39856,#39857,#39858,#39859,#39860,
#39861,#39862,#39863,#39864,#39865,#39866,#39867,#39868,#39869,#39870,#39871,
#39872,#39873,#39874,#39875,#39876,#39877,#39878,#39879,#39880,#39881,#39882,
#39883,#39884,#39885,#39886,#39887,#39888,#39889,#39890,#39891,#39892,#39893,
#39894,#39895,#39896,#39897,#39898,#39899,#39900,#39901,#39902,#39903,#39904,
#39905,#39906,#39907,#39908,#39909,#39910,#39911,#39912,#39913,#39914,#39915,
#39916,#39917,#39918,#39919,#39920,#39921,#39922,#39923,#39924,#39925,#39926,
#39927,#39928,#39929,#39930,#39931,#39932));
#39938=DERIVED_UNIT_ELEMENT(#39946,1.);
#39939=DERIVED_UNIT_ELEMENT(#65306,-3.);
#39940=DERIVED_UNIT_ELEMENT(#39946,1.);
#39941=DERIVED_UNIT_ELEMENT(#65306,-3.);
#39942=DERIVED_UNIT_ELEMENT(#39946,1.);
#39943=DERIVED_UNIT_ELEMENT(#65306,-3.);
#39944=DERIVED_UNIT_ELEMENT(#39946,1.);
#39945=DERIVED_UNIT_ELEMENT(#65306,-3.);
#39946=(
MASS_UNIT()
NAMED_UNIT(*)
SI_UNIT(.KILO.,.GRAM.)
);
#39947=DERIVED_UNIT((#39938,#39939));
#39948=DERIVED_UNIT((#39940,#39941));
#39949=DERIVED_UNIT((#39942,#39943));
#39950=DERIVED_UNIT((#39944,#39945));
#39951=MEASURE_REPRESENTATION_ITEM('density measure',
POSITIVE_RATIO_MEASURE(7850.),#39947);
#39952=MEASURE_REPRESENTATION_ITEM('density measure',
POSITIVE_RATIO_MEASURE(7850.),#39948);
#39953=MEASURE_REPRESENTATION_ITEM('density measure',
POSITIVE_RATIO_MEASURE(7850.),#39949);
#39954=MEASURE_REPRESENTATION_ITEM('density measure',
POSITIVE_RATIO_MEASURE(7850.),#39950);
#39955=PROPERTY_DEFINITION_REPRESENTATION(#39975,#39963);
#39956=PROPERTY_DEFINITION_REPRESENTATION(#39976,#39964);
#39957=PROPERTY_DEFINITION_REPRESENTATION(#39977,#39965);
#39958=PROPERTY_DEFINITION_REPRESENTATION(#39978,#39966);
#39959=PROPERTY_DEFINITION_REPRESENTATION(#39979,#39967);
#39960=PROPERTY_DEFINITION_REPRESENTATION(#39980,#39968);
#39961=PROPERTY_DEFINITION_REPRESENTATION(#39981,#39969);
#39962=PROPERTY_DEFINITION_REPRESENTATION(#39982,#39970);
#39963=REPRESENTATION('material name',(#39971),#65300);
#39964=REPRESENTATION('density',(#39951),#65300);
#39965=REPRESENTATION('material name',(#39972),#65301);
#39966=REPRESENTATION('density',(#39952),#65301);
#39967=REPRESENTATION('material name',(#39973),#65302);
#39968=REPRESENTATION('density',(#39953),#65302);
#39969=REPRESENTATION('material name',(#39974),#65303);
#39970=REPRESENTATION('density',(#39954),#65303);
#39971=DESCRIPTIVE_REPRESENTATION_ITEM('Steel','Steel');
#39972=DESCRIPTIVE_REPRESENTATION_ITEM('Steel','Steel');
#39973=DESCRIPTIVE_REPRESENTATION_ITEM('Steel','Steel');
#39974=DESCRIPTIVE_REPRESENTATION_ITEM('Steel','Steel');
#39975=PROPERTY_DEFINITION('material property','material name',#65330);
#39976=PROPERTY_DEFINITION('material property','density of part',#65330);
#39977=PROPERTY_DEFINITION('material property','material name',#65331);
#39978=PROPERTY_DEFINITION('material property','density of part',#65331);
#39979=PROPERTY_DEFINITION('material property','material name',#65332);
#39980=PROPERTY_DEFINITION('material property','density of part',#65332);
#39981=PROPERTY_DEFINITION('material property','material name',#65333);
#39982=PROPERTY_DEFINITION('material property','density of part',#65333);
#39983=AXIS2_PLACEMENT_3D('',#52451,#42514,#42515);
#39984=AXIS2_PLACEMENT_3D('',#52452,#42516,#42517);
#39985=AXIS2_PLACEMENT_3D('',#52453,#42518,#42519);
#39986=AXIS2_PLACEMENT_3D('',#52455,#42520,#42521);
#39987=AXIS2_PLACEMENT_3D('',#52458,#42523,#42524);
#39988=AXIS2_PLACEMENT_3D('',#52459,#42525,#42526);
#39989=AXIS2_PLACEMENT_3D('',#52461,#42527,#42528);
#39990=AXIS2_PLACEMENT_3D('',#52464,#42530,#42531);
#39991=AXIS2_PLACEMENT_3D('',#52465,#42532,#42533);
#39992=AXIS2_PLACEMENT_3D('',#52467,#42534,#42535);
#39993=AXIS2_PLACEMENT_3D('',#52470,#42537,#42538);
#39994=AXIS2_PLACEMENT_3D('',#52471,#42539,#42540);
#39995=AXIS2_PLACEMENT_3D('',#52473,#42541,#42542);
#39996=AXIS2_PLACEMENT_3D('',#52476,#42544,#42545);
#39997=AXIS2_PLACEMENT_3D('',#52477,#42546,#42547);
#39998=AXIS2_PLACEMENT_3D('',#52479,#42548,#42549);
#39999=AXIS2_PLACEMENT_3D('',#52482,#42551,#42552);
#40000=AXIS2_PLACEMENT_3D('',#52483,#42553,#42554);
#40001=AXIS2_PLACEMENT_3D('',#52485,#42555,#42556);
#40002=AXIS2_PLACEMENT_3D('',#52488,#42558,#42559);
#40003=AXIS2_PLACEMENT_3D('',#52489,#42560,#42561);
#40004=AXIS2_PLACEMENT_3D('',#52492,#42562,#42563);
#40005=AXIS2_PLACEMENT_3D('',#52496,#42565,#42566);
#40006=AXIS2_PLACEMENT_3D('',#52498,#42568,#42569);
#40007=AXIS2_PLACEMENT_3D('',#52501,#42570,#42571);
#40008=AXIS2_PLACEMENT_3D('',#52505,#42573,#42574);
#40009=AXIS2_PLACEMENT_3D('',#52507,#42576,#42577);
#40010=AXIS2_PLACEMENT_3D('',#52510,#42578,#42579);
#40011=AXIS2_PLACEMENT_3D('',#52514,#42581,#42582);
#40012=AXIS2_PLACEMENT_3D('',#52516,#42584,#42585);
#40013=AXIS2_PLACEMENT_3D('',#52519,#42586,#42587);
#40014=AXIS2_PLACEMENT_3D('',#52523,#42589,#42590);
#40015=AXIS2_PLACEMENT_3D('',#52525,#42592,#42593);
#40016=AXIS2_PLACEMENT_3D('',#52528,#42594,#42595);
#40017=AXIS2_PLACEMENT_3D('',#52532,#42597,#42598);
#40018=AXIS2_PLACEMENT_3D('',#52534,#42600,#42601);
#40019=AXIS2_PLACEMENT_3D('',#52537,#42602,#42603);
#40020=AXIS2_PLACEMENT_3D('',#52541,#42605,#42606);
#40021=AXIS2_PLACEMENT_3D('',#52543,#42608,#42609);
#40022=AXIS2_PLACEMENT_3D('',#52546,#42610,#42611);
#40023=AXIS2_PLACEMENT_3D('',#52550,#42613,#42614);
#40024=AXIS2_PLACEMENT_3D('',#52552,#42616,#42617);
#40025=AXIS2_PLACEMENT_3D('',#52555,#42618,#42619);
#40026=AXIS2_PLACEMENT_3D('',#52559,#42621,#42622);
#40027=AXIS2_PLACEMENT_3D('',#52561,#42624,#42625);
#40028=AXIS2_PLACEMENT_3D('',#52564,#42626,#42627);
#40029=AXIS2_PLACEMENT_3D('',#52568,#42629,#42630);
#40030=AXIS2_PLACEMENT_3D('',#52570,#42632,#42633);
#40031=AXIS2_PLACEMENT_3D('',#52573,#42634,#42635);
#40032=AXIS2_PLACEMENT_3D('',#52577,#42637,#42638);
#40033=AXIS2_PLACEMENT_3D('',#52579,#42640,#42641);
#40034=AXIS2_PLACEMENT_3D('',#52582,#42642,#42643);
#40035=AXIS2_PLACEMENT_3D('',#52586,#42645,#42646);
#40036=AXIS2_PLACEMENT_3D('',#52588,#42648,#42649);
#40037=AXIS2_PLACEMENT_3D('',#52591,#42650,#42651);
#40038=AXIS2_PLACEMENT_3D('',#52595,#42653,#42654);
#40039=AXIS2_PLACEMENT_3D('',#52597,#42656,#42657);
#40040=AXIS2_PLACEMENT_3D('',#52600,#42658,#42659);
#40041=AXIS2_PLACEMENT_3D('',#52604,#42661,#42662);
#40042=AXIS2_PLACEMENT_3D('',#52606,#42664,#42665);
#40043=AXIS2_PLACEMENT_3D('',#52609,#42666,#42667);
#40044=AXIS2_PLACEMENT_3D('',#52613,#42669,#42670);
#40045=AXIS2_PLACEMENT_3D('',#52615,#42672,#42673);
#40046=AXIS2_PLACEMENT_3D('',#52618,#42674,#42675);
#40047=AXIS2_PLACEMENT_3D('',#52622,#42677,#42678);
#40048=AXIS2_PLACEMENT_3D('',#52624,#42680,#42681);
#40049=AXIS2_PLACEMENT_3D('',#52627,#42682,#42683);
#40050=AXIS2_PLACEMENT_3D('',#52631,#42685,#42686);
#40051=AXIS2_PLACEMENT_3D('',#52633,#42688,#42689);
#40052=AXIS2_PLACEMENT_3D('',#52636,#42690,#42691);
#40053=AXIS2_PLACEMENT_3D('',#52640,#42693,#42694);
#40054=AXIS2_PLACEMENT_3D('',#52642,#42696,#42697);
#40055=AXIS2_PLACEMENT_3D('',#52645,#42698,#42699);
#40056=AXIS2_PLACEMENT_3D('',#52649,#42701,#42702);
#40057=AXIS2_PLACEMENT_3D('',#52651,#42704,#42705);
#40058=AXIS2_PLACEMENT_3D('',#52654,#42706,#42707);
#40059=AXIS2_PLACEMENT_3D('',#52658,#42709,#42710);
#40060=AXIS2_PLACEMENT_3D('',#52660,#42712,#42713);
#40061=AXIS2_PLACEMENT_3D('',#52663,#42714,#42715);
#40062=AXIS2_PLACEMENT_3D('',#52667,#42717,#42718);
#40063=AXIS2_PLACEMENT_3D('',#52669,#42720,#42721);
#40064=AXIS2_PLACEMENT_3D('',#52672,#42722,#42723);
#40065=AXIS2_PLACEMENT_3D('',#52676,#42725,#42726);
#40066=AXIS2_PLACEMENT_3D('',#52678,#42728,#42729);
#40067=AXIS2_PLACEMENT_3D('',#52681,#42730,#42731);
#40068=AXIS2_PLACEMENT_3D('',#52685,#42733,#42734);
#40069=AXIS2_PLACEMENT_3D('',#52687,#42736,#42737);
#40070=AXIS2_PLACEMENT_3D('',#52690,#42738,#42739);
#40071=AXIS2_PLACEMENT_3D('',#52694,#42741,#42742);
#40072=AXIS2_PLACEMENT_3D('',#52696,#42744,#42745);
#40073=AXIS2_PLACEMENT_3D('',#52699,#42746,#42747);
#40074=AXIS2_PLACEMENT_3D('',#52703,#42749,#42750);
#40075=AXIS2_PLACEMENT_3D('',#52705,#42752,#42753);
#40076=AXIS2_PLACEMENT_3D('',#52708,#42754,#42755);
#40077=AXIS2_PLACEMENT_3D('',#52712,#42757,#42758);
#40078=AXIS2_PLACEMENT_3D('',#52714,#42760,#42761);
#40079=AXIS2_PLACEMENT_3D('',#52717,#42762,#42763);
#40080=AXIS2_PLACEMENT_3D('',#52721,#42765,#42766);
#40081=AXIS2_PLACEMENT_3D('',#52723,#42768,#42769);
#40082=AXIS2_PLACEMENT_3D('',#52726,#42770,#42771);
#40083=AXIS2_PLACEMENT_3D('',#52730,#42773,#42774);
#40084=AXIS2_PLACEMENT_3D('',#52732,#42776,#42777);
#40085=AXIS2_PLACEMENT_3D('',#52735,#42778,#42779);
#40086=AXIS2_PLACEMENT_3D('',#52739,#42781,#42782);
#40087=AXIS2_PLACEMENT_3D('',#52741,#42784,#42785);
#40088=AXIS2_PLACEMENT_3D('',#52744,#42786,#42787);
#40089=AXIS2_PLACEMENT_3D('',#52748,#42789,#42790);
#40090=AXIS2_PLACEMENT_3D('',#52750,#42792,#42793);
#40091=AXIS2_PLACEMENT_3D('',#52753,#42794,#42795);
#40092=AXIS2_PLACEMENT_3D('',#52757,#42797,#42798);
#40093=AXIS2_PLACEMENT_3D('',#52759,#42800,#42801);
#40094=AXIS2_PLACEMENT_3D('',#52762,#42802,#42803);
#40095=AXIS2_PLACEMENT_3D('',#52766,#42805,#42806);
#40096=AXIS2_PLACEMENT_3D('',#52768,#42808,#42809);
#40097=AXIS2_PLACEMENT_3D('',#52771,#42810,#42811);
#40098=AXIS2_PLACEMENT_3D('',#52775,#42813,#42814);
#40099=AXIS2_PLACEMENT_3D('',#52777,#42816,#42817);
#40100=AXIS2_PLACEMENT_3D('',#52780,#42818,#42819);
#40101=AXIS2_PLACEMENT_3D('',#52784,#42821,#42822);
#40102=AXIS2_PLACEMENT_3D('',#52786,#42824,#42825);
#40103=AXIS2_PLACEMENT_3D('',#52789,#42826,#42827);
#40104=AXIS2_PLACEMENT_3D('',#52793,#42829,#42830);
#40105=AXIS2_PLACEMENT_3D('',#52795,#42832,#42833);
#40106=AXIS2_PLACEMENT_3D('',#52798,#42834,#42835);
#40107=AXIS2_PLACEMENT_3D('',#52802,#42837,#42838);
#40108=AXIS2_PLACEMENT_3D('',#52804,#42840,#42841);
#40109=AXIS2_PLACEMENT_3D('',#52807,#42842,#42843);
#40110=AXIS2_PLACEMENT_3D('',#52811,#42845,#42846);
#40111=AXIS2_PLACEMENT_3D('',#52813,#42848,#42849);
#40112=AXIS2_PLACEMENT_3D('',#52816,#42850,#42851);
#40113=AXIS2_PLACEMENT_3D('',#52820,#42853,#42854);
#40114=AXIS2_PLACEMENT_3D('',#52822,#42856,#42857);
#40115=AXIS2_PLACEMENT_3D('',#52825,#42858,#42859);
#40116=AXIS2_PLACEMENT_3D('',#52829,#42861,#42862);
#40117=AXIS2_PLACEMENT_3D('',#52831,#42864,#42865);
#40118=AXIS2_PLACEMENT_3D('',#52834,#42866,#42867);
#40119=AXIS2_PLACEMENT_3D('',#52838,#42869,#42870);
#40120=AXIS2_PLACEMENT_3D('',#52840,#42872,#42873);
#40121=AXIS2_PLACEMENT_3D('',#52843,#42874,#42875);
#40122=AXIS2_PLACEMENT_3D('',#52847,#42877,#42878);
#40123=AXIS2_PLACEMENT_3D('',#52849,#42880,#42881);
#40124=AXIS2_PLACEMENT_3D('',#52852,#42882,#42883);
#40125=AXIS2_PLACEMENT_3D('',#52856,#42885,#42886);
#40126=AXIS2_PLACEMENT_3D('',#52858,#42888,#42889);
#40127=AXIS2_PLACEMENT_3D('',#52861,#42890,#42891);
#40128=AXIS2_PLACEMENT_3D('',#52865,#42893,#42894);
#40129=AXIS2_PLACEMENT_3D('',#52867,#42896,#42897);
#40130=AXIS2_PLACEMENT_3D('',#52870,#42898,#42899);
#40131=AXIS2_PLACEMENT_3D('',#52874,#42901,#42902);
#40132=AXIS2_PLACEMENT_3D('',#52876,#42904,#42905);
#40133=AXIS2_PLACEMENT_3D('',#52879,#42906,#42907);
#40134=AXIS2_PLACEMENT_3D('',#52883,#42909,#42910);
#40135=AXIS2_PLACEMENT_3D('',#52885,#42912,#42913);
#40136=AXIS2_PLACEMENT_3D('',#52888,#42914,#42915);
#40137=AXIS2_PLACEMENT_3D('',#52892,#42917,#42918);
#40138=AXIS2_PLACEMENT_3D('',#52894,#42920,#42921);
#40139=AXIS2_PLACEMENT_3D('',#52897,#42922,#42923);
#40140=AXIS2_PLACEMENT_3D('',#52901,#42925,#42926);
#40141=AXIS2_PLACEMENT_3D('',#52903,#42928,#42929);
#40142=AXIS2_PLACEMENT_3D('',#52906,#42930,#42931);
#40143=AXIS2_PLACEMENT_3D('',#52910,#42933,#42934);
#40144=AXIS2_PLACEMENT_3D('',#52912,#42936,#42937);
#40145=AXIS2_PLACEMENT_3D('',#52915,#42938,#42939);
#40146=AXIS2_PLACEMENT_3D('',#52919,#42941,#42942);
#40147=AXIS2_PLACEMENT_3D('',#52921,#42944,#42945);
#40148=AXIS2_PLACEMENT_3D('',#52924,#42946,#42947);
#40149=AXIS2_PLACEMENT_3D('',#52928,#42949,#42950);
#40150=AXIS2_PLACEMENT_3D('',#52930,#42952,#42953);
#40151=AXIS2_PLACEMENT_3D('',#52933,#42954,#42955);
#40152=AXIS2_PLACEMENT_3D('',#52937,#42957,#42958);
#40153=AXIS2_PLACEMENT_3D('',#52939,#42960,#42961);
#40154=AXIS2_PLACEMENT_3D('',#52942,#42962,#42963);
#40155=AXIS2_PLACEMENT_3D('',#52946,#42965,#42966);
#40156=AXIS2_PLACEMENT_3D('',#52948,#42968,#42969);
#40157=AXIS2_PLACEMENT_3D('',#52951,#42970,#42971);
#40158=AXIS2_PLACEMENT_3D('',#52955,#42973,#42974);
#40159=AXIS2_PLACEMENT_3D('',#52957,#42976,#42977);
#40160=AXIS2_PLACEMENT_3D('',#52960,#42978,#42979);
#40161=AXIS2_PLACEMENT_3D('',#52964,#42981,#42982);
#40162=AXIS2_PLACEMENT_3D('',#52966,#42984,#42985);
#40163=AXIS2_PLACEMENT_3D('',#52969,#42986,#42987);
#40164=AXIS2_PLACEMENT_3D('',#52973,#42989,#42990);
#40165=AXIS2_PLACEMENT_3D('',#52975,#42992,#42993);
#40166=AXIS2_PLACEMENT_3D('',#52978,#42994,#42995);
#40167=AXIS2_PLACEMENT_3D('',#52982,#42997,#42998);
#40168=AXIS2_PLACEMENT_3D('',#52984,#43000,#43001);
#40169=AXIS2_PLACEMENT_3D('',#52987,#43002,#43003);
#40170=AXIS2_PLACEMENT_3D('',#52991,#43005,#43006);
#40171=AXIS2_PLACEMENT_3D('',#52993,#43008,#43009);
#40172=AXIS2_PLACEMENT_3D('',#52996,#43010,#43011);
#40173=AXIS2_PLACEMENT_3D('',#53000,#43013,#43014);
#40174=AXIS2_PLACEMENT_3D('',#53002,#43016,#43017);
#40175=AXIS2_PLACEMENT_3D('',#53005,#43018,#43019);
#40176=AXIS2_PLACEMENT_3D('',#53009,#43021,#43022);
#40177=AXIS2_PLACEMENT_3D('',#53011,#43024,#43025);
#40178=AXIS2_PLACEMENT_3D('',#53014,#43026,#43027);
#40179=AXIS2_PLACEMENT_3D('',#53018,#43029,#43030);
#40180=AXIS2_PLACEMENT_3D('',#53020,#43032,#43033);
#40181=AXIS2_PLACEMENT_3D('',#53023,#43034,#43035);
#40182=AXIS2_PLACEMENT_3D('',#53027,#43037,#43038);
#40183=AXIS2_PLACEMENT_3D('',#53029,#43040,#43041);
#40184=AXIS2_PLACEMENT_3D('',#53032,#43042,#43043);
#40185=AXIS2_PLACEMENT_3D('',#53036,#43045,#43046);
#40186=AXIS2_PLACEMENT_3D('',#53038,#43048,#43049);
#40187=AXIS2_PLACEMENT_3D('',#53041,#43050,#43051);
#40188=AXIS2_PLACEMENT_3D('',#53045,#43053,#43054);
#40189=AXIS2_PLACEMENT_3D('',#53047,#43056,#43057);
#40190=AXIS2_PLACEMENT_3D('',#53050,#43058,#43059);
#40191=AXIS2_PLACEMENT_3D('',#53054,#43061,#43062);
#40192=AXIS2_PLACEMENT_3D('',#53056,#43064,#43065);
#40193=AXIS2_PLACEMENT_3D('',#53059,#43066,#43067);
#40194=AXIS2_PLACEMENT_3D('',#53063,#43069,#43070);
#40195=AXIS2_PLACEMENT_3D('',#53065,#43072,#43073);
#40196=AXIS2_PLACEMENT_3D('',#53068,#43074,#43075);
#40197=AXIS2_PLACEMENT_3D('',#53072,#43077,#43078);
#40198=AXIS2_PLACEMENT_3D('',#53074,#43080,#43081);
#40199=AXIS2_PLACEMENT_3D('',#53077,#43082,#43083);
#40200=AXIS2_PLACEMENT_3D('',#53081,#43085,#43086);
#40201=AXIS2_PLACEMENT_3D('',#53225,#43098,#43099);
#40202=AXIS2_PLACEMENT_3D('',#53227,#43100,#43101);
#40203=AXIS2_PLACEMENT_3D('',#53230,#43103,#43104);
#40204=AXIS2_PLACEMENT_3D('',#53231,#43105,#43106);
#40205=AXIS2_PLACEMENT_3D('',#53233,#43107,#43108);
#40206=AXIS2_PLACEMENT_3D('',#53236,#43110,#43111);
#40207=AXIS2_PLACEMENT_3D('',#53237,#43112,#43113);
#40208=AXIS2_PLACEMENT_3D('',#53239,#43114,#43115);
#40209=AXIS2_PLACEMENT_3D('',#53242,#43117,#43118);
#40210=AXIS2_PLACEMENT_3D('',#53243,#43119,#43120);
#40211=AXIS2_PLACEMENT_3D('',#53245,#43121,#43122);
#40212=AXIS2_PLACEMENT_3D('',#53248,#43124,#43125);
#40213=AXIS2_PLACEMENT_3D('',#53249,#43126,#43127);
#40214=AXIS2_PLACEMENT_3D('',#53251,#43128,#43129);
#40215=AXIS2_PLACEMENT_3D('',#53253,#43130,#43131);
#40216=AXIS2_PLACEMENT_3D('',#53254,#43132,#43133);
#40217=AXIS2_PLACEMENT_3D('',#53255,#43134,#43135);
#40218=AXIS2_PLACEMENT_3D('',#53257,#43136,#43137);
#40219=AXIS2_PLACEMENT_3D('',#53259,#43138,#43139);
#40220=AXIS2_PLACEMENT_3D('',#53260,#43140,#43141);
#40221=AXIS2_PLACEMENT_3D('',#53261,#43142,#43143);
#40222=AXIS2_PLACEMENT_3D('',#53263,#43144,#43145);
#40223=AXIS2_PLACEMENT_3D('',#53264,#43146,#43147);
#40224=AXIS2_PLACEMENT_3D('',#53265,#43148,#43149);
#40225=AXIS2_PLACEMENT_3D('',#53267,#43150,#43151);
#40226=AXIS2_PLACEMENT_3D('',#53268,#43152,#43153);
#40227=AXIS2_PLACEMENT_3D('',#53269,#43154,#43155);
#40228=AXIS2_PLACEMENT_3D('',#53271,#43156,#43157);
#40229=AXIS2_PLACEMENT_3D('',#53274,#43159,#43160);
#40230=AXIS2_PLACEMENT_3D('',#53275,#43161,#43162);
#40231=AXIS2_PLACEMENT_3D('',#53277,#43163,#43164);
#40232=AXIS2_PLACEMENT_3D('',#53280,#43166,#43167);
#40233=AXIS2_PLACEMENT_3D('',#53281,#43168,#43169);
#40234=AXIS2_PLACEMENT_3D('',#53283,#43170,#43171);
#40235=AXIS2_PLACEMENT_3D('',#53286,#43173,#43174);
#40236=AXIS2_PLACEMENT_3D('',#53287,#43175,#43176);
#40237=AXIS2_PLACEMENT_3D('',#53289,#43177,#43178);
#40238=AXIS2_PLACEMENT_3D('',#53292,#43180,#43181);
#40239=AXIS2_PLACEMENT_3D('',#53331,#43184,#43185);
#40240=AXIS2_PLACEMENT_3D('',#53340,#43189,#43190);
#40241=AXIS2_PLACEMENT_3D('',#53344,#43192,#43193);
#40242=AXIS2_PLACEMENT_3D('',#53368,#43205,#43206);
#40243=AXIS2_PLACEMENT_3D('',#53372,#43208,#43209);
#40244=AXIS2_PLACEMENT_3D('',#53452,#43250,#43251);
#40245=AXIS2_PLACEMENT_3D('',#53475,#43262,#43263);
#40246=AXIS2_PLACEMENT_3D('',#53479,#43265,#43266);
#40247=AXIS2_PLACEMENT_3D('',#53503,#43278,#43279);
#40248=AXIS2_PLACEMENT_3D('',#53507,#43281,#43282);
#40249=AXIS2_PLACEMENT_3D('',#53541,#43300,#43301);
#40250=AXIS2_PLACEMENT_3D('',#53544,#43304,#43305);
#40251=AXIS2_PLACEMENT_3D('',#53547,#43308,#43309);
#40252=AXIS2_PLACEMENT_3D('',#53556,#43313,#43314);
#40253=AXIS2_PLACEMENT_3D('',#53559,#43316,#43317);
#40254=AXIS2_PLACEMENT_3D('',#53592,#43334,#43335);
#40255=AXIS2_PLACEMENT_3D('',#53599,#43338,#43339);
#40256=AXIS2_PLACEMENT_3D('',#53603,#43341,#43342);
#40257=AXIS2_PLACEMENT_3D('',#53621,#43352,#43353);
#40258=AXIS2_PLACEMENT_3D('',#53624,#43356,#43357);
#40259=AXIS2_PLACEMENT_3D('',#53627,#43360,#43361);
#40260=AXIS2_PLACEMENT_3D('',#53642,#43368,#43369);
#40261=AXIS2_PLACEMENT_3D('',#53646,#43371,#43372);
#40262=AXIS2_PLACEMENT_3D('',#53652,#43376,#43377);
#40263=AXIS2_PLACEMENT_3D('',#53657,#43380,#43381);
#40264=AXIS2_PLACEMENT_3D('',#53662,#43384,#43385);
#40265=AXIS2_PLACEMENT_3D('',#53667,#43388,#43389);
#40266=AXIS2_PLACEMENT_3D('',#53672,#43392,#43393);
#40267=AXIS2_PLACEMENT_3D('',#53677,#43396,#43397);
#40268=AXIS2_PLACEMENT_3D('',#53682,#43400,#43401);
#40269=AXIS2_PLACEMENT_3D('',#53687,#43404,#43405);
#40270=AXIS2_PLACEMENT_3D('',#53692,#43408,#43409);
#40271=AXIS2_PLACEMENT_3D('',#53697,#43412,#43413);
#40272=AXIS2_PLACEMENT_3D('',#53702,#43416,#43417);
#40273=AXIS2_PLACEMENT_3D('',#53707,#43420,#43421);
#40274=AXIS2_PLACEMENT_3D('',#53711,#43423,#43424);
#40275=AXIS2_PLACEMENT_3D('',#53716,#43427,#43428);
#40276=AXIS2_PLACEMENT_3D('',#53721,#43431,#43432);
#40277=AXIS2_PLACEMENT_3D('',#53726,#43435,#43436);
#40278=AXIS2_PLACEMENT_3D('',#53731,#43439,#43440);
#40279=AXIS2_PLACEMENT_3D('',#53736,#43443,#43444);
#40280=AXIS2_PLACEMENT_3D('',#53741,#43447,#43448);
#40281=AXIS2_PLACEMENT_3D('',#53746,#43451,#43452);
#40282=AXIS2_PLACEMENT_3D('',#53751,#43455,#43456);
#40283=AXIS2_PLACEMENT_3D('',#53756,#43459,#43460);
#40284=AXIS2_PLACEMENT_3D('',#53761,#43463,#43464);
#40285=AXIS2_PLACEMENT_3D('',#53766,#43467,#43468);
#40286=AXIS2_PLACEMENT_3D('',#53771,#43471,#43472);
#40287=AXIS2_PLACEMENT_3D('',#53776,#43475,#43476);
#40288=AXIS2_PLACEMENT_3D('',#53781,#43479,#43480);
#40289=AXIS2_PLACEMENT_3D('',#53786,#43483,#43484);
#40290=AXIS2_PLACEMENT_3D('',#53791,#43487,#43488);
#40291=AXIS2_PLACEMENT_3D('',#53796,#43491,#43492);
#40292=AXIS2_PLACEMENT_3D('',#53801,#43495,#43496);
#40293=AXIS2_PLACEMENT_3D('',#53806,#43499,#43500);
#40294=AXIS2_PLACEMENT_3D('',#53811,#43503,#43504);
#40295=AXIS2_PLACEMENT_3D('',#53816,#43507,#43508);
#40296=AXIS2_PLACEMENT_3D('',#53821,#43511,#43512);
#40297=AXIS2_PLACEMENT_3D('',#53826,#43515,#43516);
#40298=AXIS2_PLACEMENT_3D('',#53832,#43520,#43521);
#40299=AXIS2_PLACEMENT_3D('',#53837,#43524,#43525);
#40300=AXIS2_PLACEMENT_3D('',#53842,#43528,#43529);
#40301=AXIS2_PLACEMENT_3D('',#53847,#43532,#43533);
#40302=AXIS2_PLACEMENT_3D('',#53852,#43536,#43537);
#40303=AXIS2_PLACEMENT_3D('',#53857,#43540,#43541);
#40304=AXIS2_PLACEMENT_3D('',#53862,#43544,#43545);
#40305=AXIS2_PLACEMENT_3D('',#53867,#43548,#43549);
#40306=AXIS2_PLACEMENT_3D('',#53872,#43552,#43553);
#40307=AXIS2_PLACEMENT_3D('',#53877,#43556,#43557);
#40308=AXIS2_PLACEMENT_3D('',#53882,#43560,#43561);
#40309=AXIS2_PLACEMENT_3D('',#53887,#43564,#43565);
#40310=AXIS2_PLACEMENT_3D('',#53888,#43566,#43567);
#40311=AXIS2_PLACEMENT_3D('',#53899,#43572,#43573);
#40312=AXIS2_PLACEMENT_3D('',#53903,#43575,#43576);
#40313=AXIS2_PLACEMENT_3D('',#53912,#43581,#43582);
#40314=AXIS2_PLACEMENT_3D('',#53917,#43585,#43586);
#40315=AXIS2_PLACEMENT_3D('',#53922,#43589,#43590);
#40316=AXIS2_PLACEMENT_3D('',#53927,#43593,#43594);
#40317=AXIS2_PLACEMENT_3D('',#53932,#43597,#43598);
#40318=AXIS2_PLACEMENT_3D('',#53937,#43601,#43602);
#40319=AXIS2_PLACEMENT_3D('',#53942,#43605,#43606);
#40320=AXIS2_PLACEMENT_3D('',#53947,#43609,#43610);
#40321=AXIS2_PLACEMENT_3D('',#53952,#43613,#43614);
#40322=AXIS2_PLACEMENT_3D('',#53957,#43617,#43618);
#40323=AXIS2_PLACEMENT_3D('',#53962,#43621,#43622);
#40324=AXIS2_PLACEMENT_3D('',#53967,#43625,#43626);
#40325=AXIS2_PLACEMENT_3D('',#53972,#43629,#43630);
#40326=AXIS2_PLACEMENT_3D('',#53978,#43634,#43635);
#40327=AXIS2_PLACEMENT_3D('',#53983,#43638,#43639);
#40328=AXIS2_PLACEMENT_3D('',#53988,#43642,#43643);
#40329=AXIS2_PLACEMENT_3D('',#53993,#43646,#43647);
#40330=AXIS2_PLACEMENT_3D('',#53998,#43650,#43651);
#40331=AXIS2_PLACEMENT_3D('',#54003,#43654,#43655);
#40332=AXIS2_PLACEMENT_3D('',#54008,#43658,#43659);
#40333=AXIS2_PLACEMENT_3D('',#54013,#43662,#43663);
#40334=AXIS2_PLACEMENT_3D('',#54018,#43666,#43667);
#40335=AXIS2_PLACEMENT_3D('',#54023,#43670,#43671);
#40336=AXIS2_PLACEMENT_3D('',#54028,#43674,#43675);
#40337=AXIS2_PLACEMENT_3D('',#54033,#43678,#43679);
#40338=AXIS2_PLACEMENT_3D('',#54038,#43682,#43683);
#40339=AXIS2_PLACEMENT_3D('',#54043,#43686,#43687);
#40340=AXIS2_PLACEMENT_3D('',#54048,#43690,#43691);
#40341=AXIS2_PLACEMENT_3D('',#54053,#43694,#43695);
#40342=AXIS2_PLACEMENT_3D('',#54058,#43698,#43699);
#40343=AXIS2_PLACEMENT_3D('',#54063,#43702,#43703);
#40344=AXIS2_PLACEMENT_3D('',#54068,#43706,#43707);
#40345=AXIS2_PLACEMENT_3D('',#54073,#43710,#43711);
#40346=AXIS2_PLACEMENT_3D('',#54078,#43714,#43715);
#40347=AXIS2_PLACEMENT_3D('',#54083,#43718,#43719);
#40348=AXIS2_PLACEMENT_3D('',#54088,#43722,#43723);
#40349=AXIS2_PLACEMENT_3D('',#54093,#43726,#43727);
#40350=AXIS2_PLACEMENT_3D('',#54097,#43729,#43730);
#40351=AXIS2_PLACEMENT_3D('',#54102,#43733,#43734);
#40352=AXIS2_PLACEMENT_3D('',#54107,#43737,#43738);
#40353=AXIS2_PLACEMENT_3D('',#54112,#43741,#43742);
#40354=AXIS2_PLACEMENT_3D('',#54117,#43745,#43746);
#40355=AXIS2_PLACEMENT_3D('',#54122,#43749,#43750);
#40356=AXIS2_PLACEMENT_3D('',#54127,#43753,#43754);
#40357=AXIS2_PLACEMENT_3D('',#54132,#43757,#43758);
#40358=AXIS2_PLACEMENT_3D('',#54137,#43761,#43762);
#40359=AXIS2_PLACEMENT_3D('',#54142,#43765,#43766);
#40360=AXIS2_PLACEMENT_3D('',#54147,#43769,#43770);
#40361=AXIS2_PLACEMENT_3D('',#54149,#43772,#43773);
#40362=AXIS2_PLACEMENT_3D('',#54155,#43777,#43778);
#40363=AXIS2_PLACEMENT_3D('',#54161,#43782,#43783);
#40364=AXIS2_PLACEMENT_3D('',#54170,#43788,#43789);
#40365=AXIS2_PLACEMENT_3D('',#54176,#43793,#43794);
#40366=AXIS2_PLACEMENT_3D('',#54185,#43799,#43800);
#40367=AXIS2_PLACEMENT_3D('',#54191,#43804,#43805);
#40368=AXIS2_PLACEMENT_3D('',#54197,#43809,#43810);
#40369=AXIS2_PLACEMENT_3D('',#54206,#43815,#43816);
#40370=AXIS2_PLACEMENT_3D('',#54215,#43821,#43822);
#40371=AXIS2_PLACEMENT_3D('',#54221,#43826,#43827);
#40372=AXIS2_PLACEMENT_3D('',#54230,#43832,#43833);
#40373=AXIS2_PLACEMENT_3D('',#54239,#43838,#43839);
#40374=AXIS2_PLACEMENT_3D('',#54245,#43843,#43844);
#40375=AXIS2_PLACEMENT_3D('',#54251,#43848,#43849);
#40376=AXIS2_PLACEMENT_3D('',#54260,#43854,#43855);
#40377=AXIS2_PLACEMENT_3D('',#54266,#43859,#43860);
#40378=AXIS2_PLACEMENT_3D('',#54275,#43865,#43866);
#40379=AXIS2_PLACEMENT_3D('',#54281,#43870,#43871);
#40380=AXIS2_PLACEMENT_3D('',#54287,#43875,#43876);
#40381=AXIS2_PLACEMENT_3D('',#54296,#43881,#43882);
#40382=AXIS2_PLACEMENT_3D('',#54305,#43887,#43888);
#40383=AXIS2_PLACEMENT_3D('',#54311,#43892,#43893);
#40384=AXIS2_PLACEMENT_3D('',#54320,#43898,#43899);
#40385=AXIS2_PLACEMENT_3D('',#54387,#43906,#43907);
#40386=AXIS2_PLACEMENT_3D('',#54388,#43908,#43909);
#40387=AXIS2_PLACEMENT_3D('',#54390,#43910,#43911);
#40388=AXIS2_PLACEMENT_3D('',#54396,#43912,#43913);
#40389=AXIS2_PLACEMENT_3D('',#54404,#43914,#43915);
#40390=AXIS2_PLACEMENT_3D('',#54408,#43917,#43918);
#40391=AXIS2_PLACEMENT_3D('',#54417,#43919,#43920);
#40392=AXIS2_PLACEMENT_3D('',#54428,#43923,#43924);
#40393=AXIS2_PLACEMENT_3D('',#54438,#43926,#43927);
#40394=AXIS2_PLACEMENT_3D('',#54448,#43928,#43929);
#40395=AXIS2_PLACEMENT_3D('',#54459,#43931,#43932);
#40396=AXIS2_PLACEMENT_3D('',#54463,#43934,#43935);
#40397=AXIS2_PLACEMENT_3D('',#54473,#43936,#43937);
#40398=AXIS2_PLACEMENT_3D('',#54477,#43939,#43940);
#40399=AXIS2_PLACEMENT_3D('',#54487,#43941,#43942);
#40400=AXIS2_PLACEMENT_3D('',#54491,#43944,#43945);
#40401=AXIS2_PLACEMENT_3D('',#54502,#43947,#43948);
#40402=AXIS2_PLACEMENT_3D('',#54511,#43949,#43950);
#40403=AXIS2_PLACEMENT_3D('',#54515,#43952,#43953);
#40404=AXIS2_PLACEMENT_3D('',#54528,#43955,#43956);
#40405=AXIS2_PLACEMENT_3D('',#54537,#43957,#43958);
#40406=AXIS2_PLACEMENT_3D('',#54548,#43960,#43961);
#40407=AXIS2_PLACEMENT_3D('',#54550,#43962,#43963);
#40408=AXIS2_PLACEMENT_3D('',#54560,#43964,#43965);
#40409=AXIS2_PLACEMENT_3D('',#54570,#43966,#43967);
#40410=AXIS2_PLACEMENT_3D('',#54580,#43968,#43969);
#40411=AXIS2_PLACEMENT_3D('',#54582,#43970,#43971);
#40412=AXIS2_PLACEMENT_3D('',#54592,#43972,#43973);
#40413=AXIS2_PLACEMENT_3D('',#54594,#43974,#43975);
#40414=AXIS2_PLACEMENT_3D('',#54603,#43976,#43977);
#40415=AXIS2_PLACEMENT_3D('',#54605,#43978,#43979);
#40416=AXIS2_PLACEMENT_3D('',#54616,#43980,#43981);
#40417=AXIS2_PLACEMENT_3D('',#54626,#43982,#43983);
#40418=AXIS2_PLACEMENT_3D('',#54628,#43984,#43985);
#40419=AXIS2_PLACEMENT_3D('',#54638,#43986,#43987);
#40420=AXIS2_PLACEMENT_3D('',#54648,#43988,#43989);
#40421=AXIS2_PLACEMENT_3D('',#54658,#43990,#43991);
#40422=AXIS2_PLACEMENT_3D('',#54660,#43992,#43993);
#40423=AXIS2_PLACEMENT_3D('',#54669,#43994,#43995);
#40424=AXIS2_PLACEMENT_3D('',#54670,#43996,#43997);
#40425=AXIS2_PLACEMENT_3D('',#54680,#43998,#43999);
#40426=AXIS2_PLACEMENT_3D('',#54682,#44000,#44001);
#40427=AXIS2_PLACEMENT_3D('',#54697,#44002,#44003);
#40428=AXIS2_PLACEMENT_3D('',#54699,#44004,#44005);
#40429=AXIS2_PLACEMENT_3D('',#54710,#44006,#44007);
#40430=AXIS2_PLACEMENT_3D('',#54712,#44008,#44009);
#40431=AXIS2_PLACEMENT_3D('',#54727,#44010,#44011);
#40432=AXIS2_PLACEMENT_3D('',#54737,#44012,#44013);
#40433=AXIS2_PLACEMENT_3D('',#54739,#44014,#44015);
#40434=AXIS2_PLACEMENT_3D('',#54754,#44016,#44017);
#40435=AXIS2_PLACEMENT_3D('',#54764,#44018,#44019);
#40436=AXIS2_PLACEMENT_3D('',#54779,#44020,#44021);
#40437=AXIS2_PLACEMENT_3D('',#54780,#44022,#44023);
#40438=AXIS2_PLACEMENT_3D('',#54782,#44024,#44025);
#40439=AXIS2_PLACEMENT_3D('',#54789,#44026,#44027);
#40440=AXIS2_PLACEMENT_3D('',#54822,#44028,#44029);
#40441=AXIS2_PLACEMENT_3D('',#54949,#44035,#44036);
#40442=AXIS2_PLACEMENT_3D('',#54960,#44041,#44042);
#40443=AXIS2_PLACEMENT_3D('',#54964,#44044,#44045);
#40444=AXIS2_PLACEMENT_3D('',#54980,#44053,#44054);
#40445=AXIS2_PLACEMENT_3D('',#54984,#44056,#44057);
#40446=AXIS2_PLACEMENT_3D('',#54988,#44059,#44060);
#40447=AXIS2_PLACEMENT_3D('',#54992,#44062,#44063);
#40448=AXIS2_PLACEMENT_3D('',#54996,#44065,#44066);
#40449=AXIS2_PLACEMENT_3D('',#55000,#44068,#44069);
#40450=AXIS2_PLACEMENT_3D('',#55002,#44071,#44072);
#40451=AXIS2_PLACEMENT_3D('',#55017,#44079,#44080);
#40452=AXIS2_PLACEMENT_3D('',#55021,#44082,#44083);
#40453=AXIS2_PLACEMENT_3D('',#55035,#44090,#44091);
#40454=AXIS2_PLACEMENT_3D('',#55039,#44093,#44094);
#40455=AXIS2_PLACEMENT_3D('',#55043,#44096,#44097);
#40456=AXIS2_PLACEMENT_3D('',#55047,#44099,#44100);
#40457=AXIS2_PLACEMENT_3D('',#55051,#44102,#44103);
#40458=AXIS2_PLACEMENT_3D('',#55054,#44105,#44106);
#40459=AXIS2_PLACEMENT_3D('',#55055,#44107,#44108);
#40460=AXIS2_PLACEMENT_3D('',#55060,#44112,#44113);
#40461=AXIS2_PLACEMENT_3D('',#55061,#44114,#44115);
#40462=AXIS2_PLACEMENT_3D('',#55066,#44119,#44120);
#40463=AXIS2_PLACEMENT_3D('',#55067,#44121,#44122);
#40464=AXIS2_PLACEMENT_3D('',#55072,#44126,#44127);
#40465=AXIS2_PLACEMENT_3D('',#55073,#44128,#44129);
#40466=AXIS2_PLACEMENT_3D('',#55078,#44133,#44134);
#40467=AXIS2_PLACEMENT_3D('',#55291,#44139,#44140);
#40468=AXIS2_PLACEMENT_3D('',#55292,#44141,#44142);
#40469=AXIS2_PLACEMENT_3D('',#55293,#44143,#44144);
#40470=AXIS2_PLACEMENT_3D('',#55296,#44147,#44148);
#40471=AXIS2_PLACEMENT_3D('',#55298,#44150,#44151);
#40472=AXIS2_PLACEMENT_3D('',#55301,#44154,#44155);
#40473=AXIS2_PLACEMENT_3D('',#55304,#44158,#44159);
#40474=AXIS2_PLACEMENT_3D('',#55306,#44161,#44162);
#40475=AXIS2_PLACEMENT_3D('',#55307,#44163,#44164);
#40476=AXIS2_PLACEMENT_3D('',#55520,#44169,#44170);
#40477=AXIS2_PLACEMENT_3D('',#55521,#44171,#44172);
#40478=AXIS2_PLACEMENT_3D('',#55522,#44173,#44174);
#40479=AXIS2_PLACEMENT_3D('',#55525,#44177,#44178);
#40480=AXIS2_PLACEMENT_3D('',#55527,#44180,#44181);
#40481=AXIS2_PLACEMENT_3D('',#55530,#44184,#44185);
#40482=AXIS2_PLACEMENT_3D('',#55533,#44188,#44189);
#40483=AXIS2_PLACEMENT_3D('',#55535,#44191,#44192);
#40484=AXIS2_PLACEMENT_3D('',#55536,#44193,#44194);
#40485=AXIS2_PLACEMENT_3D('',#55537,#44195,#44196);
#40486=AXIS2_PLACEMENT_3D('',#55538,#44197,#44198);
#40487=AXIS2_PLACEMENT_3D('',#55539,#44199,#44200);
#40488=AXIS2_PLACEMENT_3D('',#55540,#44201,#44202);
#40489=AXIS2_PLACEMENT_3D('',#55541,#44203,#44204);
#40490=AXIS2_PLACEMENT_3D('',#55542,#44205,#44206);
#40491=AXIS2_PLACEMENT_3D('',#55543,#44207,#44208);
#40492=AXIS2_PLACEMENT_3D('',#55545,#44209,#44210);
#40493=AXIS2_PLACEMENT_3D('',#55548,#44212,#44213);
#40494=AXIS2_PLACEMENT_3D('',#55549,#44214,#44215);
#40495=AXIS2_PLACEMENT_3D('',#55551,#44216,#44217);
#40496=AXIS2_PLACEMENT_3D('',#55554,#44219,#44220);
#40497=AXIS2_PLACEMENT_3D('',#55555,#44221,#44222);
#40498=AXIS2_PLACEMENT_3D('',#55557,#44223,#44224);
#40499=AXIS2_PLACEMENT_3D('',#55561,#44226,#44227);
#40500=AXIS2_PLACEMENT_3D('',#55565,#44229,#44230);
#40501=AXIS2_PLACEMENT_3D('',#55568,#44232,#44233);
#40502=AXIS2_PLACEMENT_3D('',#55572,#44235,#44236);
#40503=AXIS2_PLACEMENT_3D('',#55576,#44238,#44239);
#40504=AXIS2_PLACEMENT_3D('',#55578,#44241,#44242);
#40505=AXIS2_PLACEMENT_3D('',#55580,#44243,#44244);
#40506=AXIS2_PLACEMENT_3D('',#55584,#44246,#44247);
#40507=AXIS2_PLACEMENT_3D('',#55588,#44249,#44250);
#40508=AXIS2_PLACEMENT_3D('',#55591,#44252,#44253);
#40509=AXIS2_PLACEMENT_3D('',#55595,#44255,#44256);
#40510=AXIS2_PLACEMENT_3D('',#55599,#44258,#44259);
#40511=AXIS2_PLACEMENT_3D('',#55601,#44261,#44262);
#40512=AXIS2_PLACEMENT_3D('',#55604,#44265,#44266);
#40513=AXIS2_PLACEMENT_3D('',#55607,#44269,#44270);
#40514=AXIS2_PLACEMENT_3D('',#55608,#44271,#44272);
#40515=AXIS2_PLACEMENT_3D('',#55609,#44273,#44274);
#40516=AXIS2_PLACEMENT_3D('',#55610,#44275,#44276);
#40517=AXIS2_PLACEMENT_3D('',#55613,#44279,#44280);
#40518=AXIS2_PLACEMENT_3D('',#55616,#44283,#44284);
#40519=AXIS2_PLACEMENT_3D('',#55618,#44286,#44287);
#40520=AXIS2_PLACEMENT_3D('',#55620,#44289,#44290);
#40521=AXIS2_PLACEMENT_3D('',#55621,#44291,#44292);
#40522=AXIS2_PLACEMENT_3D('',#55622,#44293,#44294);
#40523=AXIS2_PLACEMENT_3D('',#55623,#44295,#44296);
#40524=AXIS2_PLACEMENT_3D('',#55624,#44297,#44298);
#40525=AXIS2_PLACEMENT_3D('',#55625,#44299,#44300);
#40526=AXIS2_PLACEMENT_3D('',#55626,#44301,#44302);
#40527=AXIS2_PLACEMENT_3D('',#55627,#44303,#44304);
#40528=AXIS2_PLACEMENT_3D('',#55628,#44305,#44306);
#40529=AXIS2_PLACEMENT_3D('',#55629,#44307,#44308);
#40530=AXIS2_PLACEMENT_3D('',#55631,#44309,#44310);
#40531=AXIS2_PLACEMENT_3D('',#55634,#44312,#44313);
#40532=AXIS2_PLACEMENT_3D('',#55635,#44314,#44315);
#40533=AXIS2_PLACEMENT_3D('',#55637,#44316,#44317);
#40534=AXIS2_PLACEMENT_3D('',#55640,#44319,#44320);
#40535=AXIS2_PLACEMENT_3D('',#55641,#44321,#44322);
#40536=AXIS2_PLACEMENT_3D('',#55643,#44323,#44324);
#40537=AXIS2_PLACEMENT_3D('',#55647,#44326,#44327);
#40538=AXIS2_PLACEMENT_3D('',#55651,#44329,#44330);
#40539=AXIS2_PLACEMENT_3D('',#55654,#44332,#44333);
#40540=AXIS2_PLACEMENT_3D('',#55658,#44335,#44336);
#40541=AXIS2_PLACEMENT_3D('',#55662,#44338,#44339);
#40542=AXIS2_PLACEMENT_3D('',#55664,#44341,#44342);
#40543=AXIS2_PLACEMENT_3D('',#55666,#44343,#44344);
#40544=AXIS2_PLACEMENT_3D('',#55670,#44346,#44347);
#40545=AXIS2_PLACEMENT_3D('',#55674,#44349,#44350);
#40546=AXIS2_PLACEMENT_3D('',#55677,#44352,#44353);
#40547=AXIS2_PLACEMENT_3D('',#55681,#44355,#44356);
#40548=AXIS2_PLACEMENT_3D('',#55685,#44358,#44359);
#40549=AXIS2_PLACEMENT_3D('',#55687,#44361,#44362);
#40550=AXIS2_PLACEMENT_3D('',#55690,#44365,#44366);
#40551=AXIS2_PLACEMENT_3D('',#55693,#44369,#44370);
#40552=AXIS2_PLACEMENT_3D('',#55694,#44371,#44372);
#40553=AXIS2_PLACEMENT_3D('',#55695,#44373,#44374);
#40554=AXIS2_PLACEMENT_3D('',#55696,#44375,#44376);
#40555=AXIS2_PLACEMENT_3D('',#55699,#44379,#44380);
#40556=AXIS2_PLACEMENT_3D('',#55702,#44383,#44384);
#40557=AXIS2_PLACEMENT_3D('',#55704,#44386,#44387);
#40558=AXIS2_PLACEMENT_3D('',#55706,#44389,#44390);
#40559=AXIS2_PLACEMENT_3D('',#55707,#44391,#44392);
#40560=AXIS2_PLACEMENT_3D('',#55708,#44393,#44394);
#40561=AXIS2_PLACEMENT_3D('',#55709,#44395,#44396);
#40562=AXIS2_PLACEMENT_3D('',#55710,#44397,#44398);
#40563=AXIS2_PLACEMENT_3D('',#55711,#44399,#44400);
#40564=AXIS2_PLACEMENT_3D('',#55712,#44401,#44402);
#40565=AXIS2_PLACEMENT_3D('',#55713,#44403,#44404);
#40566=AXIS2_PLACEMENT_3D('',#55714,#44405,#44406);
#40567=AXIS2_PLACEMENT_3D('',#55715,#44407,#44408);
#40568=AXIS2_PLACEMENT_3D('',#55717,#44409,#44410);
#40569=AXIS2_PLACEMENT_3D('',#55720,#44412,#44413);
#40570=AXIS2_PLACEMENT_3D('',#55721,#44414,#44415);
#40571=AXIS2_PLACEMENT_3D('',#55723,#44416,#44417);
#40572=AXIS2_PLACEMENT_3D('',#55726,#44419,#44420);
#40573=AXIS2_PLACEMENT_3D('',#55727,#44421,#44422);
#40574=AXIS2_PLACEMENT_3D('',#55729,#44423,#44424);
#40575=AXIS2_PLACEMENT_3D('',#55733,#44426,#44427);
#40576=AXIS2_PLACEMENT_3D('',#55737,#44429,#44430);
#40577=AXIS2_PLACEMENT_3D('',#55740,#44432,#44433);
#40578=AXIS2_PLACEMENT_3D('',#55744,#44435,#44436);
#40579=AXIS2_PLACEMENT_3D('',#55748,#44438,#44439);
#40580=AXIS2_PLACEMENT_3D('',#55750,#44441,#44442);
#40581=AXIS2_PLACEMENT_3D('',#55752,#44443,#44444);
#40582=AXIS2_PLACEMENT_3D('',#55756,#44446,#44447);
#40583=AXIS2_PLACEMENT_3D('',#55760,#44449,#44450);
#40584=AXIS2_PLACEMENT_3D('',#55763,#44452,#44453);
#40585=AXIS2_PLACEMENT_3D('',#55767,#44455,#44456);
#40586=AXIS2_PLACEMENT_3D('',#55771,#44458,#44459);
#40587=AXIS2_PLACEMENT_3D('',#55773,#44461,#44462);
#40588=AXIS2_PLACEMENT_3D('',#55776,#44465,#44466);
#40589=AXIS2_PLACEMENT_3D('',#55779,#44469,#44470);
#40590=AXIS2_PLACEMENT_3D('',#55780,#44471,#44472);
#40591=AXIS2_PLACEMENT_3D('',#55781,#44473,#44474);
#40592=AXIS2_PLACEMENT_3D('',#55782,#44475,#44476);
#40593=AXIS2_PLACEMENT_3D('',#55785,#44479,#44480);
#40594=AXIS2_PLACEMENT_3D('',#55788,#44483,#44484);
#40595=AXIS2_PLACEMENT_3D('',#55790,#44486,#44487);
#40596=AXIS2_PLACEMENT_3D('',#55792,#44489,#44490);
#40597=AXIS2_PLACEMENT_3D('',#55793,#44491,#44492);
#40598=AXIS2_PLACEMENT_3D('',#55794,#44493,#44494);
#40599=AXIS2_PLACEMENT_3D('',#55795,#44495,#44496);
#40600=AXIS2_PLACEMENT_3D('',#55796,#44497,#44498);
#40601=AXIS2_PLACEMENT_3D('',#55797,#44499,#44500);
#40602=AXIS2_PLACEMENT_3D('',#55798,#44501,#44502);
#40603=AXIS2_PLACEMENT_3D('',#55799,#44503,#44504);
#40604=AXIS2_PLACEMENT_3D('',#55800,#44505,#44506);
#40605=AXIS2_PLACEMENT_3D('',#55801,#44507,#44508);
#40606=AXIS2_PLACEMENT_3D('',#55803,#44509,#44510);
#40607=AXIS2_PLACEMENT_3D('',#55806,#44512,#44513);
#40608=AXIS2_PLACEMENT_3D('',#55807,#44514,#44515);
#40609=AXIS2_PLACEMENT_3D('',#55809,#44516,#44517);
#40610=AXIS2_PLACEMENT_3D('',#55812,#44519,#44520);
#40611=AXIS2_PLACEMENT_3D('',#55813,#44521,#44522);
#40612=AXIS2_PLACEMENT_3D('',#55815,#44523,#44524);
#40613=AXIS2_PLACEMENT_3D('',#55819,#44526,#44527);
#40614=AXIS2_PLACEMENT_3D('',#55823,#44529,#44530);
#40615=AXIS2_PLACEMENT_3D('',#55826,#44532,#44533);
#40616=AXIS2_PLACEMENT_3D('',#55830,#44535,#44536);
#40617=AXIS2_PLACEMENT_3D('',#55834,#44538,#44539);
#40618=AXIS2_PLACEMENT_3D('',#55836,#44541,#44542);
#40619=AXIS2_PLACEMENT_3D('',#55838,#44543,#44544);
#40620=AXIS2_PLACEMENT_3D('',#55842,#44546,#44547);
#40621=AXIS2_PLACEMENT_3D('',#55846,#44549,#44550);
#40622=AXIS2_PLACEMENT_3D('',#55849,#44552,#44553);
#40623=AXIS2_PLACEMENT_3D('',#55853,#44555,#44556);
#40624=AXIS2_PLACEMENT_3D('',#55857,#44558,#44559);
#40625=AXIS2_PLACEMENT_3D('',#55859,#44561,#44562);
#40626=AXIS2_PLACEMENT_3D('',#55862,#44565,#44566);
#40627=AXIS2_PLACEMENT_3D('',#55865,#44569,#44570);
#40628=AXIS2_PLACEMENT_3D('',#55866,#44571,#44572);
#40629=AXIS2_PLACEMENT_3D('',#55867,#44573,#44574);
#40630=AXIS2_PLACEMENT_3D('',#55868,#44575,#44576);
#40631=AXIS2_PLACEMENT_3D('',#55871,#44579,#44580);
#40632=AXIS2_PLACEMENT_3D('',#55874,#44583,#44584);
#40633=AXIS2_PLACEMENT_3D('',#55876,#44586,#44587);
#40634=AXIS2_PLACEMENT_3D('',#55878,#44589,#44590);
#40635=AXIS2_PLACEMENT_3D('',#55879,#44591,#44592);
#40636=AXIS2_PLACEMENT_3D('',#55880,#44593,#44594);
#40637=AXIS2_PLACEMENT_3D('',#55881,#44595,#44596);
#40638=AXIS2_PLACEMENT_3D('',#55887,#44597,#44598);
#40639=AXIS2_PLACEMENT_3D('',#55897,#44599,#44600);
#40640=AXIS2_PLACEMENT_3D('',#55900,#44602,#44603);
#40641=AXIS2_PLACEMENT_3D('',#55912,#44604,#44605);
#40642=AXIS2_PLACEMENT_3D('',#55922,#44607,#44608);
#40643=AXIS2_PLACEMENT_3D('',#55925,#44610,#44611);
#40644=AXIS2_PLACEMENT_3D('',#55937,#44612,#44613);
#40645=AXIS2_PLACEMENT_3D('',#55941,#44615,#44616);
#40646=AXIS2_PLACEMENT_3D('',#55950,#44618,#44619);
#40647=AXIS2_PLACEMENT_3D('',#55960,#44620,#44621);
#40648=AXIS2_PLACEMENT_3D('',#55964,#44623,#44624);
#40649=AXIS2_PLACEMENT_3D('',#55974,#44625,#44626);
#40650=AXIS2_PLACEMENT_3D('',#55986,#44628,#44629);
#40651=AXIS2_PLACEMENT_3D('',#55990,#44631,#44632);
#40652=AXIS2_PLACEMENT_3D('',#55999,#44633,#44634);
#40653=AXIS2_PLACEMENT_3D('',#56013,#44637,#44638);
#40654=AXIS2_PLACEMENT_3D('',#56022,#44639,#44640);
#40655=AXIS2_PLACEMENT_3D('',#56025,#44642,#44643);
#40656=AXIS2_PLACEMENT_3D('',#56032,#44644,#44645);
#40657=AXIS2_PLACEMENT_3D('',#56039,#44646,#44647);
#40658=AXIS2_PLACEMENT_3D('',#56040,#44648,#44649);
#40659=AXIS2_PLACEMENT_3D('',#56051,#44650,#44651);
#40660=AXIS2_PLACEMENT_3D('',#56061,#44652,#44653);
#40661=AXIS2_PLACEMENT_3D('',#56062,#44654,#44655);
#40662=AXIS2_PLACEMENT_3D('',#56073,#44656,#44657);
#40663=AXIS2_PLACEMENT_3D('',#56075,#44658,#44659);
#40664=AXIS2_PLACEMENT_3D('',#56084,#44660,#44661);
#40665=AXIS2_PLACEMENT_3D('',#56095,#44662,#44663);
#40666=AXIS2_PLACEMENT_3D('',#56097,#44664,#44665);
#40667=AXIS2_PLACEMENT_3D('',#56106,#44666,#44667);
#40668=AXIS2_PLACEMENT_3D('',#56116,#44668,#44669);
#40669=AXIS2_PLACEMENT_3D('',#56118,#44670,#44671);
#40670=AXIS2_PLACEMENT_3D('',#56128,#44672,#44673);
#40671=AXIS2_PLACEMENT_3D('',#56139,#44674,#44675);
#40672=AXIS2_PLACEMENT_3D('',#56149,#44676,#44677);
#40673=AXIS2_PLACEMENT_3D('',#56150,#44678,#44679);
#40674=AXIS2_PLACEMENT_3D('',#56151,#44680,#44681);
#40675=AXIS2_PLACEMENT_3D('',#56159,#44682,#44683);
#40676=AXIS2_PLACEMENT_3D('',#56160,#44684,#44685);
#40677=AXIS2_PLACEMENT_3D('',#56161,#44686,#44687);
#40678=AXIS2_PLACEMENT_3D('',#56171,#44688,#44689);
#40679=AXIS2_PLACEMENT_3D('',#56172,#44690,#44691);
#40680=AXIS2_PLACEMENT_3D('',#56188,#44692,#44693);
#40681=AXIS2_PLACEMENT_3D('',#56190,#44694,#44695);
#40682=AXIS2_PLACEMENT_3D('',#56199,#44696,#44697);
#40683=AXIS2_PLACEMENT_3D('',#56200,#44698,#44699);
#40684=AXIS2_PLACEMENT_3D('',#56202,#44700,#44701);
#40685=AXIS2_PLACEMENT_3D('',#56213,#44702,#44703);
#40686=AXIS2_PLACEMENT_3D('',#56214,#44704,#44705);
#40687=AXIS2_PLACEMENT_3D('',#56216,#44706,#44707);
#40688=AXIS2_PLACEMENT_3D('',#56226,#44708,#44709);
#40689=AXIS2_PLACEMENT_3D('',#56228,#44710,#44711);
#40690=AXIS2_PLACEMENT_3D('',#56238,#44712,#44713);
#40691=AXIS2_PLACEMENT_3D('',#56239,#44714,#44715);
#40692=AXIS2_PLACEMENT_3D('',#56268,#44718,#44719);
#40693=AXIS2_PLACEMENT_3D('',#56270,#44721,#44722);
#40694=AXIS2_PLACEMENT_3D('',#56273,#44725,#44726);
#40695=AXIS2_PLACEMENT_3D('',#56275,#44728,#44729);
#40696=AXIS2_PLACEMENT_3D('',#56278,#44732,#44733);
#40697=AXIS2_PLACEMENT_3D('',#56280,#44735,#44736);
#40698=AXIS2_PLACEMENT_3D('',#56282,#44738,#44739);
#40699=AXIS2_PLACEMENT_3D('',#56285,#44742,#44743);
#40700=AXIS2_PLACEMENT_3D('',#56288,#44746,#44747);
#40701=AXIS2_PLACEMENT_3D('',#56290,#44749,#44750);
#40702=AXIS2_PLACEMENT_3D('',#56293,#44753,#44754);
#40703=AXIS2_PLACEMENT_3D('',#56773,#44798,#44799);
#40704=AXIS2_PLACEMENT_3D('',#56774,#44800,#44801);
#40705=AXIS2_PLACEMENT_3D('',#56775,#44802,#44803);
#40706=AXIS2_PLACEMENT_3D('',#56776,#44804,#44805);
#40707=AXIS2_PLACEMENT_3D('',#56777,#44806,#44807);
#40708=AXIS2_PLACEMENT_3D('',#56778,#44808,#44809);
#40709=AXIS2_PLACEMENT_3D('',#56779,#44810,#44811);
#40710=AXIS2_PLACEMENT_3D('',#56780,#44812,#44813);
#40711=AXIS2_PLACEMENT_3D('',#56781,#44814,#44815);
#40712=AXIS2_PLACEMENT_3D('',#56782,#44816,#44817);
#40713=AXIS2_PLACEMENT_3D('',#56783,#44818,#44819);
#40714=AXIS2_PLACEMENT_3D('',#56784,#44820,#44821);
#40715=AXIS2_PLACEMENT_3D('',#56785,#44822,#44823);
#40716=AXIS2_PLACEMENT_3D('',#56786,#44824,#44825);
#40717=AXIS2_PLACEMENT_3D('',#56787,#44826,#44827);
#40718=AXIS2_PLACEMENT_3D('',#56788,#44828,#44829);
#40719=AXIS2_PLACEMENT_3D('',#56789,#44830,#44831);
#40720=AXIS2_PLACEMENT_3D('',#56790,#44832,#44833);
#40721=AXIS2_PLACEMENT_3D('',#56791,#44834,#44835);
#40722=AXIS2_PLACEMENT_3D('',#56792,#44836,#44837);
#40723=AXIS2_PLACEMENT_3D('',#56793,#44838,#44839);
#40724=AXIS2_PLACEMENT_3D('',#56794,#44840,#44841);
#40725=AXIS2_PLACEMENT_3D('',#56795,#44842,#44843);
#40726=AXIS2_PLACEMENT_3D('',#56796,#44844,#44845);
#40727=AXIS2_PLACEMENT_3D('',#56797,#44846,#44847);
#40728=AXIS2_PLACEMENT_3D('',#56798,#44848,#44849);
#40729=AXIS2_PLACEMENT_3D('',#56799,#44850,#44851);
#40730=AXIS2_PLACEMENT_3D('',#56800,#44852,#44853);
#40731=AXIS2_PLACEMENT_3D('',#56801,#44854,#44855);
#40732=AXIS2_PLACEMENT_3D('',#56802,#44856,#44857);
#40733=AXIS2_PLACEMENT_3D('',#56803,#44858,#44859);
#40734=AXIS2_PLACEMENT_3D('',#56804,#44860,#44861);
#40735=AXIS2_PLACEMENT_3D('',#56805,#44862,#44863);
#40736=AXIS2_PLACEMENT_3D('',#56806,#44864,#44865);
#40737=AXIS2_PLACEMENT_3D('',#56807,#44866,#44867);
#40738=AXIS2_PLACEMENT_3D('',#56808,#44868,#44869);
#40739=AXIS2_PLACEMENT_3D('',#56809,#44870,#44871);
#40740=AXIS2_PLACEMENT_3D('',#56810,#44872,#44873);
#40741=AXIS2_PLACEMENT_3D('',#56811,#44874,#44875);
#40742=AXIS2_PLACEMENT_3D('',#56812,#44876,#44877);
#40743=AXIS2_PLACEMENT_3D('',#56813,#44878,#44879);
#40744=AXIS2_PLACEMENT_3D('',#56814,#44880,#44881);
#40745=AXIS2_PLACEMENT_3D('',#56815,#44882,#44883);
#40746=AXIS2_PLACEMENT_3D('',#56816,#44884,#44885);
#40747=AXIS2_PLACEMENT_3D('',#56817,#44886,#44887);
#40748=AXIS2_PLACEMENT_3D('',#56818,#44888,#44889);
#40749=AXIS2_PLACEMENT_3D('',#56819,#44890,#44891);
#40750=AXIS2_PLACEMENT_3D('',#56820,#44892,#44893);
#40751=AXIS2_PLACEMENT_3D('',#56821,#44894,#44895);
#40752=AXIS2_PLACEMENT_3D('',#56822,#44896,#44897);
#40753=AXIS2_PLACEMENT_3D('',#56823,#44898,#44899);
#40754=AXIS2_PLACEMENT_3D('',#56824,#44900,#44901);
#40755=AXIS2_PLACEMENT_3D('',#56825,#44902,#44903);
#40756=AXIS2_PLACEMENT_3D('',#56826,#44904,#44905);
#40757=AXIS2_PLACEMENT_3D('',#56827,#44906,#44907);
#40758=AXIS2_PLACEMENT_3D('',#56830,#44910,#44911);
#40759=AXIS2_PLACEMENT_3D('',#56832,#44913,#44914);
#40760=AXIS2_PLACEMENT_3D('',#56834,#44916,#44917);
#40761=AXIS2_PLACEMENT_3D('',#56836,#44919,#44920);
#40762=AXIS2_PLACEMENT_3D('',#56838,#44922,#44923);
#40763=AXIS2_PLACEMENT_3D('',#56840,#44925,#44926);
#40764=AXIS2_PLACEMENT_3D('',#56842,#44928,#44929);
#40765=AXIS2_PLACEMENT_3D('',#56844,#44931,#44932);
#40766=AXIS2_PLACEMENT_3D('',#56846,#44934,#44935);
#40767=AXIS2_PLACEMENT_3D('',#56848,#44937,#44938);
#40768=AXIS2_PLACEMENT_3D('',#56850,#44940,#44941);
#40769=AXIS2_PLACEMENT_3D('',#56851,#44942,#44943);
#40770=AXIS2_PLACEMENT_3D('',#56854,#44946,#44947);
#40771=AXIS2_PLACEMENT_3D('',#56856,#44949,#44950);
#40772=AXIS2_PLACEMENT_3D('',#56858,#44952,#44953);
#40773=AXIS2_PLACEMENT_3D('',#56859,#44954,#44955);
#40774=AXIS2_PLACEMENT_3D('',#56860,#44956,#44957);
#40775=AXIS2_PLACEMENT_3D('',#56861,#44958,#44959);
#40776=AXIS2_PLACEMENT_3D('',#56862,#44960,#44961);
#40777=AXIS2_PLACEMENT_3D('',#56863,#44962,#44963);
#40778=AXIS2_PLACEMENT_3D('',#56865,#44965,#44966);
#40779=AXIS2_PLACEMENT_3D('',#56867,#44968,#44969);
#40780=AXIS2_PLACEMENT_3D('',#56868,#44970,#44971);
#40781=AXIS2_PLACEMENT_3D('',#56870,#44973,#44974);
#40782=AXIS2_PLACEMENT_3D('',#56872,#44976,#44977);
#40783=AXIS2_PLACEMENT_3D('',#56873,#44978,#44979);
#40784=AXIS2_PLACEMENT_3D('',#56875,#44981,#44982);
#40785=AXIS2_PLACEMENT_3D('',#56877,#44984,#44985);
#40786=AXIS2_PLACEMENT_3D('',#56878,#44986,#44987);
#40787=AXIS2_PLACEMENT_3D('',#56880,#44989,#44990);
#40788=AXIS2_PLACEMENT_3D('',#56882,#44992,#44993);
#40789=AXIS2_PLACEMENT_3D('',#56883,#44994,#44995);
#40790=AXIS2_PLACEMENT_3D('',#56885,#44997,#44998);
#40791=AXIS2_PLACEMENT_3D('',#56887,#45000,#45001);
#40792=AXIS2_PLACEMENT_3D('',#56888,#45002,#45003);
#40793=AXIS2_PLACEMENT_3D('',#56890,#45005,#45006);
#40794=AXIS2_PLACEMENT_3D('',#56892,#45008,#45009);
#40795=AXIS2_PLACEMENT_3D('',#56893,#45010,#45011);
#40796=AXIS2_PLACEMENT_3D('',#56895,#45013,#45014);
#40797=AXIS2_PLACEMENT_3D('',#56897,#45016,#45017);
#40798=AXIS2_PLACEMENT_3D('',#56898,#45018,#45019);
#40799=AXIS2_PLACEMENT_3D('',#56900,#45021,#45022);
#40800=AXIS2_PLACEMENT_3D('',#56902,#45024,#45025);
#40801=AXIS2_PLACEMENT_3D('',#56903,#45026,#45027);
#40802=AXIS2_PLACEMENT_3D('',#56905,#45029,#45030);
#40803=AXIS2_PLACEMENT_3D('',#56907,#45032,#45033);
#40804=AXIS2_PLACEMENT_3D('',#56908,#45034,#45035);
#40805=AXIS2_PLACEMENT_3D('',#56910,#45037,#45038);
#40806=AXIS2_PLACEMENT_3D('',#56912,#45040,#45041);
#40807=AXIS2_PLACEMENT_3D('',#56913,#45042,#45043);
#40808=AXIS2_PLACEMENT_3D('',#56915,#45045,#45046);
#40809=AXIS2_PLACEMENT_3D('',#56917,#45048,#45049);
#40810=AXIS2_PLACEMENT_3D('',#56918,#45050,#45051);
#40811=AXIS2_PLACEMENT_3D('',#56920,#45053,#45054);
#40812=AXIS2_PLACEMENT_3D('',#56922,#45056,#45057);
#40813=AXIS2_PLACEMENT_3D('',#56923,#45058,#45059);
#40814=AXIS2_PLACEMENT_3D('',#56925,#45061,#45062);
#40815=AXIS2_PLACEMENT_3D('',#56927,#45064,#45065);
#40816=AXIS2_PLACEMENT_3D('',#56928,#45066,#45067);
#40817=AXIS2_PLACEMENT_3D('',#56930,#45069,#45070);
#40818=AXIS2_PLACEMENT_3D('',#56932,#45072,#45073);
#40819=AXIS2_PLACEMENT_3D('',#56933,#45074,#45075);
#40820=AXIS2_PLACEMENT_3D('',#56935,#45077,#45078);
#40821=AXIS2_PLACEMENT_3D('',#56937,#45080,#45081);
#40822=AXIS2_PLACEMENT_3D('',#56938,#45082,#45083);
#40823=AXIS2_PLACEMENT_3D('',#56940,#45085,#45086);
#40824=AXIS2_PLACEMENT_3D('',#56942,#45088,#45089);
#40825=AXIS2_PLACEMENT_3D('',#56943,#45090,#45091);
#40826=AXIS2_PLACEMENT_3D('',#56945,#45093,#45094);
#40827=AXIS2_PLACEMENT_3D('',#56947,#45096,#45097);
#40828=AXIS2_PLACEMENT_3D('',#56948,#45098,#45099);
#40829=AXIS2_PLACEMENT_3D('',#56950,#45101,#45102);
#40830=AXIS2_PLACEMENT_3D('',#56952,#45104,#45105);
#40831=AXIS2_PLACEMENT_3D('',#56953,#45106,#45107);
#40832=AXIS2_PLACEMENT_3D('',#56955,#45109,#45110);
#40833=AXIS2_PLACEMENT_3D('',#56957,#45112,#45113);
#40834=AXIS2_PLACEMENT_3D('',#56958,#45114,#45115);
#40835=AXIS2_PLACEMENT_3D('',#56960,#45117,#45118);
#40836=AXIS2_PLACEMENT_3D('',#56962,#45120,#45121);
#40837=AXIS2_PLACEMENT_3D('',#56963,#45122,#45123);
#40838=AXIS2_PLACEMENT_3D('',#56965,#45125,#45126);
#40839=AXIS2_PLACEMENT_3D('',#56967,#45128,#45129);
#40840=AXIS2_PLACEMENT_3D('',#56968,#45130,#45131);
#40841=AXIS2_PLACEMENT_3D('',#56970,#45133,#45134);
#40842=AXIS2_PLACEMENT_3D('',#56972,#45136,#45137);
#40843=AXIS2_PLACEMENT_3D('',#56973,#45138,#45139);
#40844=AXIS2_PLACEMENT_3D('',#56975,#45141,#45142);
#40845=AXIS2_PLACEMENT_3D('',#56977,#45144,#45145);
#40846=AXIS2_PLACEMENT_3D('',#56978,#45146,#45147);
#40847=AXIS2_PLACEMENT_3D('',#56980,#45149,#45150);
#40848=AXIS2_PLACEMENT_3D('',#56982,#45152,#45153);
#40849=AXIS2_PLACEMENT_3D('',#56983,#45154,#45155);
#40850=AXIS2_PLACEMENT_3D('',#56985,#45157,#45158);
#40851=AXIS2_PLACEMENT_3D('',#56987,#45160,#45161);
#40852=AXIS2_PLACEMENT_3D('',#56988,#45162,#45163);
#40853=AXIS2_PLACEMENT_3D('',#56990,#45165,#45166);
#40854=AXIS2_PLACEMENT_3D('',#56992,#45168,#45169);
#40855=AXIS2_PLACEMENT_3D('',#56993,#45170,#45171);
#40856=AXIS2_PLACEMENT_3D('',#56995,#45173,#45174);
#40857=AXIS2_PLACEMENT_3D('',#56997,#45176,#45177);
#40858=AXIS2_PLACEMENT_3D('',#56998,#45178,#45179);
#40859=AXIS2_PLACEMENT_3D('',#57000,#45181,#45182);
#40860=AXIS2_PLACEMENT_3D('',#57002,#45184,#45185);
#40861=AXIS2_PLACEMENT_3D('',#57003,#45186,#45187);
#40862=AXIS2_PLACEMENT_3D('',#57005,#45189,#45190);
#40863=AXIS2_PLACEMENT_3D('',#57007,#45192,#45193);
#40864=AXIS2_PLACEMENT_3D('',#57008,#45194,#45195);
#40865=AXIS2_PLACEMENT_3D('',#57010,#45197,#45198);
#40866=AXIS2_PLACEMENT_3D('',#57012,#45200,#45201);
#40867=AXIS2_PLACEMENT_3D('',#57013,#45202,#45203);
#40868=AXIS2_PLACEMENT_3D('',#57015,#45205,#45206);
#40869=AXIS2_PLACEMENT_3D('',#57017,#45208,#45209);
#40870=AXIS2_PLACEMENT_3D('',#57018,#45210,#45211);
#40871=AXIS2_PLACEMENT_3D('',#57020,#45213,#45214);
#40872=AXIS2_PLACEMENT_3D('',#57022,#45216,#45217);
#40873=AXIS2_PLACEMENT_3D('',#57023,#45218,#45219);
#40874=AXIS2_PLACEMENT_3D('',#57025,#45221,#45222);
#40875=AXIS2_PLACEMENT_3D('',#57027,#45224,#45225);
#40876=AXIS2_PLACEMENT_3D('',#57028,#45226,#45227);
#40877=AXIS2_PLACEMENT_3D('',#57030,#45229,#45230);
#40878=AXIS2_PLACEMENT_3D('',#57032,#45232,#45233);
#40879=AXIS2_PLACEMENT_3D('',#57033,#45234,#45235);
#40880=AXIS2_PLACEMENT_3D('',#57035,#45237,#45238);
#40881=AXIS2_PLACEMENT_3D('',#57037,#45240,#45241);
#40882=AXIS2_PLACEMENT_3D('',#57038,#45242,#45243);
#40883=AXIS2_PLACEMENT_3D('',#57040,#45245,#45246);
#40884=AXIS2_PLACEMENT_3D('',#57042,#45248,#45249);
#40885=AXIS2_PLACEMENT_3D('',#57043,#45250,#45251);
#40886=AXIS2_PLACEMENT_3D('',#57045,#45253,#45254);
#40887=AXIS2_PLACEMENT_3D('',#57047,#45256,#45257);
#40888=AXIS2_PLACEMENT_3D('',#57048,#45258,#45259);
#40889=AXIS2_PLACEMENT_3D('',#57050,#45261,#45262);
#40890=AXIS2_PLACEMENT_3D('',#57052,#45264,#45265);
#40891=AXIS2_PLACEMENT_3D('',#57053,#45266,#45267);
#40892=AXIS2_PLACEMENT_3D('',#57055,#45269,#45270);
#40893=AXIS2_PLACEMENT_3D('',#57057,#45272,#45273);
#40894=AXIS2_PLACEMENT_3D('',#57058,#45274,#45275);
#40895=AXIS2_PLACEMENT_3D('',#57060,#45277,#45278);
#40896=AXIS2_PLACEMENT_3D('',#57062,#45280,#45281);
#40897=AXIS2_PLACEMENT_3D('',#57063,#45282,#45283);
#40898=AXIS2_PLACEMENT_3D('',#57065,#45285,#45286);
#40899=AXIS2_PLACEMENT_3D('',#57067,#45288,#45289);
#40900=AXIS2_PLACEMENT_3D('',#57068,#45290,#45291);
#40901=AXIS2_PLACEMENT_3D('',#57070,#45293,#45294);
#40902=AXIS2_PLACEMENT_3D('',#57072,#45296,#45297);
#40903=AXIS2_PLACEMENT_3D('',#57073,#45298,#45299);
#40904=AXIS2_PLACEMENT_3D('',#57075,#45301,#45302);
#40905=AXIS2_PLACEMENT_3D('',#57077,#45304,#45305);
#40906=AXIS2_PLACEMENT_3D('',#57078,#45306,#45307);
#40907=AXIS2_PLACEMENT_3D('',#57080,#45309,#45310);
#40908=AXIS2_PLACEMENT_3D('',#57082,#45312,#45313);
#40909=AXIS2_PLACEMENT_3D('',#57083,#45314,#45315);
#40910=AXIS2_PLACEMENT_3D('',#57085,#45317,#45318);
#40911=AXIS2_PLACEMENT_3D('',#57087,#45320,#45321);
#40912=AXIS2_PLACEMENT_3D('',#57088,#45322,#45323);
#40913=AXIS2_PLACEMENT_3D('',#57090,#45325,#45326);
#40914=AXIS2_PLACEMENT_3D('',#57092,#45328,#45329);
#40915=AXIS2_PLACEMENT_3D('',#57093,#45330,#45331);
#40916=AXIS2_PLACEMENT_3D('',#57095,#45333,#45334);
#40917=AXIS2_PLACEMENT_3D('',#57097,#45336,#45337);
#40918=AXIS2_PLACEMENT_3D('',#57098,#45338,#45339);
#40919=AXIS2_PLACEMENT_3D('',#57100,#45341,#45342);
#40920=AXIS2_PLACEMENT_3D('',#57102,#45344,#45345);
#40921=AXIS2_PLACEMENT_3D('',#57103,#45346,#45347);
#40922=AXIS2_PLACEMENT_3D('',#57105,#45349,#45350);
#40923=AXIS2_PLACEMENT_3D('',#57107,#45352,#45353);
#40924=AXIS2_PLACEMENT_3D('',#57109,#45355,#45356);
#40925=AXIS2_PLACEMENT_3D('',#57112,#45359,#45360);
#40926=AXIS2_PLACEMENT_3D('',#57114,#45362,#45363);
#40927=AXIS2_PLACEMENT_3D('',#57115,#45364,#45365);
#40928=AXIS2_PLACEMENT_3D('',#57117,#45367,#45368);
#40929=AXIS2_PLACEMENT_3D('',#57118,#45369,#45370);
#40930=AXIS2_PLACEMENT_3D('',#57119,#45371,#45372);
#40931=AXIS2_PLACEMENT_3D('',#57120,#45373,#45374);
#40932=AXIS2_PLACEMENT_3D('',#57122,#45376,#45377);
#40933=AXIS2_PLACEMENT_3D('',#57123,#45378,#45379);
#40934=AXIS2_PLACEMENT_3D('',#57124,#45380,#45381);
#40935=AXIS2_PLACEMENT_3D('',#57125,#45382,#45383);
#40936=AXIS2_PLACEMENT_3D('',#57127,#45385,#45386);
#40937=AXIS2_PLACEMENT_3D('',#57129,#45388,#45389);
#40938=AXIS2_PLACEMENT_3D('',#57131,#45391,#45392);
#40939=AXIS2_PLACEMENT_3D('',#57133,#45394,#45395);
#40940=AXIS2_PLACEMENT_3D('',#57134,#45396,#45397);
#40941=AXIS2_PLACEMENT_3D('',#57135,#45398,#45399);
#40942=AXIS2_PLACEMENT_3D('',#57136,#45400,#45401);
#40943=AXIS2_PLACEMENT_3D('',#57137,#45402,#45403);
#40944=AXIS2_PLACEMENT_3D('',#57138,#45404,#45405);
#40945=AXIS2_PLACEMENT_3D('',#57139,#45406,#45407);
#40946=AXIS2_PLACEMENT_3D('',#57140,#45408,#45409);
#40947=AXIS2_PLACEMENT_3D('',#57142,#45410,#45411);
#40948=AXIS2_PLACEMENT_3D('',#57145,#45413,#45414);
#40949=AXIS2_PLACEMENT_3D('',#57146,#45415,#45416);
#40950=AXIS2_PLACEMENT_3D('',#57148,#45417,#45418);
#40951=AXIS2_PLACEMENT_3D('',#57151,#45420,#45421);
#40952=AXIS2_PLACEMENT_3D('',#57152,#45422,#45423);
#40953=AXIS2_PLACEMENT_3D('',#57154,#45424,#45425);
#40954=AXIS2_PLACEMENT_3D('',#57158,#45427,#45428);
#40955=AXIS2_PLACEMENT_3D('',#57162,#45430,#45431);
#40956=AXIS2_PLACEMENT_3D('',#57165,#45433,#45434);
#40957=AXIS2_PLACEMENT_3D('',#57169,#45436,#45437);
#40958=AXIS2_PLACEMENT_3D('',#57173,#45439,#45440);
#40959=AXIS2_PLACEMENT_3D('',#57175,#45442,#45443);
#40960=AXIS2_PLACEMENT_3D('',#57177,#45444,#45445);
#40961=AXIS2_PLACEMENT_3D('',#57181,#45447,#45448);
#40962=AXIS2_PLACEMENT_3D('',#57185,#45450,#45451);
#40963=AXIS2_PLACEMENT_3D('',#57188,#45453,#45454);
#40964=AXIS2_PLACEMENT_3D('',#57192,#45456,#45457);
#40965=AXIS2_PLACEMENT_3D('',#57196,#45459,#45460);
#40966=AXIS2_PLACEMENT_3D('',#57198,#45462,#45463);
#40967=AXIS2_PLACEMENT_3D('',#57201,#45466,#45467);
#40968=AXIS2_PLACEMENT_3D('',#57204,#45470,#45471);
#40969=AXIS2_PLACEMENT_3D('',#57205,#45472,#45473);
#40970=AXIS2_PLACEMENT_3D('',#57206,#45474,#45475);
#40971=AXIS2_PLACEMENT_3D('',#57207,#45476,#45477);
#40972=AXIS2_PLACEMENT_3D('',#57210,#45480,#45481);
#40973=AXIS2_PLACEMENT_3D('',#57213,#45484,#45485);
#40974=AXIS2_PLACEMENT_3D('',#57215,#45487,#45488);
#40975=AXIS2_PLACEMENT_3D('',#57217,#45490,#45491);
#40976=AXIS2_PLACEMENT_3D('',#57218,#45492,#45493);
#40977=AXIS2_PLACEMENT_3D('',#57219,#45494,#45495);
#40978=AXIS2_PLACEMENT_3D('',#57220,#45496,#45497);
#40979=AXIS2_PLACEMENT_3D('',#57221,#45498,#45499);
#40980=AXIS2_PLACEMENT_3D('',#57222,#45500,#45501);
#40981=AXIS2_PLACEMENT_3D('',#57223,#45502,#45503);
#40982=AXIS2_PLACEMENT_3D('',#57224,#45504,#45505);
#40983=AXIS2_PLACEMENT_3D('',#57225,#45506,#45507);
#40984=AXIS2_PLACEMENT_3D('',#57226,#45508,#45509);
#40985=AXIS2_PLACEMENT_3D('',#57228,#45510,#45511);
#40986=AXIS2_PLACEMENT_3D('',#57231,#45513,#45514);
#40987=AXIS2_PLACEMENT_3D('',#57232,#45515,#45516);
#40988=AXIS2_PLACEMENT_3D('',#57234,#45517,#45518);
#40989=AXIS2_PLACEMENT_3D('',#57237,#45520,#45521);
#40990=AXIS2_PLACEMENT_3D('',#57238,#45522,#45523);
#40991=AXIS2_PLACEMENT_3D('',#57240,#45524,#45525);
#40992=AXIS2_PLACEMENT_3D('',#57244,#45527,#45528);
#40993=AXIS2_PLACEMENT_3D('',#57248,#45530,#45531);
#40994=AXIS2_PLACEMENT_3D('',#57251,#45533,#45534);
#40995=AXIS2_PLACEMENT_3D('',#57255,#45536,#45537);
#40996=AXIS2_PLACEMENT_3D('',#57259,#45539,#45540);
#40997=AXIS2_PLACEMENT_3D('',#57261,#45542,#45543);
#40998=AXIS2_PLACEMENT_3D('',#57263,#45544,#45545);
#40999=AXIS2_PLACEMENT_3D('',#57267,#45547,#45548);
#41000=AXIS2_PLACEMENT_3D('',#57271,#45550,#45551);
#41001=AXIS2_PLACEMENT_3D('',#57274,#45553,#45554);
#41002=AXIS2_PLACEMENT_3D('',#57278,#45556,#45557);
#41003=AXIS2_PLACEMENT_3D('',#57282,#45559,#45560);
#41004=AXIS2_PLACEMENT_3D('',#57284,#45562,#45563);
#41005=AXIS2_PLACEMENT_3D('',#57287,#45566,#45567);
#41006=AXIS2_PLACEMENT_3D('',#57290,#45570,#45571);
#41007=AXIS2_PLACEMENT_3D('',#57291,#45572,#45573);
#41008=AXIS2_PLACEMENT_3D('',#57292,#45574,#45575);
#41009=AXIS2_PLACEMENT_3D('',#57293,#45576,#45577);
#41010=AXIS2_PLACEMENT_3D('',#57296,#45580,#45581);
#41011=AXIS2_PLACEMENT_3D('',#57299,#45584,#45585);
#41012=AXIS2_PLACEMENT_3D('',#57301,#45587,#45588);
#41013=AXIS2_PLACEMENT_3D('',#57303,#45590,#45591);
#41014=AXIS2_PLACEMENT_3D('',#57304,#45592,#45593);
#41015=AXIS2_PLACEMENT_3D('',#57305,#45594,#45595);
#41016=AXIS2_PLACEMENT_3D('',#57306,#45596,#45597);
#41017=AXIS2_PLACEMENT_3D('',#57308,#45599,#45600);
#41018=AXIS2_PLACEMENT_3D('',#57310,#45602,#45603);
#41019=AXIS2_PLACEMENT_3D('',#57312,#45605,#45606);
#41020=AXIS2_PLACEMENT_3D('',#57315,#45609,#45610);
#41021=AXIS2_PLACEMENT_3D('',#57317,#45612,#45613);
#41022=AXIS2_PLACEMENT_3D('',#57318,#45614,#45615);
#41023=AXIS2_PLACEMENT_3D('',#57322,#45617,#45618);
#41024=AXIS2_PLACEMENT_3D('',#57323,#45619,#45620);
#41025=AXIS2_PLACEMENT_3D('',#57324,#45621,#45622);
#41026=AXIS2_PLACEMENT_3D('',#57326,#45623,#45624);
#41027=AXIS2_PLACEMENT_3D('',#57329,#45626,#45627);
#41028=AXIS2_PLACEMENT_3D('',#57330,#45628,#45629);
#41029=AXIS2_PLACEMENT_3D('',#57332,#45631,#45632);
#41030=AXIS2_PLACEMENT_3D('',#57334,#45634,#45635);
#41031=AXIS2_PLACEMENT_3D('',#57340,#45639,#45640);
#41032=AXIS2_PLACEMENT_3D('',#57346,#45644,#45645);
#41033=AXIS2_PLACEMENT_3D('',#57348,#45646,#45647);
#41034=AXIS2_PLACEMENT_3D('',#57351,#45649,#45650);
#41035=AXIS2_PLACEMENT_3D('',#57352,#45651,#45652);
#41036=AXIS2_PLACEMENT_3D('',#57354,#45653,#45654);
#41037=AXIS2_PLACEMENT_3D('',#57357,#45656,#45657);
#41038=AXIS2_PLACEMENT_3D('',#57358,#45658,#45659);
#41039=AXIS2_PLACEMENT_3D('',#57360,#45661,#45662);
#41040=AXIS2_PLACEMENT_3D('',#57362,#45664,#45665);
#41041=AXIS2_PLACEMENT_3D('',#57363,#45666,#45667);
#41042=AXIS2_PLACEMENT_3D('',#57364,#45668,#45669);
#41043=AXIS2_PLACEMENT_3D('',#57366,#45670,#45671);
#41044=AXIS2_PLACEMENT_3D('',#57369,#45673,#45674);
#41045=AXIS2_PLACEMENT_3D('',#57370,#45675,#45676);
#41046=AXIS2_PLACEMENT_3D('',#57372,#45677,#45678);
#41047=AXIS2_PLACEMENT_3D('',#57375,#45680,#45681);
#41048=AXIS2_PLACEMENT_3D('',#57376,#45682,#45683);
#41049=AXIS2_PLACEMENT_3D('',#57378,#45684,#45685);
#41050=AXIS2_PLACEMENT_3D('',#57381,#45687,#45688);
#41051=AXIS2_PLACEMENT_3D('',#57382,#45689,#45690);
#41052=AXIS2_PLACEMENT_3D('',#57385,#45691,#45692);
#41053=AXIS2_PLACEMENT_3D('',#57386,#45693,#45694);
#41054=AXIS2_PLACEMENT_3D('',#57389,#45696,#45697);
#41055=AXIS2_PLACEMENT_3D('',#57390,#45698,#45699);
#41056=AXIS2_PLACEMENT_3D('',#57393,#45700,#45701);
#41057=AXIS2_PLACEMENT_3D('',#57394,#45702,#45703);
#41058=AXIS2_PLACEMENT_3D('',#57397,#45705,#45706);
#41059=AXIS2_PLACEMENT_3D('',#57398,#45707,#45708);
#41060=AXIS2_PLACEMENT_3D('',#57401,#45710,#45711);
#41061=AXIS2_PLACEMENT_3D('',#57402,#45712,#45713);
#41062=AXIS2_PLACEMENT_3D('',#57405,#45714,#45715);
#41063=AXIS2_PLACEMENT_3D('',#57409,#45717,#45718);
#41064=AXIS2_PLACEMENT_3D('',#57411,#45720,#45721);
#41065=AXIS2_PLACEMENT_3D('',#57414,#45723,#45724);
#41066=AXIS2_PLACEMENT_3D('',#57415,#45725,#45726);
#41067=AXIS2_PLACEMENT_3D('',#57418,#45727,#45728);
#41068=AXIS2_PLACEMENT_3D('',#57422,#45730,#45731);
#41069=AXIS2_PLACEMENT_3D('',#57426,#45733,#45734);
#41070=AXIS2_PLACEMENT_3D('',#57430,#45736,#45737);
#41071=AXIS2_PLACEMENT_3D('',#57434,#45739,#45740);
#41072=AXIS2_PLACEMENT_3D('',#57438,#45742,#45743);
#41073=AXIS2_PLACEMENT_3D('',#57464,#45757,#45758);
#41074=AXIS2_PLACEMENT_3D('',#57473,#45763,#45764);
#41075=AXIS2_PLACEMENT_3D('',#57483,#45770,#45771);
#41076=AXIS2_PLACEMENT_3D('',#57493,#45777,#45778);
#41077=AXIS2_PLACEMENT_3D('',#57496,#45781,#45782);
#41078=AXIS2_PLACEMENT_3D('',#57509,#45789,#45790);
#41079=AXIS2_PLACEMENT_3D('',#57515,#45794,#45795);
#41080=AXIS2_PLACEMENT_3D('',#57525,#45801,#45802);
#41081=AXIS2_PLACEMENT_3D('',#57528,#45805,#45806);
#41082=AXIS2_PLACEMENT_3D('',#57537,#45811,#45812);
#41083=AXIS2_PLACEMENT_3D('',#57547,#45818,#45819);
#41084=AXIS2_PLACEMENT_3D('',#57557,#45825,#45826);
#41085=AXIS2_PLACEMENT_3D('',#57560,#45829,#45830);
#41086=AXIS2_PLACEMENT_3D('',#57563,#45831,#45832);
#41087=AXIS2_PLACEMENT_3D('',#57567,#45834,#45835);
#41088=AXIS2_PLACEMENT_3D('',#57571,#45837,#45838);
#41089=AXIS2_PLACEMENT_3D('',#57575,#45840,#45841);
#41090=AXIS2_PLACEMENT_3D('',#57579,#45843,#45844);
#41091=AXIS2_PLACEMENT_3D('',#57583,#45846,#45847);
#41092=AXIS2_PLACEMENT_3D('',#57588,#45852,#45853);
#41093=AXIS2_PLACEMENT_3D('',#57593,#45855,#45856);
#41094=AXIS2_PLACEMENT_3D('',#57597,#45858,#45859);
#41095=AXIS2_PLACEMENT_3D('',#57601,#45861,#45862);
#41096=AXIS2_PLACEMENT_3D('',#57604,#45864,#45865);
#41097=AXIS2_PLACEMENT_3D('',#57607,#45866,#45867);
#41098=AXIS2_PLACEMENT_3D('',#57611,#45869,#45870);
#41099=AXIS2_PLACEMENT_3D('',#57615,#45872,#45873);
#41100=AXIS2_PLACEMENT_3D('',#57619,#45875,#45876);
#41101=AXIS2_PLACEMENT_3D('',#57623,#45878,#45879);
#41102=AXIS2_PLACEMENT_3D('',#57627,#45881,#45882);
#41103=AXIS2_PLACEMENT_3D('',#57629,#45884,#45885);
#41104=AXIS2_PLACEMENT_3D('',#57633,#45887,#45888);
#41105=AXIS2_PLACEMENT_3D('',#57637,#45890,#45891);
#41106=AXIS2_PLACEMENT_3D('',#57641,#45893,#45894);
#41107=AXIS2_PLACEMENT_3D('',#57645,#45896,#45897);
#41108=AXIS2_PLACEMENT_3D('',#57649,#45899,#45900);
#41109=AXIS2_PLACEMENT_3D('',#57655,#45903,#45904);
#41110=AXIS2_PLACEMENT_3D('',#57659,#45906,#45907);
#41111=AXIS2_PLACEMENT_3D('',#57663,#45909,#45910);
#41112=AXIS2_PLACEMENT_3D('',#57667,#45912,#45913);
#41113=AXIS2_PLACEMENT_3D('',#57671,#45915,#45916);
#41114=AXIS2_PLACEMENT_3D('',#57674,#45918,#45919);
#41115=AXIS2_PLACEMENT_3D('',#57675,#45920,#45921);
#41116=AXIS2_PLACEMENT_3D('',#57680,#45923,#45924);
#41117=AXIS2_PLACEMENT_3D('',#57684,#45927,#45928);
#41118=AXIS2_PLACEMENT_3D('',#57685,#45929,#45930);
#41119=AXIS2_PLACEMENT_3D('',#57691,#45934,#45935);
#41120=AXIS2_PLACEMENT_3D('',#57696,#45937,#45938);
#41121=AXIS2_PLACEMENT_3D('',#57700,#45941,#45942);
#41122=AXIS2_PLACEMENT_3D('',#57701,#45943,#45944);
#41123=AXIS2_PLACEMENT_3D('',#57707,#45948,#45949);
#41124=AXIS2_PLACEMENT_3D('',#57710,#45951,#45952);
#41125=AXIS2_PLACEMENT_3D('',#57712,#45953,#45954);
#41126=AXIS2_PLACEMENT_3D('',#57714,#45956,#45957);
#41127=AXIS2_PLACEMENT_3D('',#57716,#45959,#45960);
#41128=AXIS2_PLACEMENT_3D('',#57719,#45962,#45963);
#41129=AXIS2_PLACEMENT_3D('',#57721,#45964,#45965);
#41130=AXIS2_PLACEMENT_3D('',#57723,#45967,#45968);
#41131=AXIS2_PLACEMENT_3D('',#57725,#45970,#45971);
#41132=AXIS2_PLACEMENT_3D('',#57729,#45974,#45975);
#41133=AXIS2_PLACEMENT_3D('',#57732,#45977,#45978);
#41134=AXIS2_PLACEMENT_3D('',#57733,#45979,#45980);
#41135=AXIS2_PLACEMENT_3D('',#57735,#45982,#45983);
#41136=AXIS2_PLACEMENT_3D('',#57736,#45984,#45985);
#41137=AXIS2_PLACEMENT_3D('',#57738,#45987,#45988);
#41138=AXIS2_PLACEMENT_3D('',#57740,#45990,#45991);
#41139=AXIS2_PLACEMENT_3D('',#57741,#45992,#45993);
#41140=AXIS2_PLACEMENT_3D('',#57742,#45994,#45995);
#41141=AXIS2_PLACEMENT_3D('',#57743,#45996,#45997);
#41142=AXIS2_PLACEMENT_3D('',#57744,#45998,#45999);
#41143=AXIS2_PLACEMENT_3D('',#57745,#46000,#46001);
#41144=AXIS2_PLACEMENT_3D('',#57746,#46002,#46003);
#41145=AXIS2_PLACEMENT_3D('',#57747,#46004,#46005);
#41146=AXIS2_PLACEMENT_3D('',#57748,#46006,#46007);
#41147=AXIS2_PLACEMENT_3D('',#57749,#46008,#46009);
#41148=AXIS2_PLACEMENT_3D('',#57750,#46010,#46011);
#41149=AXIS2_PLACEMENT_3D('',#57751,#46012,#46013);
#41150=AXIS2_PLACEMENT_3D('',#57752,#46014,#46015);
#41151=AXIS2_PLACEMENT_3D('',#57753,#46016,#46017);
#41152=AXIS2_PLACEMENT_3D('',#57754,#46018,#46019);
#41153=AXIS2_PLACEMENT_3D('',#57755,#46020,#46021);
#41154=AXIS2_PLACEMENT_3D('',#57756,#46022,#46023);
#41155=AXIS2_PLACEMENT_3D('',#57757,#46024,#46025);
#41156=AXIS2_PLACEMENT_3D('',#57760,#46028,#46029);
#41157=AXIS2_PLACEMENT_3D('',#57762,#46031,#46032);
#41158=AXIS2_PLACEMENT_3D('',#57764,#46034,#46035);
#41159=AXIS2_PLACEMENT_3D('',#57766,#46037,#46038);
#41160=AXIS2_PLACEMENT_3D('',#57768,#46040,#46041);
#41161=AXIS2_PLACEMENT_3D('',#57770,#46043,#46044);
#41162=AXIS2_PLACEMENT_3D('',#57772,#46046,#46047);
#41163=AXIS2_PLACEMENT_3D('',#57774,#46049,#46050);
#41164=AXIS2_PLACEMENT_3D('',#57776,#46052,#46053);
#41165=AXIS2_PLACEMENT_3D('',#57778,#46055,#46056);
#41166=AXIS2_PLACEMENT_3D('',#57780,#46058,#46059);
#41167=AXIS2_PLACEMENT_3D('',#57781,#46060,#46061);
#41168=AXIS2_PLACEMENT_3D('',#57784,#46064,#46065);
#41169=AXIS2_PLACEMENT_3D('',#57786,#46067,#46068);
#41170=AXIS2_PLACEMENT_3D('',#57788,#46070,#46071);
#41171=AXIS2_PLACEMENT_3D('',#57790,#46073,#46074);
#41172=AXIS2_PLACEMENT_3D('',#57792,#46076,#46077);
#41173=AXIS2_PLACEMENT_3D('',#57794,#46079,#46080);
#41174=AXIS2_PLACEMENT_3D('',#57796,#46082,#46083);
#41175=AXIS2_PLACEMENT_3D('',#57798,#46085,#46086);
#41176=AXIS2_PLACEMENT_3D('',#57800,#46088,#46089);
#41177=AXIS2_PLACEMENT_3D('',#57802,#46091,#46092);
#41178=AXIS2_PLACEMENT_3D('',#57804,#46094,#46095);
#41179=AXIS2_PLACEMENT_3D('',#57805,#46096,#46097);
#41180=AXIS2_PLACEMENT_3D('',#57807,#46099,#46100);
#41181=AXIS2_PLACEMENT_3D('',#57809,#46102,#46103);
#41182=AXIS2_PLACEMENT_3D('',#57811,#46105,#46106);
#41183=AXIS2_PLACEMENT_3D('',#57812,#46107,#46108);
#41184=AXIS2_PLACEMENT_3D('',#57813,#46109,#46110);
#41185=AXIS2_PLACEMENT_3D('',#57814,#46111,#46112);
#41186=AXIS2_PLACEMENT_3D('',#57815,#46113,#46114);
#41187=AXIS2_PLACEMENT_3D('',#57816,#46115,#46116);
#41188=AXIS2_PLACEMENT_3D('',#57817,#46117,#46118);
#41189=AXIS2_PLACEMENT_3D('',#57834,#46127,#46128);
#41190=AXIS2_PLACEMENT_3D('',#57837,#46131,#46132);
#41191=AXIS2_PLACEMENT_3D('',#57839,#46134,#46135);
#41192=AXIS2_PLACEMENT_3D('',#57841,#46137,#46138);
#41193=AXIS2_PLACEMENT_3D('',#57842,#46139,#46140);
#41194=AXIS2_PLACEMENT_3D('',#57851,#46145,#46146);
#41195=AXIS2_PLACEMENT_3D('',#57857,#46150,#46151);
#41196=AXIS2_PLACEMENT_3D('',#57863,#46155,#46156);
#41197=AXIS2_PLACEMENT_3D('',#57866,#46159,#46160);
#41198=AXIS2_PLACEMENT_3D('',#57868,#46162,#46163);
#41199=AXIS2_PLACEMENT_3D('',#57870,#46165,#46166);
#41200=AXIS2_PLACEMENT_3D('',#57871,#46167,#46168);
#41201=AXIS2_PLACEMENT_3D('',#57877,#46172,#46173);
#41202=AXIS2_PLACEMENT_3D('',#57881,#46176,#46177);
#41203=AXIS2_PLACEMENT_3D('',#57885,#46180,#46181);
#41204=AXIS2_PLACEMENT_3D('',#57887,#46183,#46184);
#41205=AXIS2_PLACEMENT_3D('',#57896,#46189,#46190);
#41206=AXIS2_PLACEMENT_3D('',#57905,#46195,#46196);
#41207=AXIS2_PLACEMENT_3D('',#57911,#46200,#46201);
#41208=AXIS2_PLACEMENT_3D('',#57917,#46205,#46206);
#41209=AXIS2_PLACEMENT_3D('',#57920,#46209,#46210);
#41210=AXIS2_PLACEMENT_3D('',#57923,#46213,#46214);
#41211=AXIS2_PLACEMENT_3D('',#57924,#46215,#46216);
#41212=AXIS2_PLACEMENT_3D('',#57925,#46217,#46218);
#41213=AXIS2_PLACEMENT_3D('',#57942,#46227,#46228);
#41214=AXIS2_PLACEMENT_3D('',#57945,#46231,#46232);
#41215=AXIS2_PLACEMENT_3D('',#57947,#46234,#46235);
#41216=AXIS2_PLACEMENT_3D('',#57949,#46237,#46238);
#41217=AXIS2_PLACEMENT_3D('',#57950,#46239,#46240);
#41218=AXIS2_PLACEMENT_3D('',#57959,#46245,#46246);
#41219=AXIS2_PLACEMENT_3D('',#57965,#46250,#46251);
#41220=AXIS2_PLACEMENT_3D('',#57971,#46255,#46256);
#41221=AXIS2_PLACEMENT_3D('',#57974,#46259,#46260);
#41222=AXIS2_PLACEMENT_3D('',#57977,#46263,#46264);
#41223=AXIS2_PLACEMENT_3D('',#57978,#46265,#46266);
#41224=AXIS2_PLACEMENT_3D('',#57979,#46267,#46268);
#41225=AXIS2_PLACEMENT_3D('',#57980,#46269,#46270);
#41226=AXIS2_PLACEMENT_3D('',#57989,#46275,#46276);
#41227=AXIS2_PLACEMENT_3D('',#57998,#46281,#46282);
#41228=AXIS2_PLACEMENT_3D('',#58001,#46285,#46286);
#41229=AXIS2_PLACEMENT_3D('',#58003,#46288,#46289);
#41230=AXIS2_PLACEMENT_3D('',#58005,#46291,#46292);
#41231=AXIS2_PLACEMENT_3D('',#58006,#46293,#46294);
#41232=AXIS2_PLACEMENT_3D('',#58008,#46295,#46296);
#41233=AXIS2_PLACEMENT_3D('',#58011,#46298,#46299);
#41234=AXIS2_PLACEMENT_3D('',#58012,#46300,#46301);
#41235=AXIS2_PLACEMENT_3D('',#58014,#46302,#46303);
#41236=AXIS2_PLACEMENT_3D('',#58017,#46305,#46306);
#41237=AXIS2_PLACEMENT_3D('',#58018,#46307,#46308);
#41238=AXIS2_PLACEMENT_3D('',#58021,#46309,#46310);
#41239=AXIS2_PLACEMENT_3D('',#58025,#46312,#46313);
#41240=AXIS2_PLACEMENT_3D('',#58027,#46315,#46316);
#41241=AXIS2_PLACEMENT_3D('',#58036,#46321,#46322);
#41242=AXIS2_PLACEMENT_3D('',#58045,#46327,#46328);
#41243=AXIS2_PLACEMENT_3D('',#58055,#46334,#46335);
#41244=AXIS2_PLACEMENT_3D('',#58065,#46341,#46342);
#41245=AXIS2_PLACEMENT_3D('',#58074,#46347,#46348);
#41246=AXIS2_PLACEMENT_3D('',#58083,#46353,#46354);
#41247=AXIS2_PLACEMENT_3D('',#58093,#46360,#46361);
#41248=AXIS2_PLACEMENT_3D('',#58103,#46367,#46368);
#41249=AXIS2_PLACEMENT_3D('',#58124,#46381,#46382);
#41250=AXIS2_PLACEMENT_3D('',#58153,#46397,#46398);
#41251=AXIS2_PLACEMENT_3D('',#58159,#46402,#46403);
#41252=AXIS2_PLACEMENT_3D('',#58163,#46406,#46407);
#41253=AXIS2_PLACEMENT_3D('',#58167,#46410,#46411);
#41254=AXIS2_PLACEMENT_3D('',#58169,#46413,#46414);
#41255=AXIS2_PLACEMENT_3D('',#58178,#46419,#46420);
#41256=AXIS2_PLACEMENT_3D('',#58180,#46421,#46422);
#41257=AXIS2_PLACEMENT_3D('',#58181,#46423,#46424);
#41258=AXIS2_PLACEMENT_3D('',#58202,#46437,#46438);
#41259=AXIS2_PLACEMENT_3D('',#58206,#46441,#46442);
#41260=AXIS2_PLACEMENT_3D('',#58208,#46443,#46444);
#41261=AXIS2_PLACEMENT_3D('',#58209,#46445,#46446);
#41262=AXIS2_PLACEMENT_3D('',#58228,#46458,#46459);
#41263=AXIS2_PLACEMENT_3D('',#58230,#46461,#46462);
#41264=AXIS2_PLACEMENT_3D('',#58232,#46464,#46465);
#41265=AXIS2_PLACEMENT_3D('',#58236,#46468,#46469);
#41266=AXIS2_PLACEMENT_3D('',#58240,#46472,#46473);
#41267=AXIS2_PLACEMENT_3D('',#58252,#46481,#46482);
#41268=AXIS2_PLACEMENT_3D('',#58253,#46483,#46484);
#41269=AXIS2_PLACEMENT_3D('',#58255,#46486,#46487);
#41270=AXIS2_PLACEMENT_3D('',#58259,#46490,#46491);
#41271=AXIS2_PLACEMENT_3D('',#58263,#46494,#46495);
#41272=AXIS2_PLACEMENT_3D('',#58275,#46503,#46504);
#41273=AXIS2_PLACEMENT_3D('',#58276,#46505,#46506);
#41274=AXIS2_PLACEMENT_3D('',#58277,#46507,#46508);
#41275=AXIS2_PLACEMENT_3D('',#58283,#46512,#46513);
#41276=AXIS2_PLACEMENT_3D('',#58284,#46514,#46515);
#41277=AXIS2_PLACEMENT_3D('',#58290,#46519,#46520);
#41278=AXIS2_PLACEMENT_3D('',#58293,#46523,#46524);
#41279=AXIS2_PLACEMENT_3D('',#58294,#46525,#46526);
#41280=AXIS2_PLACEMENT_3D('',#58300,#46530,#46531);
#41281=AXIS2_PLACEMENT_3D('',#58301,#46532,#46533);
#41282=AXIS2_PLACEMENT_3D('',#58307,#46537,#46538);
#41283=AXIS2_PLACEMENT_3D('',#58310,#46541,#46542);
#41284=AXIS2_PLACEMENT_3D('',#58311,#46543,#46544);
#41285=AXIS2_PLACEMENT_3D('',#58312,#46545,#46546);
#41286=AXIS2_PLACEMENT_3D('',#58313,#46547,#46548);
#41287=AXIS2_PLACEMENT_3D('',#58314,#46549,#46550);
#41288=AXIS2_PLACEMENT_3D('',#58315,#46551,#46552);
#41289=AXIS2_PLACEMENT_3D('',#58316,#46553,#46554);
#41290=AXIS2_PLACEMENT_3D('',#58319,#46557,#46558);
#41291=AXIS2_PLACEMENT_3D('',#58322,#46561,#46562);
#41292=AXIS2_PLACEMENT_3D('',#58324,#46564,#46565);
#41293=AXIS2_PLACEMENT_3D('',#58325,#46566,#46567);
#41294=AXIS2_PLACEMENT_3D('',#58327,#46569,#46570);
#41295=AXIS2_PLACEMENT_3D('',#58328,#46571,#46572);
#41296=AXIS2_PLACEMENT_3D('',#58330,#46574,#46575);
#41297=AXIS2_PLACEMENT_3D('',#58331,#46576,#46577);
#41298=AXIS2_PLACEMENT_3D('',#58333,#46579,#46580);
#41299=AXIS2_PLACEMENT_3D('',#58334,#46581,#46582);
#41300=AXIS2_PLACEMENT_3D('',#58337,#46585,#46586);
#41301=AXIS2_PLACEMENT_3D('',#58339,#46588,#46589);
#41302=AXIS2_PLACEMENT_3D('',#58341,#46591,#46592);
#41303=AXIS2_PLACEMENT_3D('',#58342,#46593,#46594);
#41304=AXIS2_PLACEMENT_3D('',#58344,#46595,#46596);
#41305=AXIS2_PLACEMENT_3D('',#58345,#46597,#46598);
#41306=AXIS2_PLACEMENT_3D('',#58347,#46599,#46600);
#41307=AXIS2_PLACEMENT_3D('',#58348,#46601,#46602);
#41308=AXIS2_PLACEMENT_3D('',#58349,#46603,#46604);
#41309=AXIS2_PLACEMENT_3D('',#58351,#46605,#46606);
#41310=AXIS2_PLACEMENT_3D('',#58353,#46607,#46608);
#41311=AXIS2_PLACEMENT_3D('',#58354,#46609,#46610);
#41312=AXIS2_PLACEMENT_3D('',#58355,#46611,#46612);
#41313=AXIS2_PLACEMENT_3D('',#58357,#46613,#46614);
#41314=AXIS2_PLACEMENT_3D('',#58359,#46615,#46616);
#41315=AXIS2_PLACEMENT_3D('',#58360,#46617,#46618);
#41316=AXIS2_PLACEMENT_3D('',#58361,#46619,#46620);
#41317=AXIS2_PLACEMENT_3D('',#58363,#46621,#46622);
#41318=AXIS2_PLACEMENT_3D('',#58364,#46623,#46624);
#41319=AXIS2_PLACEMENT_3D('',#58365,#46625,#46626);
#41320=AXIS2_PLACEMENT_3D('',#58367,#46627,#46628);
#41321=AXIS2_PLACEMENT_3D('',#58368,#46629,#46630);
#41322=AXIS2_PLACEMENT_3D('',#58369,#46631,#46632);
#41323=AXIS2_PLACEMENT_3D('',#58394,#46645,#46646);
#41324=AXIS2_PLACEMENT_3D('',#58419,#46659,#46660);
#41325=AXIS2_PLACEMENT_3D('',#58422,#46663,#46664);
#41326=AXIS2_PLACEMENT_3D('',#58425,#46667,#46668);
#41327=AXIS2_PLACEMENT_3D('',#58428,#46671,#46672);
#41328=AXIS2_PLACEMENT_3D('',#58431,#46675,#46676);
#41329=AXIS2_PLACEMENT_3D('',#58432,#46677,#46678);
#41330=AXIS2_PLACEMENT_3D('',#58435,#46681,#46682);
#41331=AXIS2_PLACEMENT_3D('',#58437,#46684,#46685);
#41332=AXIS2_PLACEMENT_3D('',#58439,#46687,#46688);
#41333=AXIS2_PLACEMENT_3D('',#58443,#46690,#46691);
#41334=AXIS2_PLACEMENT_3D('',#58444,#46692,#46693);
#41335=AXIS2_PLACEMENT_3D('',#58445,#46694,#46695);
#41336=AXIS2_PLACEMENT_3D('',#58447,#46696,#46697);
#41337=AXIS2_PLACEMENT_3D('',#58450,#46699,#46700);
#41338=AXIS2_PLACEMENT_3D('',#58451,#46701,#46702);
#41339=AXIS2_PLACEMENT_3D('',#58453,#46704,#46705);
#41340=AXIS2_PLACEMENT_3D('',#58455,#46707,#46708);
#41341=AXIS2_PLACEMENT_3D('',#58457,#46709,#46710);
#41342=AXIS2_PLACEMENT_3D('',#58460,#46712,#46713);
#41343=AXIS2_PLACEMENT_3D('',#58461,#46714,#46715);
#41344=AXIS2_PLACEMENT_3D('',#58465,#46717,#46718);
#41345=AXIS2_PLACEMENT_3D('',#58466,#46719,#46720);
#41346=AXIS2_PLACEMENT_3D('',#58467,#46721,#46722);
#41347=AXIS2_PLACEMENT_3D('',#58469,#46724,#46725);
#41348=AXIS2_PLACEMENT_3D('',#58471,#46727,#46728);
#41349=AXIS2_PLACEMENT_3D('',#58474,#46729,#46730);
#41350=AXIS2_PLACEMENT_3D('',#58478,#46732,#46733);
#41351=AXIS2_PLACEMENT_3D('',#58480,#46735,#46736);
#41352=AXIS2_PLACEMENT_3D('',#58489,#46741,#46742);
#41353=AXIS2_PLACEMENT_3D('',#58492,#46743,#46744);
#41354=AXIS2_PLACEMENT_3D('',#58496,#46746,#46747);
#41355=AXIS2_PLACEMENT_3D('',#58498,#46749,#46750);
#41356=AXIS2_PLACEMENT_3D('',#58501,#46753,#46754);
#41357=AXIS2_PLACEMENT_3D('',#58506,#46759,#46760);
#41358=AXIS2_PLACEMENT_3D('',#58508,#46762,#46763);
#41359=AXIS2_PLACEMENT_3D('',#58512,#46767,#46768);
#41360=AXIS2_PLACEMENT_3D('',#58513,#46769,#46770);
#41361=AXIS2_PLACEMENT_3D('',#58514,#46771,#46772);
#41362=AXIS2_PLACEMENT_3D('',#58515,#46773,#46774);
#41363=AXIS2_PLACEMENT_3D('',#58519,#46776,#46777);
#41364=AXIS2_PLACEMENT_3D('',#58520,#46778,#46779);
#41365=AXIS2_PLACEMENT_3D('',#58521,#46780,#46781);
#41366=AXIS2_PLACEMENT_3D('',#58523,#46782,#46783);
#41367=AXIS2_PLACEMENT_3D('',#58526,#46785,#46786);
#41368=AXIS2_PLACEMENT_3D('',#58527,#46787,#46788);
#41369=AXIS2_PLACEMENT_3D('',#58529,#46790,#46791);
#41370=AXIS2_PLACEMENT_3D('',#58531,#46793,#46794);
#41371=AXIS2_PLACEMENT_3D('',#58533,#46795,#46796);
#41372=AXIS2_PLACEMENT_3D('',#58536,#46798,#46799);
#41373=AXIS2_PLACEMENT_3D('',#58537,#46800,#46801);
#41374=AXIS2_PLACEMENT_3D('',#58541,#46803,#46804);
#41375=AXIS2_PLACEMENT_3D('',#58542,#46805,#46806);
#41376=AXIS2_PLACEMENT_3D('',#58543,#46807,#46808);
#41377=AXIS2_PLACEMENT_3D('',#58545,#46810,#46811);
#41378=AXIS2_PLACEMENT_3D('',#58547,#46813,#46814);
#41379=AXIS2_PLACEMENT_3D('',#58550,#46815,#46816);
#41380=AXIS2_PLACEMENT_3D('',#58554,#46818,#46819);
#41381=AXIS2_PLACEMENT_3D('',#58556,#46821,#46822);
#41382=AXIS2_PLACEMENT_3D('',#58565,#46827,#46828);
#41383=AXIS2_PLACEMENT_3D('',#58568,#46829,#46830);
#41384=AXIS2_PLACEMENT_3D('',#58572,#46832,#46833);
#41385=AXIS2_PLACEMENT_3D('',#58574,#46835,#46836);
#41386=AXIS2_PLACEMENT_3D('',#58577,#46839,#46840);
#41387=AXIS2_PLACEMENT_3D('',#58582,#46845,#46846);
#41388=AXIS2_PLACEMENT_3D('',#58584,#46848,#46849);
#41389=AXIS2_PLACEMENT_3D('',#58588,#46853,#46854);
#41390=AXIS2_PLACEMENT_3D('',#58589,#46855,#46856);
#41391=AXIS2_PLACEMENT_3D('',#58590,#46857,#46858);
#41392=AXIS2_PLACEMENT_3D('',#58591,#46859,#46860);
#41393=AXIS2_PLACEMENT_3D('',#60824,#47977,#47978);
#41394=AXIS2_PLACEMENT_3D('',#63057,#49095,#49096);
#41395=AXIS2_PLACEMENT_3D('',#63060,#49099,#49100);
#41396=AXIS2_PLACEMENT_3D('',#63062,#49102,#49103);
#41397=AXIS2_PLACEMENT_3D('',#63064,#49105,#49106);
#41398=AXIS2_PLACEMENT_3D('',#63066,#49108,#49109);
#41399=AXIS2_PLACEMENT_3D('',#63068,#49111,#49112);
#41400=AXIS2_PLACEMENT_3D('',#63069,#49113,#49114);
#41401=AXIS2_PLACEMENT_3D('',#63072,#49117,#49118);
#41402=AXIS2_PLACEMENT_3D('',#63074,#49120,#49121);
#41403=AXIS2_PLACEMENT_3D('',#63076,#49123,#49124);
#41404=AXIS2_PLACEMENT_3D('',#63078,#49126,#49127);
#41405=AXIS2_PLACEMENT_3D('',#63080,#49129,#49130);
#41406=AXIS2_PLACEMENT_3D('',#63081,#49131,#49132);
#41407=AXIS2_PLACEMENT_3D('',#63084,#49135,#49136);
#41408=AXIS2_PLACEMENT_3D('',#63086,#49138,#49139);
#41409=AXIS2_PLACEMENT_3D('',#63088,#49141,#49142);
#41410=AXIS2_PLACEMENT_3D('',#63090,#49144,#49145);
#41411=AXIS2_PLACEMENT_3D('',#63092,#49147,#49148);
#41412=AXIS2_PLACEMENT_3D('',#63093,#49149,#49150);
#41413=AXIS2_PLACEMENT_3D('',#63096,#49153,#49154);
#41414=AXIS2_PLACEMENT_3D('',#63098,#49156,#49157);
#41415=AXIS2_PLACEMENT_3D('',#63100,#49159,#49160);
#41416=AXIS2_PLACEMENT_3D('',#63102,#49162,#49163);
#41417=AXIS2_PLACEMENT_3D('',#63104,#49165,#49166);
#41418=AXIS2_PLACEMENT_3D('',#63105,#49167,#49168);
#41419=AXIS2_PLACEMENT_3D('',#63108,#49171,#49172);
#41420=AXIS2_PLACEMENT_3D('',#63110,#49174,#49175);
#41421=AXIS2_PLACEMENT_3D('',#63112,#49177,#49178);
#41422=AXIS2_PLACEMENT_3D('',#63114,#49180,#49181);
#41423=AXIS2_PLACEMENT_3D('',#63116,#49183,#49184);
#41424=AXIS2_PLACEMENT_3D('',#63117,#49185,#49186);
#41425=AXIS2_PLACEMENT_3D('',#63120,#49189,#49190);
#41426=AXIS2_PLACEMENT_3D('',#63122,#49192,#49193);
#41427=AXIS2_PLACEMENT_3D('',#63124,#49195,#49196);
#41428=AXIS2_PLACEMENT_3D('',#63126,#49198,#49199);
#41429=AXIS2_PLACEMENT_3D('',#63128,#49201,#49202);
#41430=AXIS2_PLACEMENT_3D('',#63129,#49203,#49204);
#41431=AXIS2_PLACEMENT_3D('',#63132,#49207,#49208);
#41432=AXIS2_PLACEMENT_3D('',#63134,#49210,#49211);
#41433=AXIS2_PLACEMENT_3D('',#63136,#49213,#49214);
#41434=AXIS2_PLACEMENT_3D('',#63138,#49216,#49217);
#41435=AXIS2_PLACEMENT_3D('',#63140,#49219,#49220);
#41436=AXIS2_PLACEMENT_3D('',#63141,#49221,#49222);
#41437=AXIS2_PLACEMENT_3D('',#63144,#49225,#49226);
#41438=AXIS2_PLACEMENT_3D('',#63146,#49228,#49229);
#41439=AXIS2_PLACEMENT_3D('',#63148,#49231,#49232);
#41440=AXIS2_PLACEMENT_3D('',#63150,#49234,#49235);
#41441=AXIS2_PLACEMENT_3D('',#63152,#49237,#49238);
#41442=AXIS2_PLACEMENT_3D('',#63153,#49239,#49240);
#41443=AXIS2_PLACEMENT_3D('',#63156,#49243,#49244);
#41444=AXIS2_PLACEMENT_3D('',#63158,#49246,#49247);
#41445=AXIS2_PLACEMENT_3D('',#63160,#49249,#49250);
#41446=AXIS2_PLACEMENT_3D('',#63162,#49252,#49253);
#41447=AXIS2_PLACEMENT_3D('',#63164,#49255,#49256);
#41448=AXIS2_PLACEMENT_3D('',#63165,#49257,#49258);
#41449=AXIS2_PLACEMENT_3D('',#63168,#49261,#49262);
#41450=AXIS2_PLACEMENT_3D('',#63170,#49264,#49265);
#41451=AXIS2_PLACEMENT_3D('',#63172,#49267,#49268);
#41452=AXIS2_PLACEMENT_3D('',#63174,#49270,#49271);
#41453=AXIS2_PLACEMENT_3D('',#63176,#49273,#49274);
#41454=AXIS2_PLACEMENT_3D('',#63177,#49275,#49276);
#41455=AXIS2_PLACEMENT_3D('',#63180,#49279,#49280);
#41456=AXIS2_PLACEMENT_3D('',#63182,#49282,#49283);
#41457=AXIS2_PLACEMENT_3D('',#63184,#49285,#49286);
#41458=AXIS2_PLACEMENT_3D('',#63186,#49288,#49289);
#41459=AXIS2_PLACEMENT_3D('',#63188,#49291,#49292);
#41460=AXIS2_PLACEMENT_3D('',#63189,#49293,#49294);
#41461=AXIS2_PLACEMENT_3D('',#63192,#49297,#49298);
#41462=AXIS2_PLACEMENT_3D('',#63194,#49300,#49301);
#41463=AXIS2_PLACEMENT_3D('',#63196,#49303,#49304);
#41464=AXIS2_PLACEMENT_3D('',#63198,#49306,#49307);
#41465=AXIS2_PLACEMENT_3D('',#63200,#49309,#49310);
#41466=AXIS2_PLACEMENT_3D('',#63201,#49311,#49312);
#41467=AXIS2_PLACEMENT_3D('',#63204,#49315,#49316);
#41468=AXIS2_PLACEMENT_3D('',#63206,#49318,#49319);
#41469=AXIS2_PLACEMENT_3D('',#63208,#49321,#49322);
#41470=AXIS2_PLACEMENT_3D('',#63210,#49324,#49325);
#41471=AXIS2_PLACEMENT_3D('',#63212,#49327,#49328);
#41472=AXIS2_PLACEMENT_3D('',#63213,#49329,#49330);
#41473=AXIS2_PLACEMENT_3D('',#63216,#49333,#49334);
#41474=AXIS2_PLACEMENT_3D('',#63218,#49336,#49337);
#41475=AXIS2_PLACEMENT_3D('',#63220,#49339,#49340);
#41476=AXIS2_PLACEMENT_3D('',#63222,#49342,#49343);
#41477=AXIS2_PLACEMENT_3D('',#63224,#49345,#49346);
#41478=AXIS2_PLACEMENT_3D('',#63225,#49347,#49348);
#41479=AXIS2_PLACEMENT_3D('',#63228,#49351,#49352);
#41480=AXIS2_PLACEMENT_3D('',#63230,#49354,#49355);
#41481=AXIS2_PLACEMENT_3D('',#63232,#49357,#49358);
#41482=AXIS2_PLACEMENT_3D('',#63234,#49360,#49361);
#41483=AXIS2_PLACEMENT_3D('',#63236,#49363,#49364);
#41484=AXIS2_PLACEMENT_3D('',#63237,#49365,#49366);
#41485=AXIS2_PLACEMENT_3D('',#63240,#49369,#49370);
#41486=AXIS2_PLACEMENT_3D('',#63242,#49372,#49373);
#41487=AXIS2_PLACEMENT_3D('',#63244,#49375,#49376);
#41488=AXIS2_PLACEMENT_3D('',#63246,#49378,#49379);
#41489=AXIS2_PLACEMENT_3D('',#63248,#49381,#49382);
#41490=AXIS2_PLACEMENT_3D('',#63249,#49383,#49384);
#41491=AXIS2_PLACEMENT_3D('',#63252,#49387,#49388);
#41492=AXIS2_PLACEMENT_3D('',#63254,#49390,#49391);
#41493=AXIS2_PLACEMENT_3D('',#63256,#49393,#49394);
#41494=AXIS2_PLACEMENT_3D('',#63258,#49396,#49397);
#41495=AXIS2_PLACEMENT_3D('',#63260,#49399,#49400);
#41496=AXIS2_PLACEMENT_3D('',#63261,#49401,#49402);
#41497=AXIS2_PLACEMENT_3D('',#63264,#49405,#49406);
#41498=AXIS2_PLACEMENT_3D('',#63266,#49408,#49409);
#41499=AXIS2_PLACEMENT_3D('',#63268,#49411,#49412);
#41500=AXIS2_PLACEMENT_3D('',#63270,#49414,#49415);
#41501=AXIS2_PLACEMENT_3D('',#63272,#49417,#49418);
#41502=AXIS2_PLACEMENT_3D('',#63273,#49419,#49420);
#41503=AXIS2_PLACEMENT_3D('',#63276,#49423,#49424);
#41504=AXIS2_PLACEMENT_3D('',#63278,#49426,#49427);
#41505=AXIS2_PLACEMENT_3D('',#63280,#49429,#49430);
#41506=AXIS2_PLACEMENT_3D('',#63282,#49432,#49433);
#41507=AXIS2_PLACEMENT_3D('',#63284,#49435,#49436);
#41508=AXIS2_PLACEMENT_3D('',#63285,#49437,#49438);
#41509=AXIS2_PLACEMENT_3D('',#63288,#49441,#49442);
#41510=AXIS2_PLACEMENT_3D('',#63290,#49444,#49445);
#41511=AXIS2_PLACEMENT_3D('',#63292,#49447,#49448);
#41512=AXIS2_PLACEMENT_3D('',#63294,#49450,#49451);
#41513=AXIS2_PLACEMENT_3D('',#63296,#49453,#49454);
#41514=AXIS2_PLACEMENT_3D('',#63297,#49455,#49456);
#41515=AXIS2_PLACEMENT_3D('',#63300,#49459,#49460);
#41516=AXIS2_PLACEMENT_3D('',#63302,#49462,#49463);
#41517=AXIS2_PLACEMENT_3D('',#63304,#49465,#49466);
#41518=AXIS2_PLACEMENT_3D('',#63306,#49468,#49469);
#41519=AXIS2_PLACEMENT_3D('',#63308,#49471,#49472);
#41520=AXIS2_PLACEMENT_3D('',#63309,#49473,#49474);
#41521=AXIS2_PLACEMENT_3D('',#63312,#49477,#49478);
#41522=AXIS2_PLACEMENT_3D('',#63314,#49480,#49481);
#41523=AXIS2_PLACEMENT_3D('',#63316,#49483,#49484);
#41524=AXIS2_PLACEMENT_3D('',#63318,#49486,#49487);
#41525=AXIS2_PLACEMENT_3D('',#63320,#49489,#49490);
#41526=AXIS2_PLACEMENT_3D('',#63321,#49491,#49492);
#41527=AXIS2_PLACEMENT_3D('',#63324,#49495,#49496);
#41528=AXIS2_PLACEMENT_3D('',#63326,#49498,#49499);
#41529=AXIS2_PLACEMENT_3D('',#63328,#49501,#49502);
#41530=AXIS2_PLACEMENT_3D('',#63330,#49504,#49505);
#41531=AXIS2_PLACEMENT_3D('',#63332,#49507,#49508);
#41532=AXIS2_PLACEMENT_3D('',#63333,#49509,#49510);
#41533=AXIS2_PLACEMENT_3D('',#63336,#49513,#49514);
#41534=AXIS2_PLACEMENT_3D('',#63338,#49516,#49517);
#41535=AXIS2_PLACEMENT_3D('',#63340,#49519,#49520);
#41536=AXIS2_PLACEMENT_3D('',#63342,#49522,#49523);
#41537=AXIS2_PLACEMENT_3D('',#63344,#49525,#49526);
#41538=AXIS2_PLACEMENT_3D('',#63345,#49527,#49528);
#41539=AXIS2_PLACEMENT_3D('',#63348,#49531,#49532);
#41540=AXIS2_PLACEMENT_3D('',#63350,#49534,#49535);
#41541=AXIS2_PLACEMENT_3D('',#63352,#49537,#49538);
#41542=AXIS2_PLACEMENT_3D('',#63354,#49540,#49541);
#41543=AXIS2_PLACEMENT_3D('',#63356,#49543,#49544);
#41544=AXIS2_PLACEMENT_3D('',#63357,#49545,#49546);
#41545=AXIS2_PLACEMENT_3D('',#63360,#49549,#49550);
#41546=AXIS2_PLACEMENT_3D('',#63362,#49552,#49553);
#41547=AXIS2_PLACEMENT_3D('',#63364,#49555,#49556);
#41548=AXIS2_PLACEMENT_3D('',#63366,#49558,#49559);
#41549=AXIS2_PLACEMENT_3D('',#63368,#49561,#49562);
#41550=AXIS2_PLACEMENT_3D('',#63369,#49563,#49564);
#41551=AXIS2_PLACEMENT_3D('',#63372,#49567,#49568);
#41552=AXIS2_PLACEMENT_3D('',#63374,#49570,#49571);
#41553=AXIS2_PLACEMENT_3D('',#63376,#49573,#49574);
#41554=AXIS2_PLACEMENT_3D('',#63378,#49576,#49577);
#41555=AXIS2_PLACEMENT_3D('',#63380,#49579,#49580);
#41556=AXIS2_PLACEMENT_3D('',#63381,#49581,#49582);
#41557=AXIS2_PLACEMENT_3D('',#63384,#49585,#49586);
#41558=AXIS2_PLACEMENT_3D('',#63386,#49588,#49589);
#41559=AXIS2_PLACEMENT_3D('',#63388,#49591,#49592);
#41560=AXIS2_PLACEMENT_3D('',#63390,#49594,#49595);
#41561=AXIS2_PLACEMENT_3D('',#63392,#49597,#49598);
#41562=AXIS2_PLACEMENT_3D('',#63393,#49599,#49600);
#41563=AXIS2_PLACEMENT_3D('',#63396,#49603,#49604);
#41564=AXIS2_PLACEMENT_3D('',#63398,#49606,#49607);
#41565=AXIS2_PLACEMENT_3D('',#63400,#49609,#49610);
#41566=AXIS2_PLACEMENT_3D('',#63402,#49612,#49613);
#41567=AXIS2_PLACEMENT_3D('',#63404,#49615,#49616);
#41568=AXIS2_PLACEMENT_3D('',#63405,#49617,#49618);
#41569=AXIS2_PLACEMENT_3D('',#63408,#49621,#49622);
#41570=AXIS2_PLACEMENT_3D('',#63410,#49624,#49625);
#41571=AXIS2_PLACEMENT_3D('',#63412,#49627,#49628);
#41572=AXIS2_PLACEMENT_3D('',#63414,#49630,#49631);
#41573=AXIS2_PLACEMENT_3D('',#63416,#49633,#49634);
#41574=AXIS2_PLACEMENT_3D('',#63417,#49635,#49636);
#41575=AXIS2_PLACEMENT_3D('',#63420,#49639,#49640);
#41576=AXIS2_PLACEMENT_3D('',#63422,#49642,#49643);
#41577=AXIS2_PLACEMENT_3D('',#63424,#49645,#49646);
#41578=AXIS2_PLACEMENT_3D('',#63426,#49648,#49649);
#41579=AXIS2_PLACEMENT_3D('',#63428,#49651,#49652);
#41580=AXIS2_PLACEMENT_3D('',#63429,#49653,#49654);
#41581=AXIS2_PLACEMENT_3D('',#63432,#49657,#49658);
#41582=AXIS2_PLACEMENT_3D('',#63434,#49660,#49661);
#41583=AXIS2_PLACEMENT_3D('',#63436,#49663,#49664);
#41584=AXIS2_PLACEMENT_3D('',#63438,#49666,#49667);
#41585=AXIS2_PLACEMENT_3D('',#63440,#49669,#49670);
#41586=AXIS2_PLACEMENT_3D('',#63441,#49671,#49672);
#41587=AXIS2_PLACEMENT_3D('',#63444,#49675,#49676);
#41588=AXIS2_PLACEMENT_3D('',#63446,#49678,#49679);
#41589=AXIS2_PLACEMENT_3D('',#63448,#49681,#49682);
#41590=AXIS2_PLACEMENT_3D('',#63450,#49684,#49685);
#41591=AXIS2_PLACEMENT_3D('',#63452,#49687,#49688);
#41592=AXIS2_PLACEMENT_3D('',#63453,#49689,#49690);
#41593=AXIS2_PLACEMENT_3D('',#63456,#49693,#49694);
#41594=AXIS2_PLACEMENT_3D('',#63458,#49696,#49697);
#41595=AXIS2_PLACEMENT_3D('',#63460,#49699,#49700);
#41596=AXIS2_PLACEMENT_3D('',#63462,#49702,#49703);
#41597=AXIS2_PLACEMENT_3D('',#63464,#49705,#49706);
#41598=AXIS2_PLACEMENT_3D('',#63465,#49707,#49708);
#41599=AXIS2_PLACEMENT_3D('',#63468,#49711,#49712);
#41600=AXIS2_PLACEMENT_3D('',#63470,#49714,#49715);
#41601=AXIS2_PLACEMENT_3D('',#63472,#49717,#49718);
#41602=AXIS2_PLACEMENT_3D('',#63474,#49720,#49721);
#41603=AXIS2_PLACEMENT_3D('',#63476,#49723,#49724);
#41604=AXIS2_PLACEMENT_3D('',#63477,#49725,#49726);
#41605=AXIS2_PLACEMENT_3D('',#63480,#49729,#49730);
#41606=AXIS2_PLACEMENT_3D('',#63482,#49732,#49733);
#41607=AXIS2_PLACEMENT_3D('',#63484,#49735,#49736);
#41608=AXIS2_PLACEMENT_3D('',#63486,#49738,#49739);
#41609=AXIS2_PLACEMENT_3D('',#63488,#49741,#49742);
#41610=AXIS2_PLACEMENT_3D('',#63489,#49743,#49744);
#41611=AXIS2_PLACEMENT_3D('',#63492,#49747,#49748);
#41612=AXIS2_PLACEMENT_3D('',#63494,#49750,#49751);
#41613=AXIS2_PLACEMENT_3D('',#63496,#49753,#49754);
#41614=AXIS2_PLACEMENT_3D('',#63498,#49756,#49757);
#41615=AXIS2_PLACEMENT_3D('',#63500,#49759,#49760);
#41616=AXIS2_PLACEMENT_3D('',#63501,#49761,#49762);
#41617=AXIS2_PLACEMENT_3D('',#63504,#49765,#49766);
#41618=AXIS2_PLACEMENT_3D('',#63506,#49768,#49769);
#41619=AXIS2_PLACEMENT_3D('',#63508,#49771,#49772);
#41620=AXIS2_PLACEMENT_3D('',#63510,#49774,#49775);
#41621=AXIS2_PLACEMENT_3D('',#63512,#49777,#49778);
#41622=AXIS2_PLACEMENT_3D('',#63513,#49779,#49780);
#41623=AXIS2_PLACEMENT_3D('',#63516,#49783,#49784);
#41624=AXIS2_PLACEMENT_3D('',#63518,#49786,#49787);
#41625=AXIS2_PLACEMENT_3D('',#63520,#49789,#49790);
#41626=AXIS2_PLACEMENT_3D('',#63522,#49792,#49793);
#41627=AXIS2_PLACEMENT_3D('',#63524,#49795,#49796);
#41628=AXIS2_PLACEMENT_3D('',#63525,#49797,#49798);
#41629=AXIS2_PLACEMENT_3D('',#63528,#49801,#49802);
#41630=AXIS2_PLACEMENT_3D('',#63530,#49804,#49805);
#41631=AXIS2_PLACEMENT_3D('',#63532,#49807,#49808);
#41632=AXIS2_PLACEMENT_3D('',#63534,#49810,#49811);
#41633=AXIS2_PLACEMENT_3D('',#63536,#49813,#49814);
#41634=AXIS2_PLACEMENT_3D('',#63537,#49815,#49816);
#41635=AXIS2_PLACEMENT_3D('',#63540,#49819,#49820);
#41636=AXIS2_PLACEMENT_3D('',#63542,#49822,#49823);
#41637=AXIS2_PLACEMENT_3D('',#63544,#49825,#49826);
#41638=AXIS2_PLACEMENT_3D('',#63546,#49828,#49829);
#41639=AXIS2_PLACEMENT_3D('',#63548,#49831,#49832);
#41640=AXIS2_PLACEMENT_3D('',#63549,#49833,#49834);
#41641=AXIS2_PLACEMENT_3D('',#63552,#49837,#49838);
#41642=AXIS2_PLACEMENT_3D('',#63554,#49840,#49841);
#41643=AXIS2_PLACEMENT_3D('',#63556,#49843,#49844);
#41644=AXIS2_PLACEMENT_3D('',#63558,#49846,#49847);
#41645=AXIS2_PLACEMENT_3D('',#63560,#49849,#49850);
#41646=AXIS2_PLACEMENT_3D('',#63561,#49851,#49852);
#41647=AXIS2_PLACEMENT_3D('',#63564,#49855,#49856);
#41648=AXIS2_PLACEMENT_3D('',#63566,#49858,#49859);
#41649=AXIS2_PLACEMENT_3D('',#63568,#49861,#49862);
#41650=AXIS2_PLACEMENT_3D('',#63570,#49864,#49865);
#41651=AXIS2_PLACEMENT_3D('',#63572,#49867,#49868);
#41652=AXIS2_PLACEMENT_3D('',#63573,#49869,#49870);
#41653=AXIS2_PLACEMENT_3D('',#63576,#49873,#49874);
#41654=AXIS2_PLACEMENT_3D('',#63578,#49876,#49877);
#41655=AXIS2_PLACEMENT_3D('',#63580,#49879,#49880);
#41656=AXIS2_PLACEMENT_3D('',#63582,#49882,#49883);
#41657=AXIS2_PLACEMENT_3D('',#63584,#49885,#49886);
#41658=AXIS2_PLACEMENT_3D('',#63585,#49887,#49888);
#41659=AXIS2_PLACEMENT_3D('',#63588,#49891,#49892);
#41660=AXIS2_PLACEMENT_3D('',#63590,#49894,#49895);
#41661=AXIS2_PLACEMENT_3D('',#63592,#49897,#49898);
#41662=AXIS2_PLACEMENT_3D('',#63594,#49900,#49901);
#41663=AXIS2_PLACEMENT_3D('',#63596,#49903,#49904);
#41664=AXIS2_PLACEMENT_3D('',#63597,#49905,#49906);
#41665=AXIS2_PLACEMENT_3D('',#63600,#49909,#49910);
#41666=AXIS2_PLACEMENT_3D('',#63602,#49912,#49913);
#41667=AXIS2_PLACEMENT_3D('',#63604,#49915,#49916);
#41668=AXIS2_PLACEMENT_3D('',#63606,#49918,#49919);
#41669=AXIS2_PLACEMENT_3D('',#63608,#49921,#49922);
#41670=AXIS2_PLACEMENT_3D('',#63609,#49923,#49924);
#41671=AXIS2_PLACEMENT_3D('',#63612,#49927,#49928);
#41672=AXIS2_PLACEMENT_3D('',#63614,#49930,#49931);
#41673=AXIS2_PLACEMENT_3D('',#63616,#49933,#49934);
#41674=AXIS2_PLACEMENT_3D('',#63618,#49936,#49937);
#41675=AXIS2_PLACEMENT_3D('',#63620,#49939,#49940);
#41676=AXIS2_PLACEMENT_3D('',#63621,#49941,#49942);
#41677=AXIS2_PLACEMENT_3D('',#63624,#49945,#49946);
#41678=AXIS2_PLACEMENT_3D('',#63626,#49948,#49949);
#41679=AXIS2_PLACEMENT_3D('',#63628,#49951,#49952);
#41680=AXIS2_PLACEMENT_3D('',#63630,#49954,#49955);
#41681=AXIS2_PLACEMENT_3D('',#63632,#49957,#49958);
#41682=AXIS2_PLACEMENT_3D('',#63633,#49959,#49960);
#41683=AXIS2_PLACEMENT_3D('',#63636,#49963,#49964);
#41684=AXIS2_PLACEMENT_3D('',#63638,#49966,#49967);
#41685=AXIS2_PLACEMENT_3D('',#63640,#49969,#49970);
#41686=AXIS2_PLACEMENT_3D('',#63642,#49972,#49973);
#41687=AXIS2_PLACEMENT_3D('',#63644,#49975,#49976);
#41688=AXIS2_PLACEMENT_3D('',#63645,#49977,#49978);
#41689=AXIS2_PLACEMENT_3D('',#63648,#49981,#49982);
#41690=AXIS2_PLACEMENT_3D('',#63650,#49984,#49985);
#41691=AXIS2_PLACEMENT_3D('',#63652,#49987,#49988);
#41692=AXIS2_PLACEMENT_3D('',#63654,#49990,#49991);
#41693=AXIS2_PLACEMENT_3D('',#63656,#49993,#49994);
#41694=AXIS2_PLACEMENT_3D('',#63657,#49995,#49996);
#41695=AXIS2_PLACEMENT_3D('',#63660,#49999,#50000);
#41696=AXIS2_PLACEMENT_3D('',#63662,#50002,#50003);
#41697=AXIS2_PLACEMENT_3D('',#63664,#50005,#50006);
#41698=AXIS2_PLACEMENT_3D('',#63666,#50008,#50009);
#41699=AXIS2_PLACEMENT_3D('',#63668,#50011,#50012);
#41700=AXIS2_PLACEMENT_3D('',#63669,#50013,#50014);
#41701=AXIS2_PLACEMENT_3D('',#63672,#50017,#50018);
#41702=AXIS2_PLACEMENT_3D('',#63674,#50020,#50021);
#41703=AXIS2_PLACEMENT_3D('',#63676,#50023,#50024);
#41704=AXIS2_PLACEMENT_3D('',#63678,#50026,#50027);
#41705=AXIS2_PLACEMENT_3D('',#63680,#50029,#50030);
#41706=AXIS2_PLACEMENT_3D('',#63681,#50031,#50032);
#41707=AXIS2_PLACEMENT_3D('',#63684,#50035,#50036);
#41708=AXIS2_PLACEMENT_3D('',#63686,#50038,#50039);
#41709=AXIS2_PLACEMENT_3D('',#63688,#50041,#50042);
#41710=AXIS2_PLACEMENT_3D('',#63690,#50044,#50045);
#41711=AXIS2_PLACEMENT_3D('',#63692,#50047,#50048);
#41712=AXIS2_PLACEMENT_3D('',#63693,#50049,#50050);
#41713=AXIS2_PLACEMENT_3D('',#63696,#50053,#50054);
#41714=AXIS2_PLACEMENT_3D('',#63698,#50056,#50057);
#41715=AXIS2_PLACEMENT_3D('',#63700,#50059,#50060);
#41716=AXIS2_PLACEMENT_3D('',#63702,#50062,#50063);
#41717=AXIS2_PLACEMENT_3D('',#63704,#50065,#50066);
#41718=AXIS2_PLACEMENT_3D('',#63705,#50067,#50068);
#41719=AXIS2_PLACEMENT_3D('',#63708,#50071,#50072);
#41720=AXIS2_PLACEMENT_3D('',#63710,#50074,#50075);
#41721=AXIS2_PLACEMENT_3D('',#63712,#50077,#50078);
#41722=AXIS2_PLACEMENT_3D('',#63714,#50080,#50081);
#41723=AXIS2_PLACEMENT_3D('',#63716,#50083,#50084);
#41724=AXIS2_PLACEMENT_3D('',#63717,#50085,#50086);
#41725=AXIS2_PLACEMENT_3D('',#63720,#50089,#50090);
#41726=AXIS2_PLACEMENT_3D('',#63722,#50092,#50093);
#41727=AXIS2_PLACEMENT_3D('',#63724,#50095,#50096);
#41728=AXIS2_PLACEMENT_3D('',#63726,#50098,#50099);
#41729=AXIS2_PLACEMENT_3D('',#63728,#50101,#50102);
#41730=AXIS2_PLACEMENT_3D('',#63729,#50103,#50104);
#41731=AXIS2_PLACEMENT_3D('',#63732,#50107,#50108);
#41732=AXIS2_PLACEMENT_3D('',#63734,#50110,#50111);
#41733=AXIS2_PLACEMENT_3D('',#63736,#50113,#50114);
#41734=AXIS2_PLACEMENT_3D('',#63738,#50116,#50117);
#41735=AXIS2_PLACEMENT_3D('',#63740,#50119,#50120);
#41736=AXIS2_PLACEMENT_3D('',#63741,#50121,#50122);
#41737=AXIS2_PLACEMENT_3D('',#63744,#50125,#50126);
#41738=AXIS2_PLACEMENT_3D('',#63746,#50128,#50129);
#41739=AXIS2_PLACEMENT_3D('',#63748,#50131,#50132);
#41740=AXIS2_PLACEMENT_3D('',#63750,#50134,#50135);
#41741=AXIS2_PLACEMENT_3D('',#63752,#50137,#50138);
#41742=AXIS2_PLACEMENT_3D('',#63753,#50139,#50140);
#41743=AXIS2_PLACEMENT_3D('',#63756,#50143,#50144);
#41744=AXIS2_PLACEMENT_3D('',#63758,#50146,#50147);
#41745=AXIS2_PLACEMENT_3D('',#63760,#50149,#50150);
#41746=AXIS2_PLACEMENT_3D('',#63762,#50152,#50153);
#41747=AXIS2_PLACEMENT_3D('',#63764,#50155,#50156);
#41748=AXIS2_PLACEMENT_3D('',#63765,#50157,#50158);
#41749=AXIS2_PLACEMENT_3D('',#63768,#50161,#50162);
#41750=AXIS2_PLACEMENT_3D('',#63770,#50164,#50165);
#41751=AXIS2_PLACEMENT_3D('',#63772,#50167,#50168);
#41752=AXIS2_PLACEMENT_3D('',#63774,#50170,#50171);
#41753=AXIS2_PLACEMENT_3D('',#63776,#50173,#50174);
#41754=AXIS2_PLACEMENT_3D('',#63777,#50175,#50176);
#41755=AXIS2_PLACEMENT_3D('',#63780,#50179,#50180);
#41756=AXIS2_PLACEMENT_3D('',#63782,#50182,#50183);
#41757=AXIS2_PLACEMENT_3D('',#63784,#50185,#50186);
#41758=AXIS2_PLACEMENT_3D('',#63786,#50188,#50189);
#41759=AXIS2_PLACEMENT_3D('',#63788,#50191,#50192);
#41760=AXIS2_PLACEMENT_3D('',#63789,#50193,#50194);
#41761=AXIS2_PLACEMENT_3D('',#63792,#50197,#50198);
#41762=AXIS2_PLACEMENT_3D('',#63794,#50200,#50201);
#41763=AXIS2_PLACEMENT_3D('',#63796,#50203,#50204);
#41764=AXIS2_PLACEMENT_3D('',#63798,#50206,#50207);
#41765=AXIS2_PLACEMENT_3D('',#63800,#50209,#50210);
#41766=AXIS2_PLACEMENT_3D('',#63801,#50211,#50212);
#41767=AXIS2_PLACEMENT_3D('',#63804,#50215,#50216);
#41768=AXIS2_PLACEMENT_3D('',#63806,#50218,#50219);
#41769=AXIS2_PLACEMENT_3D('',#63808,#50221,#50222);
#41770=AXIS2_PLACEMENT_3D('',#63810,#50224,#50225);
#41771=AXIS2_PLACEMENT_3D('',#63812,#50227,#50228);
#41772=AXIS2_PLACEMENT_3D('',#63813,#50229,#50230);
#41773=AXIS2_PLACEMENT_3D('',#63816,#50233,#50234);
#41774=AXIS2_PLACEMENT_3D('',#63818,#50236,#50237);
#41775=AXIS2_PLACEMENT_3D('',#63820,#50239,#50240);
#41776=AXIS2_PLACEMENT_3D('',#63822,#50242,#50243);
#41777=AXIS2_PLACEMENT_3D('',#63824,#50245,#50246);
#41778=AXIS2_PLACEMENT_3D('',#63825,#50247,#50248);
#41779=AXIS2_PLACEMENT_3D('',#63828,#50251,#50252);
#41780=AXIS2_PLACEMENT_3D('',#63830,#50254,#50255);
#41781=AXIS2_PLACEMENT_3D('',#63832,#50257,#50258);
#41782=AXIS2_PLACEMENT_3D('',#63834,#50260,#50261);
#41783=AXIS2_PLACEMENT_3D('',#63836,#50263,#50264);
#41784=AXIS2_PLACEMENT_3D('',#63837,#50265,#50266);
#41785=AXIS2_PLACEMENT_3D('',#63840,#50269,#50270);
#41786=AXIS2_PLACEMENT_3D('',#63842,#50272,#50273);
#41787=AXIS2_PLACEMENT_3D('',#63844,#50275,#50276);
#41788=AXIS2_PLACEMENT_3D('',#63846,#50278,#50279);
#41789=AXIS2_PLACEMENT_3D('',#63848,#50281,#50282);
#41790=AXIS2_PLACEMENT_3D('',#63849,#50283,#50284);
#41791=AXIS2_PLACEMENT_3D('',#63852,#50287,#50288);
#41792=AXIS2_PLACEMENT_3D('',#63854,#50290,#50291);
#41793=AXIS2_PLACEMENT_3D('',#63856,#50293,#50294);
#41794=AXIS2_PLACEMENT_3D('',#63858,#50296,#50297);
#41795=AXIS2_PLACEMENT_3D('',#63860,#50299,#50300);
#41796=AXIS2_PLACEMENT_3D('',#63861,#50301,#50302);
#41797=AXIS2_PLACEMENT_3D('',#63864,#50305,#50306);
#41798=AXIS2_PLACEMENT_3D('',#63866,#50308,#50309);
#41799=AXIS2_PLACEMENT_3D('',#63868,#50311,#50312);
#41800=AXIS2_PLACEMENT_3D('',#63870,#50314,#50315);
#41801=AXIS2_PLACEMENT_3D('',#63872,#50317,#50318);
#41802=AXIS2_PLACEMENT_3D('',#63873,#50319,#50320);
#41803=AXIS2_PLACEMENT_3D('',#63876,#50323,#50324);
#41804=AXIS2_PLACEMENT_3D('',#63878,#50326,#50327);
#41805=AXIS2_PLACEMENT_3D('',#63880,#50329,#50330);
#41806=AXIS2_PLACEMENT_3D('',#63882,#50332,#50333);
#41807=AXIS2_PLACEMENT_3D('',#63884,#50335,#50336);
#41808=AXIS2_PLACEMENT_3D('',#63885,#50337,#50338);
#41809=AXIS2_PLACEMENT_3D('',#63888,#50341,#50342);
#41810=AXIS2_PLACEMENT_3D('',#63890,#50344,#50345);
#41811=AXIS2_PLACEMENT_3D('',#63892,#50347,#50348);
#41812=AXIS2_PLACEMENT_3D('',#63894,#50350,#50351);
#41813=AXIS2_PLACEMENT_3D('',#63896,#50353,#50354);
#41814=AXIS2_PLACEMENT_3D('',#63897,#50355,#50356);
#41815=AXIS2_PLACEMENT_3D('',#63900,#50359,#50360);
#41816=AXIS2_PLACEMENT_3D('',#63902,#50362,#50363);
#41817=AXIS2_PLACEMENT_3D('',#63904,#50365,#50366);
#41818=AXIS2_PLACEMENT_3D('',#63906,#50368,#50369);
#41819=AXIS2_PLACEMENT_3D('',#63908,#50371,#50372);
#41820=AXIS2_PLACEMENT_3D('',#63909,#50373,#50374);
#41821=AXIS2_PLACEMENT_3D('',#63912,#50377,#50378);
#41822=AXIS2_PLACEMENT_3D('',#63914,#50380,#50381);
#41823=AXIS2_PLACEMENT_3D('',#63916,#50383,#50384);
#41824=AXIS2_PLACEMENT_3D('',#63918,#50386,#50387);
#41825=AXIS2_PLACEMENT_3D('',#63920,#50389,#50390);
#41826=AXIS2_PLACEMENT_3D('',#63921,#50391,#50392);
#41827=AXIS2_PLACEMENT_3D('',#63924,#50395,#50396);
#41828=AXIS2_PLACEMENT_3D('',#63926,#50398,#50399);
#41829=AXIS2_PLACEMENT_3D('',#63928,#50401,#50402);
#41830=AXIS2_PLACEMENT_3D('',#63930,#50404,#50405);
#41831=AXIS2_PLACEMENT_3D('',#63932,#50407,#50408);
#41832=AXIS2_PLACEMENT_3D('',#63933,#50409,#50410);
#41833=AXIS2_PLACEMENT_3D('',#63936,#50413,#50414);
#41834=AXIS2_PLACEMENT_3D('',#63938,#50416,#50417);
#41835=AXIS2_PLACEMENT_3D('',#63940,#50419,#50420);
#41836=AXIS2_PLACEMENT_3D('',#63942,#50422,#50423);
#41837=AXIS2_PLACEMENT_3D('',#63944,#50425,#50426);
#41838=AXIS2_PLACEMENT_3D('',#63945,#50427,#50428);
#41839=AXIS2_PLACEMENT_3D('',#63948,#50431,#50432);
#41840=AXIS2_PLACEMENT_3D('',#63950,#50434,#50435);
#41841=AXIS2_PLACEMENT_3D('',#63952,#50437,#50438);
#41842=AXIS2_PLACEMENT_3D('',#63954,#50440,#50441);
#41843=AXIS2_PLACEMENT_3D('',#63956,#50443,#50444);
#41844=AXIS2_PLACEMENT_3D('',#63957,#50445,#50446);
#41845=AXIS2_PLACEMENT_3D('',#63960,#50449,#50450);
#41846=AXIS2_PLACEMENT_3D('',#63962,#50452,#50453);
#41847=AXIS2_PLACEMENT_3D('',#63964,#50455,#50456);
#41848=AXIS2_PLACEMENT_3D('',#63966,#50458,#50459);
#41849=AXIS2_PLACEMENT_3D('',#63968,#50461,#50462);
#41850=AXIS2_PLACEMENT_3D('',#63969,#50463,#50464);
#41851=AXIS2_PLACEMENT_3D('',#63972,#50467,#50468);
#41852=AXIS2_PLACEMENT_3D('',#63974,#50470,#50471);
#41853=AXIS2_PLACEMENT_3D('',#63976,#50473,#50474);
#41854=AXIS2_PLACEMENT_3D('',#63978,#50476,#50477);
#41855=AXIS2_PLACEMENT_3D('',#63980,#50479,#50480);
#41856=AXIS2_PLACEMENT_3D('',#63981,#50481,#50482);
#41857=AXIS2_PLACEMENT_3D('',#63984,#50485,#50486);
#41858=AXIS2_PLACEMENT_3D('',#63986,#50488,#50489);
#41859=AXIS2_PLACEMENT_3D('',#63988,#50491,#50492);
#41860=AXIS2_PLACEMENT_3D('',#63990,#50494,#50495);
#41861=AXIS2_PLACEMENT_3D('',#63992,#50497,#50498);
#41862=AXIS2_PLACEMENT_3D('',#63993,#50499,#50500);
#41863=AXIS2_PLACEMENT_3D('',#63996,#50503,#50504);
#41864=AXIS2_PLACEMENT_3D('',#63998,#50506,#50507);
#41865=AXIS2_PLACEMENT_3D('',#64000,#50509,#50510);
#41866=AXIS2_PLACEMENT_3D('',#64002,#50512,#50513);
#41867=AXIS2_PLACEMENT_3D('',#64004,#50515,#50516);
#41868=AXIS2_PLACEMENT_3D('',#64005,#50517,#50518);
#41869=AXIS2_PLACEMENT_3D('',#64008,#50521,#50522);
#41870=AXIS2_PLACEMENT_3D('',#64010,#50524,#50525);
#41871=AXIS2_PLACEMENT_3D('',#64012,#50527,#50528);
#41872=AXIS2_PLACEMENT_3D('',#64014,#50530,#50531);
#41873=AXIS2_PLACEMENT_3D('',#64016,#50533,#50534);
#41874=AXIS2_PLACEMENT_3D('',#64017,#50535,#50536);
#41875=AXIS2_PLACEMENT_3D('',#64020,#50539,#50540);
#41876=AXIS2_PLACEMENT_3D('',#64022,#50542,#50543);
#41877=AXIS2_PLACEMENT_3D('',#64024,#50545,#50546);
#41878=AXIS2_PLACEMENT_3D('',#64026,#50548,#50549);
#41879=AXIS2_PLACEMENT_3D('',#64028,#50551,#50552);
#41880=AXIS2_PLACEMENT_3D('',#64029,#50553,#50554);
#41881=AXIS2_PLACEMENT_3D('',#64032,#50557,#50558);
#41882=AXIS2_PLACEMENT_3D('',#64034,#50560,#50561);
#41883=AXIS2_PLACEMENT_3D('',#64036,#50563,#50564);
#41884=AXIS2_PLACEMENT_3D('',#64038,#50566,#50567);
#41885=AXIS2_PLACEMENT_3D('',#64040,#50569,#50570);
#41886=AXIS2_PLACEMENT_3D('',#64041,#50571,#50572);
#41887=AXIS2_PLACEMENT_3D('',#64044,#50575,#50576);
#41888=AXIS2_PLACEMENT_3D('',#64046,#50578,#50579);
#41889=AXIS2_PLACEMENT_3D('',#64048,#50581,#50582);
#41890=AXIS2_PLACEMENT_3D('',#64050,#50584,#50585);
#41891=AXIS2_PLACEMENT_3D('',#64052,#50587,#50588);
#41892=AXIS2_PLACEMENT_3D('',#64053,#50589,#50590);
#41893=AXIS2_PLACEMENT_3D('',#64056,#50593,#50594);
#41894=AXIS2_PLACEMENT_3D('',#64058,#50596,#50597);
#41895=AXIS2_PLACEMENT_3D('',#64060,#50599,#50600);
#41896=AXIS2_PLACEMENT_3D('',#64062,#50602,#50603);
#41897=AXIS2_PLACEMENT_3D('',#64064,#50605,#50606);
#41898=AXIS2_PLACEMENT_3D('',#64065,#50607,#50608);
#41899=AXIS2_PLACEMENT_3D('',#64068,#50611,#50612);
#41900=AXIS2_PLACEMENT_3D('',#64070,#50614,#50615);
#41901=AXIS2_PLACEMENT_3D('',#64072,#50617,#50618);
#41902=AXIS2_PLACEMENT_3D('',#64074,#50620,#50621);
#41903=AXIS2_PLACEMENT_3D('',#64076,#50623,#50624);
#41904=AXIS2_PLACEMENT_3D('',#64077,#50625,#50626);
#41905=AXIS2_PLACEMENT_3D('',#64080,#50629,#50630);
#41906=AXIS2_PLACEMENT_3D('',#64082,#50632,#50633);
#41907=AXIS2_PLACEMENT_3D('',#64084,#50635,#50636);
#41908=AXIS2_PLACEMENT_3D('',#64086,#50638,#50639);
#41909=AXIS2_PLACEMENT_3D('',#64088,#50641,#50642);
#41910=AXIS2_PLACEMENT_3D('',#64089,#50643,#50644);
#41911=AXIS2_PLACEMENT_3D('',#64092,#50647,#50648);
#41912=AXIS2_PLACEMENT_3D('',#64094,#50650,#50651);
#41913=AXIS2_PLACEMENT_3D('',#64096,#50653,#50654);
#41914=AXIS2_PLACEMENT_3D('',#64098,#50656,#50657);
#41915=AXIS2_PLACEMENT_3D('',#64100,#50659,#50660);
#41916=AXIS2_PLACEMENT_3D('',#64101,#50661,#50662);
#41917=AXIS2_PLACEMENT_3D('',#64104,#50665,#50666);
#41918=AXIS2_PLACEMENT_3D('',#64106,#50668,#50669);
#41919=AXIS2_PLACEMENT_3D('',#64108,#50671,#50672);
#41920=AXIS2_PLACEMENT_3D('',#64110,#50674,#50675);
#41921=AXIS2_PLACEMENT_3D('',#64112,#50677,#50678);
#41922=AXIS2_PLACEMENT_3D('',#64113,#50679,#50680);
#41923=AXIS2_PLACEMENT_3D('',#64116,#50683,#50684);
#41924=AXIS2_PLACEMENT_3D('',#64118,#50686,#50687);
#41925=AXIS2_PLACEMENT_3D('',#64120,#50689,#50690);
#41926=AXIS2_PLACEMENT_3D('',#64122,#50692,#50693);
#41927=AXIS2_PLACEMENT_3D('',#64124,#50695,#50696);
#41928=AXIS2_PLACEMENT_3D('',#64125,#50697,#50698);
#41929=AXIS2_PLACEMENT_3D('',#64128,#50701,#50702);
#41930=AXIS2_PLACEMENT_3D('',#64130,#50704,#50705);
#41931=AXIS2_PLACEMENT_3D('',#64132,#50707,#50708);
#41932=AXIS2_PLACEMENT_3D('',#64134,#50710,#50711);
#41933=AXIS2_PLACEMENT_3D('',#64136,#50713,#50714);
#41934=AXIS2_PLACEMENT_3D('',#64137,#50715,#50716);
#41935=AXIS2_PLACEMENT_3D('',#64140,#50719,#50720);
#41936=AXIS2_PLACEMENT_3D('',#64142,#50722,#50723);
#41937=AXIS2_PLACEMENT_3D('',#64144,#50725,#50726);
#41938=AXIS2_PLACEMENT_3D('',#64146,#50728,#50729);
#41939=AXIS2_PLACEMENT_3D('',#64148,#50731,#50732);
#41940=AXIS2_PLACEMENT_3D('',#64149,#50733,#50734);
#41941=AXIS2_PLACEMENT_3D('',#64152,#50737,#50738);
#41942=AXIS2_PLACEMENT_3D('',#64154,#50740,#50741);
#41943=AXIS2_PLACEMENT_3D('',#64156,#50743,#50744);
#41944=AXIS2_PLACEMENT_3D('',#64158,#50746,#50747);
#41945=AXIS2_PLACEMENT_3D('',#64160,#50749,#50750);
#41946=AXIS2_PLACEMENT_3D('',#64161,#50751,#50752);
#41947=AXIS2_PLACEMENT_3D('',#64164,#50755,#50756);
#41948=AXIS2_PLACEMENT_3D('',#64166,#50758,#50759);
#41949=AXIS2_PLACEMENT_3D('',#64168,#50761,#50762);
#41950=AXIS2_PLACEMENT_3D('',#64170,#50764,#50765);
#41951=AXIS2_PLACEMENT_3D('',#64172,#50767,#50768);
#41952=AXIS2_PLACEMENT_3D('',#64173,#50769,#50770);
#41953=AXIS2_PLACEMENT_3D('',#64176,#50773,#50774);
#41954=AXIS2_PLACEMENT_3D('',#64178,#50776,#50777);
#41955=AXIS2_PLACEMENT_3D('',#64180,#50779,#50780);
#41956=AXIS2_PLACEMENT_3D('',#64182,#50782,#50783);
#41957=AXIS2_PLACEMENT_3D('',#64184,#50785,#50786);
#41958=AXIS2_PLACEMENT_3D('',#64185,#50787,#50788);
#41959=AXIS2_PLACEMENT_3D('',#64188,#50791,#50792);
#41960=AXIS2_PLACEMENT_3D('',#64190,#50794,#50795);
#41961=AXIS2_PLACEMENT_3D('',#64192,#50797,#50798);
#41962=AXIS2_PLACEMENT_3D('',#64194,#50800,#50801);
#41963=AXIS2_PLACEMENT_3D('',#64196,#50803,#50804);
#41964=AXIS2_PLACEMENT_3D('',#64197,#50805,#50806);
#41965=AXIS2_PLACEMENT_3D('',#64200,#50809,#50810);
#41966=AXIS2_PLACEMENT_3D('',#64202,#50812,#50813);
#41967=AXIS2_PLACEMENT_3D('',#64204,#50815,#50816);
#41968=AXIS2_PLACEMENT_3D('',#64206,#50818,#50819);
#41969=AXIS2_PLACEMENT_3D('',#64208,#50821,#50822);
#41970=AXIS2_PLACEMENT_3D('',#64209,#50823,#50824);
#41971=AXIS2_PLACEMENT_3D('',#64212,#50827,#50828);
#41972=AXIS2_PLACEMENT_3D('',#64214,#50830,#50831);
#41973=AXIS2_PLACEMENT_3D('',#64216,#50833,#50834);
#41974=AXIS2_PLACEMENT_3D('',#64218,#50836,#50837);
#41975=AXIS2_PLACEMENT_3D('',#64220,#50839,#50840);
#41976=AXIS2_PLACEMENT_3D('',#64221,#50841,#50842);
#41977=AXIS2_PLACEMENT_3D('',#64224,#50845,#50846);
#41978=AXIS2_PLACEMENT_3D('',#64226,#50848,#50849);
#41979=AXIS2_PLACEMENT_3D('',#64228,#50851,#50852);
#41980=AXIS2_PLACEMENT_3D('',#64230,#50854,#50855);
#41981=AXIS2_PLACEMENT_3D('',#64232,#50857,#50858);
#41982=AXIS2_PLACEMENT_3D('',#64233,#50859,#50860);
#41983=AXIS2_PLACEMENT_3D('',#64236,#50863,#50864);
#41984=AXIS2_PLACEMENT_3D('',#64238,#50866,#50867);
#41985=AXIS2_PLACEMENT_3D('',#64240,#50869,#50870);
#41986=AXIS2_PLACEMENT_3D('',#64242,#50872,#50873);
#41987=AXIS2_PLACEMENT_3D('',#64244,#50875,#50876);
#41988=AXIS2_PLACEMENT_3D('',#64245,#50877,#50878);
#41989=AXIS2_PLACEMENT_3D('',#64248,#50881,#50882);
#41990=AXIS2_PLACEMENT_3D('',#64250,#50884,#50885);
#41991=AXIS2_PLACEMENT_3D('',#64252,#50887,#50888);
#41992=AXIS2_PLACEMENT_3D('',#64254,#50890,#50891);
#41993=AXIS2_PLACEMENT_3D('',#64256,#50893,#50894);
#41994=AXIS2_PLACEMENT_3D('',#64257,#50895,#50896);
#41995=AXIS2_PLACEMENT_3D('',#64260,#50899,#50900);
#41996=AXIS2_PLACEMENT_3D('',#64262,#50902,#50903);
#41997=AXIS2_PLACEMENT_3D('',#64264,#50905,#50906);
#41998=AXIS2_PLACEMENT_3D('',#64266,#50908,#50909);
#41999=AXIS2_PLACEMENT_3D('',#64268,#50911,#50912);
#42000=AXIS2_PLACEMENT_3D('',#64269,#50913,#50914);
#42001=AXIS2_PLACEMENT_3D('',#64272,#50917,#50918);
#42002=AXIS2_PLACEMENT_3D('',#64274,#50920,#50921);
#42003=AXIS2_PLACEMENT_3D('',#64276,#50923,#50924);
#42004=AXIS2_PLACEMENT_3D('',#64278,#50926,#50927);
#42005=AXIS2_PLACEMENT_3D('',#64280,#50929,#50930);
#42006=AXIS2_PLACEMENT_3D('',#64281,#50931,#50932);
#42007=AXIS2_PLACEMENT_3D('',#64284,#50935,#50936);
#42008=AXIS2_PLACEMENT_3D('',#64286,#50938,#50939);
#42009=AXIS2_PLACEMENT_3D('',#64288,#50941,#50942);
#42010=AXIS2_PLACEMENT_3D('',#64290,#50944,#50945);
#42011=AXIS2_PLACEMENT_3D('',#64292,#50947,#50948);
#42012=AXIS2_PLACEMENT_3D('',#64293,#50949,#50950);
#42013=AXIS2_PLACEMENT_3D('',#64296,#50953,#50954);
#42014=AXIS2_PLACEMENT_3D('',#64298,#50956,#50957);
#42015=AXIS2_PLACEMENT_3D('',#64300,#50959,#50960);
#42016=AXIS2_PLACEMENT_3D('',#64302,#50962,#50963);
#42017=AXIS2_PLACEMENT_3D('',#64304,#50965,#50966);
#42018=AXIS2_PLACEMENT_3D('',#64305,#50967,#50968);
#42019=AXIS2_PLACEMENT_3D('',#64308,#50971,#50972);
#42020=AXIS2_PLACEMENT_3D('',#64310,#50974,#50975);
#42021=AXIS2_PLACEMENT_3D('',#64312,#50977,#50978);
#42022=AXIS2_PLACEMENT_3D('',#64314,#50980,#50981);
#42023=AXIS2_PLACEMENT_3D('',#64316,#50983,#50984);
#42024=AXIS2_PLACEMENT_3D('',#64317,#50985,#50986);
#42025=AXIS2_PLACEMENT_3D('',#64320,#50989,#50990);
#42026=AXIS2_PLACEMENT_3D('',#64322,#50992,#50993);
#42027=AXIS2_PLACEMENT_3D('',#64324,#50995,#50996);
#42028=AXIS2_PLACEMENT_3D('',#64326,#50998,#50999);
#42029=AXIS2_PLACEMENT_3D('',#64328,#51001,#51002);
#42030=AXIS2_PLACEMENT_3D('',#64329,#51003,#51004);
#42031=AXIS2_PLACEMENT_3D('',#64332,#51007,#51008);
#42032=AXIS2_PLACEMENT_3D('',#64334,#51010,#51011);
#42033=AXIS2_PLACEMENT_3D('',#64336,#51013,#51014);
#42034=AXIS2_PLACEMENT_3D('',#64338,#51016,#51017);
#42035=AXIS2_PLACEMENT_3D('',#64340,#51019,#51020);
#42036=AXIS2_PLACEMENT_3D('',#64341,#51021,#51022);
#42037=AXIS2_PLACEMENT_3D('',#64344,#51025,#51026);
#42038=AXIS2_PLACEMENT_3D('',#64346,#51028,#51029);
#42039=AXIS2_PLACEMENT_3D('',#64348,#51031,#51032);
#42040=AXIS2_PLACEMENT_3D('',#64350,#51034,#51035);
#42041=AXIS2_PLACEMENT_3D('',#64352,#51037,#51038);
#42042=AXIS2_PLACEMENT_3D('',#64353,#51039,#51040);
#42043=AXIS2_PLACEMENT_3D('',#64356,#51043,#51044);
#42044=AXIS2_PLACEMENT_3D('',#64358,#51046,#51047);
#42045=AXIS2_PLACEMENT_3D('',#64360,#51049,#51050);
#42046=AXIS2_PLACEMENT_3D('',#64362,#51052,#51053);
#42047=AXIS2_PLACEMENT_3D('',#64364,#51055,#51056);
#42048=AXIS2_PLACEMENT_3D('',#64365,#51057,#51058);
#42049=AXIS2_PLACEMENT_3D('',#64368,#51061,#51062);
#42050=AXIS2_PLACEMENT_3D('',#64370,#51064,#51065);
#42051=AXIS2_PLACEMENT_3D('',#64372,#51067,#51068);
#42052=AXIS2_PLACEMENT_3D('',#64374,#51070,#51071);
#42053=AXIS2_PLACEMENT_3D('',#64376,#51073,#51074);
#42054=AXIS2_PLACEMENT_3D('',#64377,#51075,#51076);
#42055=AXIS2_PLACEMENT_3D('',#64380,#51079,#51080);
#42056=AXIS2_PLACEMENT_3D('',#64382,#51082,#51083);
#42057=AXIS2_PLACEMENT_3D('',#64384,#51085,#51086);
#42058=AXIS2_PLACEMENT_3D('',#64386,#51088,#51089);
#42059=AXIS2_PLACEMENT_3D('',#64388,#51091,#51092);
#42060=AXIS2_PLACEMENT_3D('',#64389,#51093,#51094);
#42061=AXIS2_PLACEMENT_3D('',#64392,#51097,#51098);
#42062=AXIS2_PLACEMENT_3D('',#64394,#51100,#51101);
#42063=AXIS2_PLACEMENT_3D('',#64396,#51103,#51104);
#42064=AXIS2_PLACEMENT_3D('',#64398,#51106,#51107);
#42065=AXIS2_PLACEMENT_3D('',#64400,#51109,#51110);
#42066=AXIS2_PLACEMENT_3D('',#64401,#51111,#51112);
#42067=AXIS2_PLACEMENT_3D('',#64404,#51115,#51116);
#42068=AXIS2_PLACEMENT_3D('',#64406,#51118,#51119);
#42069=AXIS2_PLACEMENT_3D('',#64408,#51121,#51122);
#42070=AXIS2_PLACEMENT_3D('',#64410,#51124,#51125);
#42071=AXIS2_PLACEMENT_3D('',#64412,#51127,#51128);
#42072=AXIS2_PLACEMENT_3D('',#64413,#51129,#51130);
#42073=AXIS2_PLACEMENT_3D('',#64416,#51133,#51134);
#42074=AXIS2_PLACEMENT_3D('',#64418,#51136,#51137);
#42075=AXIS2_PLACEMENT_3D('',#64420,#51139,#51140);
#42076=AXIS2_PLACEMENT_3D('',#64422,#51142,#51143);
#42077=AXIS2_PLACEMENT_3D('',#64424,#51145,#51146);
#42078=AXIS2_PLACEMENT_3D('',#64425,#51147,#51148);
#42079=AXIS2_PLACEMENT_3D('',#64428,#51151,#51152);
#42080=AXIS2_PLACEMENT_3D('',#64430,#51154,#51155);
#42081=AXIS2_PLACEMENT_3D('',#64432,#51157,#51158);
#42082=AXIS2_PLACEMENT_3D('',#64434,#51160,#51161);
#42083=AXIS2_PLACEMENT_3D('',#64436,#51163,#51164);
#42084=AXIS2_PLACEMENT_3D('',#64437,#51165,#51166);
#42085=AXIS2_PLACEMENT_3D('',#64440,#51169,#51170);
#42086=AXIS2_PLACEMENT_3D('',#64442,#51172,#51173);
#42087=AXIS2_PLACEMENT_3D('',#64444,#51175,#51176);
#42088=AXIS2_PLACEMENT_3D('',#64446,#51178,#51179);
#42089=AXIS2_PLACEMENT_3D('',#64448,#51181,#51182);
#42090=AXIS2_PLACEMENT_3D('',#64449,#51183,#51184);
#42091=AXIS2_PLACEMENT_3D('',#64452,#51187,#51188);
#42092=AXIS2_PLACEMENT_3D('',#64454,#51190,#51191);
#42093=AXIS2_PLACEMENT_3D('',#64456,#51193,#51194);
#42094=AXIS2_PLACEMENT_3D('',#64458,#51196,#51197);
#42095=AXIS2_PLACEMENT_3D('',#64460,#51199,#51200);
#42096=AXIS2_PLACEMENT_3D('',#64461,#51201,#51202);
#42097=AXIS2_PLACEMENT_3D('',#64464,#51205,#51206);
#42098=AXIS2_PLACEMENT_3D('',#64466,#51208,#51209);
#42099=AXIS2_PLACEMENT_3D('',#64468,#51211,#51212);
#42100=AXIS2_PLACEMENT_3D('',#64470,#51214,#51215);
#42101=AXIS2_PLACEMENT_3D('',#64472,#51217,#51218);
#42102=AXIS2_PLACEMENT_3D('',#64473,#51219,#51220);
#42103=AXIS2_PLACEMENT_3D('',#64476,#51223,#51224);
#42104=AXIS2_PLACEMENT_3D('',#64478,#51226,#51227);
#42105=AXIS2_PLACEMENT_3D('',#64480,#51229,#51230);
#42106=AXIS2_PLACEMENT_3D('',#64482,#51232,#51233);
#42107=AXIS2_PLACEMENT_3D('',#64484,#51235,#51236);
#42108=AXIS2_PLACEMENT_3D('',#64485,#51237,#51238);
#42109=AXIS2_PLACEMENT_3D('',#64488,#51241,#51242);
#42110=AXIS2_PLACEMENT_3D('',#64490,#51244,#51245);
#42111=AXIS2_PLACEMENT_3D('',#64492,#51247,#51248);
#42112=AXIS2_PLACEMENT_3D('',#64494,#51250,#51251);
#42113=AXIS2_PLACEMENT_3D('',#64496,#51253,#51254);
#42114=AXIS2_PLACEMENT_3D('',#64497,#51255,#51256);
#42115=AXIS2_PLACEMENT_3D('',#64500,#51259,#51260);
#42116=AXIS2_PLACEMENT_3D('',#64502,#51262,#51263);
#42117=AXIS2_PLACEMENT_3D('',#64504,#51265,#51266);
#42118=AXIS2_PLACEMENT_3D('',#64506,#51268,#51269);
#42119=AXIS2_PLACEMENT_3D('',#64508,#51271,#51272);
#42120=AXIS2_PLACEMENT_3D('',#64509,#51273,#51274);
#42121=AXIS2_PLACEMENT_3D('',#64512,#51277,#51278);
#42122=AXIS2_PLACEMENT_3D('',#64514,#51280,#51281);
#42123=AXIS2_PLACEMENT_3D('',#64516,#51283,#51284);
#42124=AXIS2_PLACEMENT_3D('',#64518,#51286,#51287);
#42125=AXIS2_PLACEMENT_3D('',#64520,#51289,#51290);
#42126=AXIS2_PLACEMENT_3D('',#64521,#51291,#51292);
#42127=AXIS2_PLACEMENT_3D('',#64524,#51295,#51296);
#42128=AXIS2_PLACEMENT_3D('',#64526,#51298,#51299);
#42129=AXIS2_PLACEMENT_3D('',#64528,#51301,#51302);
#42130=AXIS2_PLACEMENT_3D('',#64530,#51304,#51305);
#42131=AXIS2_PLACEMENT_3D('',#64532,#51307,#51308);
#42132=AXIS2_PLACEMENT_3D('',#64533,#51309,#51310);
#42133=AXIS2_PLACEMENT_3D('',#64536,#51313,#51314);
#42134=AXIS2_PLACEMENT_3D('',#64538,#51316,#51317);
#42135=AXIS2_PLACEMENT_3D('',#64540,#51319,#51320);
#42136=AXIS2_PLACEMENT_3D('',#64542,#51322,#51323);
#42137=AXIS2_PLACEMENT_3D('',#64544,#51325,#51326);
#42138=AXIS2_PLACEMENT_3D('',#64545,#51327,#51328);
#42139=AXIS2_PLACEMENT_3D('',#64548,#51331,#51332);
#42140=AXIS2_PLACEMENT_3D('',#64550,#51334,#51335);
#42141=AXIS2_PLACEMENT_3D('',#64552,#51337,#51338);
#42142=AXIS2_PLACEMENT_3D('',#64554,#51340,#51341);
#42143=AXIS2_PLACEMENT_3D('',#64556,#51343,#51344);
#42144=AXIS2_PLACEMENT_3D('',#64557,#51345,#51346);
#42145=AXIS2_PLACEMENT_3D('',#64560,#51349,#51350);
#42146=AXIS2_PLACEMENT_3D('',#64562,#51352,#51353);
#42147=AXIS2_PLACEMENT_3D('',#64564,#51355,#51356);
#42148=AXIS2_PLACEMENT_3D('',#64566,#51358,#51359);
#42149=AXIS2_PLACEMENT_3D('',#64568,#51361,#51362);
#42150=AXIS2_PLACEMENT_3D('',#64569,#51363,#51364);
#42151=AXIS2_PLACEMENT_3D('',#64572,#51367,#51368);
#42152=AXIS2_PLACEMENT_3D('',#64574,#51370,#51371);
#42153=AXIS2_PLACEMENT_3D('',#64576,#51373,#51374);
#42154=AXIS2_PLACEMENT_3D('',#64578,#51376,#51377);
#42155=AXIS2_PLACEMENT_3D('',#64580,#51379,#51380);
#42156=AXIS2_PLACEMENT_3D('',#64581,#51381,#51382);
#42157=AXIS2_PLACEMENT_3D('',#64584,#51385,#51386);
#42158=AXIS2_PLACEMENT_3D('',#64586,#51388,#51389);
#42159=AXIS2_PLACEMENT_3D('',#64588,#51391,#51392);
#42160=AXIS2_PLACEMENT_3D('',#64590,#51394,#51395);
#42161=AXIS2_PLACEMENT_3D('',#64592,#51397,#51398);
#42162=AXIS2_PLACEMENT_3D('',#64593,#51399,#51400);
#42163=AXIS2_PLACEMENT_3D('',#64596,#51403,#51404);
#42164=AXIS2_PLACEMENT_3D('',#64598,#51406,#51407);
#42165=AXIS2_PLACEMENT_3D('',#64600,#51409,#51410);
#42166=AXIS2_PLACEMENT_3D('',#64602,#51412,#51413);
#42167=AXIS2_PLACEMENT_3D('',#64604,#51415,#51416);
#42168=AXIS2_PLACEMENT_3D('',#64605,#51417,#51418);
#42169=AXIS2_PLACEMENT_3D('',#64608,#51421,#51422);
#42170=AXIS2_PLACEMENT_3D('',#64610,#51424,#51425);
#42171=AXIS2_PLACEMENT_3D('',#64612,#51427,#51428);
#42172=AXIS2_PLACEMENT_3D('',#64614,#51430,#51431);
#42173=AXIS2_PLACEMENT_3D('',#64616,#51433,#51434);
#42174=AXIS2_PLACEMENT_3D('',#64617,#51435,#51436);
#42175=AXIS2_PLACEMENT_3D('',#64620,#51439,#51440);
#42176=AXIS2_PLACEMENT_3D('',#64622,#51442,#51443);
#42177=AXIS2_PLACEMENT_3D('',#64624,#51445,#51446);
#42178=AXIS2_PLACEMENT_3D('',#64626,#51448,#51449);
#42179=AXIS2_PLACEMENT_3D('',#64628,#51451,#51452);
#42180=AXIS2_PLACEMENT_3D('',#64629,#51453,#51454);
#42181=AXIS2_PLACEMENT_3D('',#64632,#51457,#51458);
#42182=AXIS2_PLACEMENT_3D('',#64634,#51460,#51461);
#42183=AXIS2_PLACEMENT_3D('',#64636,#51463,#51464);
#42184=AXIS2_PLACEMENT_3D('',#64638,#51466,#51467);
#42185=AXIS2_PLACEMENT_3D('',#64640,#51469,#51470);
#42186=AXIS2_PLACEMENT_3D('',#64641,#51471,#51472);
#42187=AXIS2_PLACEMENT_3D('',#64644,#51475,#51476);
#42188=AXIS2_PLACEMENT_3D('',#64646,#51478,#51479);
#42189=AXIS2_PLACEMENT_3D('',#64648,#51481,#51482);
#42190=AXIS2_PLACEMENT_3D('',#64650,#51484,#51485);
#42191=AXIS2_PLACEMENT_3D('',#64652,#51487,#51488);
#42192=AXIS2_PLACEMENT_3D('',#64653,#51489,#51490);
#42193=AXIS2_PLACEMENT_3D('',#64656,#51493,#51494);
#42194=AXIS2_PLACEMENT_3D('',#64658,#51496,#51497);
#42195=AXIS2_PLACEMENT_3D('',#64660,#51499,#51500);
#42196=AXIS2_PLACEMENT_3D('',#64662,#51502,#51503);
#42197=AXIS2_PLACEMENT_3D('',#64664,#51505,#51506);
#42198=AXIS2_PLACEMENT_3D('',#64665,#51507,#51508);
#42199=AXIS2_PLACEMENT_3D('',#64668,#51511,#51512);
#42200=AXIS2_PLACEMENT_3D('',#64670,#51514,#51515);
#42201=AXIS2_PLACEMENT_3D('',#64672,#51517,#51518);
#42202=AXIS2_PLACEMENT_3D('',#64674,#51520,#51521);
#42203=AXIS2_PLACEMENT_3D('',#64676,#51523,#51524);
#42204=AXIS2_PLACEMENT_3D('',#64677,#51525,#51526);
#42205=AXIS2_PLACEMENT_3D('',#64680,#51529,#51530);
#42206=AXIS2_PLACEMENT_3D('',#64682,#51532,#51533);
#42207=AXIS2_PLACEMENT_3D('',#64684,#51535,#51536);
#42208=AXIS2_PLACEMENT_3D('',#64686,#51538,#51539);
#42209=AXIS2_PLACEMENT_3D('',#64688,#51541,#51542);
#42210=AXIS2_PLACEMENT_3D('',#64689,#51543,#51544);
#42211=AXIS2_PLACEMENT_3D('',#64692,#51547,#51548);
#42212=AXIS2_PLACEMENT_3D('',#64694,#51550,#51551);
#42213=AXIS2_PLACEMENT_3D('',#64696,#51553,#51554);
#42214=AXIS2_PLACEMENT_3D('',#64698,#51556,#51557);
#42215=AXIS2_PLACEMENT_3D('',#64700,#51559,#51560);
#42216=AXIS2_PLACEMENT_3D('',#64701,#51561,#51562);
#42217=AXIS2_PLACEMENT_3D('',#64704,#51565,#51566);
#42218=AXIS2_PLACEMENT_3D('',#64706,#51568,#51569);
#42219=AXIS2_PLACEMENT_3D('',#64708,#51571,#51572);
#42220=AXIS2_PLACEMENT_3D('',#64710,#51574,#51575);
#42221=AXIS2_PLACEMENT_3D('',#64712,#51577,#51578);
#42222=AXIS2_PLACEMENT_3D('',#64713,#51579,#51580);
#42223=AXIS2_PLACEMENT_3D('',#64716,#51583,#51584);
#42224=AXIS2_PLACEMENT_3D('',#64718,#51586,#51587);
#42225=AXIS2_PLACEMENT_3D('',#64720,#51589,#51590);
#42226=AXIS2_PLACEMENT_3D('',#64722,#51592,#51593);
#42227=AXIS2_PLACEMENT_3D('',#64724,#51595,#51596);
#42228=AXIS2_PLACEMENT_3D('',#64725,#51597,#51598);
#42229=AXIS2_PLACEMENT_3D('',#64728,#51601,#51602);
#42230=AXIS2_PLACEMENT_3D('',#64730,#51604,#51605);
#42231=AXIS2_PLACEMENT_3D('',#64732,#51607,#51608);
#42232=AXIS2_PLACEMENT_3D('',#64734,#51610,#51611);
#42233=AXIS2_PLACEMENT_3D('',#64736,#51613,#51614);
#42234=AXIS2_PLACEMENT_3D('',#64737,#51615,#51616);
#42235=AXIS2_PLACEMENT_3D('',#64740,#51619,#51620);
#42236=AXIS2_PLACEMENT_3D('',#64742,#51622,#51623);
#42237=AXIS2_PLACEMENT_3D('',#64744,#51625,#51626);
#42238=AXIS2_PLACEMENT_3D('',#64746,#51628,#51629);
#42239=AXIS2_PLACEMENT_3D('',#64748,#51631,#51632);
#42240=AXIS2_PLACEMENT_3D('',#64749,#51633,#51634);
#42241=AXIS2_PLACEMENT_3D('',#64752,#51637,#51638);
#42242=AXIS2_PLACEMENT_3D('',#64754,#51640,#51641);
#42243=AXIS2_PLACEMENT_3D('',#64756,#51643,#51644);
#42244=AXIS2_PLACEMENT_3D('',#64758,#51646,#51647);
#42245=AXIS2_PLACEMENT_3D('',#64760,#51649,#51650);
#42246=AXIS2_PLACEMENT_3D('',#64761,#51651,#51652);
#42247=AXIS2_PLACEMENT_3D('',#64764,#51655,#51656);
#42248=AXIS2_PLACEMENT_3D('',#64766,#51658,#51659);
#42249=AXIS2_PLACEMENT_3D('',#64768,#51661,#51662);
#42250=AXIS2_PLACEMENT_3D('',#64770,#51664,#51665);
#42251=AXIS2_PLACEMENT_3D('',#64772,#51667,#51668);
#42252=AXIS2_PLACEMENT_3D('',#64773,#51669,#51670);
#42253=AXIS2_PLACEMENT_3D('',#64776,#51673,#51674);
#42254=AXIS2_PLACEMENT_3D('',#64778,#51676,#51677);
#42255=AXIS2_PLACEMENT_3D('',#64780,#51679,#51680);
#42256=AXIS2_PLACEMENT_3D('',#64782,#51682,#51683);
#42257=AXIS2_PLACEMENT_3D('',#64784,#51685,#51686);
#42258=AXIS2_PLACEMENT_3D('',#64785,#51687,#51688);
#42259=AXIS2_PLACEMENT_3D('',#64788,#51691,#51692);
#42260=AXIS2_PLACEMENT_3D('',#64790,#51694,#51695);
#42261=AXIS2_PLACEMENT_3D('',#64792,#51697,#51698);
#42262=AXIS2_PLACEMENT_3D('',#64794,#51700,#51701);
#42263=AXIS2_PLACEMENT_3D('',#64796,#51703,#51704);
#42264=AXIS2_PLACEMENT_3D('',#64797,#51705,#51706);
#42265=AXIS2_PLACEMENT_3D('',#64800,#51709,#51710);
#42266=AXIS2_PLACEMENT_3D('',#64802,#51712,#51713);
#42267=AXIS2_PLACEMENT_3D('',#64804,#51715,#51716);
#42268=AXIS2_PLACEMENT_3D('',#64806,#51718,#51719);
#42269=AXIS2_PLACEMENT_3D('',#64808,#51721,#51722);
#42270=AXIS2_PLACEMENT_3D('',#64809,#51723,#51724);
#42271=AXIS2_PLACEMENT_3D('',#64812,#51727,#51728);
#42272=AXIS2_PLACEMENT_3D('',#64814,#51730,#51731);
#42273=AXIS2_PLACEMENT_3D('',#64816,#51733,#51734);
#42274=AXIS2_PLACEMENT_3D('',#64818,#51736,#51737);
#42275=AXIS2_PLACEMENT_3D('',#64820,#51739,#51740);
#42276=AXIS2_PLACEMENT_3D('',#64821,#51741,#51742);
#42277=AXIS2_PLACEMENT_3D('',#64824,#51745,#51746);
#42278=AXIS2_PLACEMENT_3D('',#64826,#51748,#51749);
#42279=AXIS2_PLACEMENT_3D('',#64828,#51751,#51752);
#42280=AXIS2_PLACEMENT_3D('',#64830,#51754,#51755);
#42281=AXIS2_PLACEMENT_3D('',#64832,#51757,#51758);
#42282=AXIS2_PLACEMENT_3D('',#64833,#51759,#51760);
#42283=AXIS2_PLACEMENT_3D('',#64836,#51763,#51764);
#42284=AXIS2_PLACEMENT_3D('',#64838,#51766,#51767);
#42285=AXIS2_PLACEMENT_3D('',#64840,#51769,#51770);
#42286=AXIS2_PLACEMENT_3D('',#64842,#51772,#51773);
#42287=AXIS2_PLACEMENT_3D('',#64844,#51775,#51776);
#42288=AXIS2_PLACEMENT_3D('',#64845,#51777,#51778);
#42289=AXIS2_PLACEMENT_3D('',#64848,#51781,#51782);
#42290=AXIS2_PLACEMENT_3D('',#64850,#51784,#51785);
#42291=AXIS2_PLACEMENT_3D('',#64852,#51787,#51788);
#42292=AXIS2_PLACEMENT_3D('',#64854,#51790,#51791);
#42293=AXIS2_PLACEMENT_3D('',#64856,#51793,#51794);
#42294=AXIS2_PLACEMENT_3D('',#64857,#51795,#51796);
#42295=AXIS2_PLACEMENT_3D('',#64860,#51799,#51800);
#42296=AXIS2_PLACEMENT_3D('',#64862,#51802,#51803);
#42297=AXIS2_PLACEMENT_3D('',#64864,#51805,#51806);
#42298=AXIS2_PLACEMENT_3D('',#64866,#51808,#51809);
#42299=AXIS2_PLACEMENT_3D('',#64868,#51811,#51812);
#42300=AXIS2_PLACEMENT_3D('',#64869,#51813,#51814);
#42301=AXIS2_PLACEMENT_3D('',#64872,#51817,#51818);
#42302=AXIS2_PLACEMENT_3D('',#64874,#51820,#51821);
#42303=AXIS2_PLACEMENT_3D('',#64876,#51823,#51824);
#42304=AXIS2_PLACEMENT_3D('',#64878,#51826,#51827);
#42305=AXIS2_PLACEMENT_3D('',#64880,#51829,#51830);
#42306=AXIS2_PLACEMENT_3D('',#64881,#51831,#51832);
#42307=AXIS2_PLACEMENT_3D('',#64884,#51835,#51836);
#42308=AXIS2_PLACEMENT_3D('',#64886,#51838,#51839);
#42309=AXIS2_PLACEMENT_3D('',#64888,#51841,#51842);
#42310=AXIS2_PLACEMENT_3D('',#64890,#51844,#51845);
#42311=AXIS2_PLACEMENT_3D('',#64892,#51847,#51848);
#42312=AXIS2_PLACEMENT_3D('',#64893,#51849,#51850);
#42313=AXIS2_PLACEMENT_3D('',#64896,#51853,#51854);
#42314=AXIS2_PLACEMENT_3D('',#64898,#51856,#51857);
#42315=AXIS2_PLACEMENT_3D('',#64900,#51859,#51860);
#42316=AXIS2_PLACEMENT_3D('',#64902,#51862,#51863);
#42317=AXIS2_PLACEMENT_3D('',#64904,#51865,#51866);
#42318=AXIS2_PLACEMENT_3D('',#64905,#51867,#51868);
#42319=AXIS2_PLACEMENT_3D('',#64908,#51871,#51872);
#42320=AXIS2_PLACEMENT_3D('',#64910,#51874,#51875);
#42321=AXIS2_PLACEMENT_3D('',#64912,#51877,#51878);
#42322=AXIS2_PLACEMENT_3D('',#64914,#51880,#51881);
#42323=AXIS2_PLACEMENT_3D('',#64916,#51883,#51884);
#42324=AXIS2_PLACEMENT_3D('',#64917,#51885,#51886);
#42325=AXIS2_PLACEMENT_3D('',#64920,#51889,#51890);
#42326=AXIS2_PLACEMENT_3D('',#64922,#51892,#51893);
#42327=AXIS2_PLACEMENT_3D('',#64924,#51895,#51896);
#42328=AXIS2_PLACEMENT_3D('',#64926,#51898,#51899);
#42329=AXIS2_PLACEMENT_3D('',#64928,#51901,#51902);
#42330=AXIS2_PLACEMENT_3D('',#64929,#51903,#51904);
#42331=AXIS2_PLACEMENT_3D('',#64932,#51907,#51908);
#42332=AXIS2_PLACEMENT_3D('',#64934,#51910,#51911);
#42333=AXIS2_PLACEMENT_3D('',#64936,#51913,#51914);
#42334=AXIS2_PLACEMENT_3D('',#64938,#51916,#51917);
#42335=AXIS2_PLACEMENT_3D('',#64940,#51919,#51920);
#42336=AXIS2_PLACEMENT_3D('',#64941,#51921,#51922);
#42337=AXIS2_PLACEMENT_3D('',#64944,#51925,#51926);
#42338=AXIS2_PLACEMENT_3D('',#64946,#51928,#51929);
#42339=AXIS2_PLACEMENT_3D('',#64948,#51931,#51932);
#42340=AXIS2_PLACEMENT_3D('',#64950,#51934,#51935);
#42341=AXIS2_PLACEMENT_3D('',#64952,#51937,#51938);
#42342=AXIS2_PLACEMENT_3D('',#64953,#51939,#51940);
#42343=AXIS2_PLACEMENT_3D('',#64956,#51943,#51944);
#42344=AXIS2_PLACEMENT_3D('',#64958,#51946,#51947);
#42345=AXIS2_PLACEMENT_3D('',#64960,#51949,#51950);
#42346=AXIS2_PLACEMENT_3D('',#64962,#51952,#51953);
#42347=AXIS2_PLACEMENT_3D('',#64964,#51955,#51956);
#42348=AXIS2_PLACEMENT_3D('',#64965,#51957,#51958);
#42349=AXIS2_PLACEMENT_3D('',#64968,#51961,#51962);
#42350=AXIS2_PLACEMENT_3D('',#64970,#51964,#51965);
#42351=AXIS2_PLACEMENT_3D('',#64972,#51967,#51968);
#42352=AXIS2_PLACEMENT_3D('',#64974,#51970,#51971);
#42353=AXIS2_PLACEMENT_3D('',#64976,#51973,#51974);
#42354=AXIS2_PLACEMENT_3D('',#64977,#51975,#51976);
#42355=AXIS2_PLACEMENT_3D('',#64980,#51979,#51980);
#42356=AXIS2_PLACEMENT_3D('',#64982,#51982,#51983);
#42357=AXIS2_PLACEMENT_3D('',#64984,#51985,#51986);
#42358=AXIS2_PLACEMENT_3D('',#64986,#51988,#51989);
#42359=AXIS2_PLACEMENT_3D('',#64988,#51991,#51992);
#42360=AXIS2_PLACEMENT_3D('',#64989,#51993,#51994);
#42361=AXIS2_PLACEMENT_3D('',#64992,#51997,#51998);
#42362=AXIS2_PLACEMENT_3D('',#64994,#52000,#52001);
#42363=AXIS2_PLACEMENT_3D('',#64996,#52003,#52004);
#42364=AXIS2_PLACEMENT_3D('',#64998,#52006,#52007);
#42365=AXIS2_PLACEMENT_3D('',#65000,#52009,#52010);
#42366=AXIS2_PLACEMENT_3D('',#65001,#52011,#52012);
#42367=AXIS2_PLACEMENT_3D('',#65004,#52015,#52016);
#42368=AXIS2_PLACEMENT_3D('',#65006,#52018,#52019);
#42369=AXIS2_PLACEMENT_3D('',#65008,#52021,#52022);
#42370=AXIS2_PLACEMENT_3D('',#65010,#52024,#52025);
#42371=AXIS2_PLACEMENT_3D('',#65012,#52027,#52028);
#42372=AXIS2_PLACEMENT_3D('',#65013,#52029,#52030);
#42373=AXIS2_PLACEMENT_3D('',#65016,#52033,#52034);
#42374=AXIS2_PLACEMENT_3D('',#65018,#52036,#52037);
#42375=AXIS2_PLACEMENT_3D('',#65020,#52039,#52040);
#42376=AXIS2_PLACEMENT_3D('',#65022,#52042,#52043);
#42377=AXIS2_PLACEMENT_3D('',#65024,#52045,#52046);
#42378=AXIS2_PLACEMENT_3D('',#65025,#52047,#52048);
#42379=AXIS2_PLACEMENT_3D('',#65028,#52051,#52052);
#42380=AXIS2_PLACEMENT_3D('',#65030,#52054,#52055);
#42381=AXIS2_PLACEMENT_3D('',#65032,#52057,#52058);
#42382=AXIS2_PLACEMENT_3D('',#65034,#52060,#52061);
#42383=AXIS2_PLACEMENT_3D('',#65036,#52063,#52064);
#42384=AXIS2_PLACEMENT_3D('',#65037,#52065,#52066);
#42385=AXIS2_PLACEMENT_3D('',#65040,#52069,#52070);
#42386=AXIS2_PLACEMENT_3D('',#65042,#52072,#52073);
#42387=AXIS2_PLACEMENT_3D('',#65044,#52075,#52076);
#42388=AXIS2_PLACEMENT_3D('',#65046,#52078,#52079);
#42389=AXIS2_PLACEMENT_3D('',#65048,#52081,#52082);
#42390=AXIS2_PLACEMENT_3D('',#65049,#52083,#52084);
#42391=AXIS2_PLACEMENT_3D('',#65052,#52087,#52088);
#42392=AXIS2_PLACEMENT_3D('',#65054,#52090,#52091);
#42393=AXIS2_PLACEMENT_3D('',#65056,#52093,#52094);
#42394=AXIS2_PLACEMENT_3D('',#65058,#52096,#52097);
#42395=AXIS2_PLACEMENT_3D('',#65060,#52099,#52100);
#42396=AXIS2_PLACEMENT_3D('',#65061,#52101,#52102);
#42397=AXIS2_PLACEMENT_3D('',#65064,#52105,#52106);
#42398=AXIS2_PLACEMENT_3D('',#65066,#52108,#52109);
#42399=AXIS2_PLACEMENT_3D('',#65068,#52111,#52112);
#42400=AXIS2_PLACEMENT_3D('',#65070,#52114,#52115);
#42401=AXIS2_PLACEMENT_3D('',#65072,#52117,#52118);
#42402=AXIS2_PLACEMENT_3D('',#65073,#52119,#52120);
#42403=AXIS2_PLACEMENT_3D('',#65076,#52123,#52124);
#42404=AXIS2_PLACEMENT_3D('',#65078,#52126,#52127);
#42405=AXIS2_PLACEMENT_3D('',#65080,#52129,#52130);
#42406=AXIS2_PLACEMENT_3D('',#65082,#52132,#52133);
#42407=AXIS2_PLACEMENT_3D('',#65084,#52135,#52136);
#42408=AXIS2_PLACEMENT_3D('',#65085,#52137,#52138);
#42409=AXIS2_PLACEMENT_3D('',#65088,#52141,#52142);
#42410=AXIS2_PLACEMENT_3D('',#65090,#52144,#52145);
#42411=AXIS2_PLACEMENT_3D('',#65092,#52147,#52148);
#42412=AXIS2_PLACEMENT_3D('',#65094,#52150,#52151);
#42413=AXIS2_PLACEMENT_3D('',#65096,#52153,#52154);
#42414=AXIS2_PLACEMENT_3D('',#65097,#52155,#52156);
#42415=AXIS2_PLACEMENT_3D('',#65100,#52159,#52160);
#42416=AXIS2_PLACEMENT_3D('',#65102,#52162,#52163);
#42417=AXIS2_PLACEMENT_3D('',#65104,#52165,#52166);
#42418=AXIS2_PLACEMENT_3D('',#65106,#52168,#52169);
#42419=AXIS2_PLACEMENT_3D('',#65108,#52171,#52172);
#42420=AXIS2_PLACEMENT_3D('',#65109,#52173,#52174);
#42421=AXIS2_PLACEMENT_3D('',#65112,#52177,#52178);
#42422=AXIS2_PLACEMENT_3D('',#65114,#52180,#52181);
#42423=AXIS2_PLACEMENT_3D('',#65116,#52183,#52184);
#42424=AXIS2_PLACEMENT_3D('',#65118,#52186,#52187);
#42425=AXIS2_PLACEMENT_3D('',#65120,#52189,#52190);
#42426=AXIS2_PLACEMENT_3D('',#65121,#52191,#52192);
#42427=AXIS2_PLACEMENT_3D('',#65124,#52195,#52196);
#42428=AXIS2_PLACEMENT_3D('',#65126,#52198,#52199);
#42429=AXIS2_PLACEMENT_3D('',#65128,#52201,#52202);
#42430=AXIS2_PLACEMENT_3D('',#65130,#52204,#52205);
#42431=AXIS2_PLACEMENT_3D('',#65132,#52207,#52208);
#42432=AXIS2_PLACEMENT_3D('',#65133,#52209,#52210);
#42433=AXIS2_PLACEMENT_3D('',#65136,#52213,#52214);
#42434=AXIS2_PLACEMENT_3D('',#65138,#52216,#52217);
#42435=AXIS2_PLACEMENT_3D('',#65140,#52219,#52220);
#42436=AXIS2_PLACEMENT_3D('',#65142,#52222,#52223);
#42437=AXIS2_PLACEMENT_3D('',#65144,#52225,#52226);
#42438=AXIS2_PLACEMENT_3D('',#65145,#52227,#52228);
#42439=AXIS2_PLACEMENT_3D('',#65148,#52231,#52232);
#42440=AXIS2_PLACEMENT_3D('',#65150,#52234,#52235);
#42441=AXIS2_PLACEMENT_3D('',#65152,#52237,#52238);
#42442=AXIS2_PLACEMENT_3D('',#65154,#52240,#52241);
#42443=AXIS2_PLACEMENT_3D('',#65156,#52243,#52244);
#42444=AXIS2_PLACEMENT_3D('',#65157,#52245,#52246);
#42445=AXIS2_PLACEMENT_3D('',#65160,#52249,#52250);
#42446=AXIS2_PLACEMENT_3D('',#65162,#52252,#52253);
#42447=AXIS2_PLACEMENT_3D('',#65164,#52255,#52256);
#42448=AXIS2_PLACEMENT_3D('',#65166,#52258,#52259);
#42449=AXIS2_PLACEMENT_3D('',#65168,#52261,#52262);
#42450=AXIS2_PLACEMENT_3D('',#65169,#52263,#52264);
#42451=AXIS2_PLACEMENT_3D('',#65172,#52267,#52268);
#42452=AXIS2_PLACEMENT_3D('',#65174,#52270,#52271);
#42453=AXIS2_PLACEMENT_3D('',#65176,#52273,#52274);
#42454=AXIS2_PLACEMENT_3D('',#65178,#52276,#52277);
#42455=AXIS2_PLACEMENT_3D('',#65180,#52279,#52280);
#42456=AXIS2_PLACEMENT_3D('',#65181,#52281,#52282);
#42457=AXIS2_PLACEMENT_3D('',#65184,#52285,#52286);
#42458=AXIS2_PLACEMENT_3D('',#65186,#52288,#52289);
#42459=AXIS2_PLACEMENT_3D('',#65188,#52291,#52292);
#42460=AXIS2_PLACEMENT_3D('',#65190,#52294,#52295);
#42461=AXIS2_PLACEMENT_3D('',#65192,#52297,#52298);
#42462=AXIS2_PLACEMENT_3D('',#65193,#52299,#52300);
#42463=AXIS2_PLACEMENT_3D('',#65196,#52303,#52304);
#42464=AXIS2_PLACEMENT_3D('',#65198,#52306,#52307);
#42465=AXIS2_PLACEMENT_3D('',#65200,#52309,#52310);
#42466=AXIS2_PLACEMENT_3D('',#65202,#52312,#52313);
#42467=AXIS2_PLACEMENT_3D('',#65204,#52315,#52316);
#42468=AXIS2_PLACEMENT_3D('',#65205,#52317,#52318);
#42469=AXIS2_PLACEMENT_3D('',#65208,#52321,#52322);
#42470=AXIS2_PLACEMENT_3D('',#65210,#52324,#52325);
#42471=AXIS2_PLACEMENT_3D('',#65212,#52327,#52328);
#42472=AXIS2_PLACEMENT_3D('',#65214,#52330,#52331);
#42473=AXIS2_PLACEMENT_3D('',#65216,#52333,#52334);
#42474=AXIS2_PLACEMENT_3D('',#65217,#52335,#52336);
#42475=AXIS2_PLACEMENT_3D('',#65220,#52339,#52340);
#42476=AXIS2_PLACEMENT_3D('',#65222,#52342,#52343);
#42477=AXIS2_PLACEMENT_3D('',#65224,#52345,#52346);
#42478=AXIS2_PLACEMENT_3D('',#65226,#52348,#52349);
#42479=AXIS2_PLACEMENT_3D('',#65228,#52351,#52352);
#42480=AXIS2_PLACEMENT_3D('',#65229,#52353,#52354);
#42481=AXIS2_PLACEMENT_3D('',#65232,#52357,#52358);
#42482=AXIS2_PLACEMENT_3D('',#65234,#52360,#52361);
#42483=AXIS2_PLACEMENT_3D('',#65236,#52363,#52364);
#42484=AXIS2_PLACEMENT_3D('',#65238,#52366,#52367);
#42485=AXIS2_PLACEMENT_3D('',#65240,#52369,#52370);
#42486=AXIS2_PLACEMENT_3D('',#65241,#52371,#52372);
#42487=AXIS2_PLACEMENT_3D('',#65244,#52375,#52376);
#42488=AXIS2_PLACEMENT_3D('',#65246,#52378,#52379);
#42489=AXIS2_PLACEMENT_3D('',#65248,#52381,#52382);
#42490=AXIS2_PLACEMENT_3D('',#65250,#52384,#52385);
#42491=AXIS2_PLACEMENT_3D('',#65252,#52387,#52388);
#42492=AXIS2_PLACEMENT_3D('',#65253,#52389,#52390);
#42493=AXIS2_PLACEMENT_3D('',#65256,#52393,#52394);
#42494=AXIS2_PLACEMENT_3D('',#65258,#52396,#52397);
#42495=AXIS2_PLACEMENT_3D('',#65260,#52399,#52400);
#42496=AXIS2_PLACEMENT_3D('',#65262,#52402,#52403);
#42497=AXIS2_PLACEMENT_3D('',#65264,#52405,#52406);
#42498=AXIS2_PLACEMENT_3D('',#65265,#52407,#52408);
#42499=AXIS2_PLACEMENT_3D('',#65268,#52411,#52412);
#42500=AXIS2_PLACEMENT_3D('',#65270,#52414,#52415);
#42501=AXIS2_PLACEMENT_3D('',#65272,#52417,#52418);
#42502=AXIS2_PLACEMENT_3D('',#65274,#52420,#52421);
#42503=AXIS2_PLACEMENT_3D('',#65276,#52423,#52424);
#42504=AXIS2_PLACEMENT_3D('',#65277,#52425,#52426);
#42505=AXIS2_PLACEMENT_3D('',#65280,#52429,#52430);
#42506=AXIS2_PLACEMENT_3D('',#65282,#52432,#52433);
#42507=AXIS2_PLACEMENT_3D('',#65284,#52435,#52436);
#42508=AXIS2_PLACEMENT_3D('',#65286,#52438,#52439);
#42509=AXIS2_PLACEMENT_3D('',#65288,#52441,#52442);
#42510=AXIS2_PLACEMENT_3D('',#65289,#52443,#52444);
#42511=AXIS2_PLACEMENT_3D('',#65290,#52445,#52446);
#42512=AXIS2_PLACEMENT_3D('',#65291,#52447,#52448);
#42513=AXIS2_PLACEMENT_3D('',#65292,#52449,#52450);
#42514=DIRECTION('axis',(0.,0.,1.));
#42515=DIRECTION('refdir',(1.,0.,0.));
#42516=DIRECTION('axis',(0.,0.,1.));
#42517=DIRECTION('refdir',(1.,0.,0.));
#42518=DIRECTION('center_axis',(-1.,-4.38245930773088E-16,0.));
#42519=DIRECTION('ref_axis',(4.38245930773088E-16,-1.,0.));
#42520=DIRECTION('center_axis',(-1.,-4.38245930773088E-16,0.));
#42521=DIRECTION('ref_axis',(4.38245930773088E-16,-1.,0.));
#42522=DIRECTION('',(-1.,-4.38245930773088E-16,0.));
#42523=DIRECTION('center_axis',(-1.,-4.38245930773088E-16,0.));
#42524=DIRECTION('ref_axis',(-4.38245930773088E-16,1.,0.));
#42525=DIRECTION('center_axis',(-1.,-4.38245930773088E-16,0.));
#42526=DIRECTION('ref_axis',(4.38245930773088E-16,-1.,0.));
#42527=DIRECTION('center_axis',(-1.,-4.38245930773088E-16,0.));
#42528=DIRECTION('ref_axis',(4.38245930773088E-16,-1.,0.));
#42529=DIRECTION('',(-1.,-4.38245930773088E-16,0.));
#42530=DIRECTION('center_axis',(-1.,-4.38245930773088E-16,0.));
#42531=DIRECTION('ref_axis',(4.38245930773088E-16,-1.,0.));
#42532=DIRECTION('center_axis',(-1.,-4.38245930773088E-16,0.));
#42533=DIRECTION('ref_axis',(4.38245930773088E-16,-1.,0.));
#42534=DIRECTION('center_axis',(-1.,-4.38245930773088E-16,0.));
#42535=DIRECTION('ref_axis',(4.38245930773088E-16,-1.,0.));
#42536=DIRECTION('',(-1.,-4.38245930773088E-16,0.));
#42537=DIRECTION('center_axis',(-1.,-4.38245930773088E-16,0.));
#42538=DIRECTION('ref_axis',(-4.38245930773088E-16,1.,0.));
#42539=DIRECTION('center_axis',(-1.,-4.38245930773088E-16,0.));
#42540=DIRECTION('ref_axis',(4.38245930773088E-16,-1.,0.));
#42541=DIRECTION('center_axis',(-1.,-4.38245930773088E-16,0.));
#42542=DIRECTION('ref_axis',(4.38245930773088E-16,-1.,0.));
#42543=DIRECTION('',(-1.,-4.38245930773088E-16,0.));
#42544=DIRECTION('center_axis',(-1.,-4.38245930773088E-16,0.));
#42545=DIRECTION('ref_axis',(4.38245930773088E-16,-1.,0.));
#42546=DIRECTION('center_axis',(0.,0.,-1.));
#42547=DIRECTION('ref_axis',(-1.,0.,0.));
#42548=DIRECTION('center_axis',(0.,0.,-1.));
#42549=DIRECTION('ref_axis',(0.,-1.,0.));
#42550=DIRECTION('',(0.,0.,-1.));
#42551=DIRECTION('center_axis',(0.,0.,-1.));
#42552=DIRECTION('ref_axis',(1.,0.,0.));
#42553=DIRECTION('center_axis',(0.,0.,-1.));
#42554=DIRECTION('ref_axis',(-1.,0.,0.));
#42555=DIRECTION('center_axis',(0.,0.,1.));
#42556=DIRECTION('ref_axis',(0.,-1.,0.));
#42557=DIRECTION('',(0.,0.,-1.));
#42558=DIRECTION('center_axis',(0.,0.,1.));
#42559=DIRECTION('ref_axis',(-1.,0.,0.));
#42560=DIRECTION('center_axis',(1.,1.46081976924362E-16,0.));
#42561=DIRECTION('ref_axis',(-1.46081976924362E-16,1.,0.));
#42562=DIRECTION('center_axis',(1.,1.46081976924362E-16,0.));
#42563=DIRECTION('ref_axis',(-1.46081976924362E-16,1.,0.));
#42564=DIRECTION('',(1.,1.46081976924362E-16,0.));
#42565=DIRECTION('center_axis',(1.,1.92420077553238E-16,0.));
#42566=DIRECTION('ref_axis',(-1.92420077553238E-16,1.,0.));
#42567=DIRECTION('',(1.,1.46081976924362E-16,0.));
#42568=DIRECTION('center_axis',(1.,1.46081976924362E-16,0.));
#42569=DIRECTION('ref_axis',(-1.46081976924362E-16,1.,0.));
#42570=DIRECTION('center_axis',(-1.,-1.46081976924362E-16,0.));
#42571=DIRECTION('ref_axis',(-1.46081976924362E-16,1.,0.));
#42572=DIRECTION('',(1.,1.46081976924362E-16,0.));
#42573=DIRECTION('center_axis',(-1.,-1.92420077553238E-16,0.));
#42574=DIRECTION('ref_axis',(-1.92420077553238E-16,1.,0.));
#42575=DIRECTION('',(1.,1.46081976924362E-16,0.));
#42576=DIRECTION('center_axis',(1.,1.46081976924362E-16,0.));
#42577=DIRECTION('ref_axis',(-1.46081976924362E-16,1.,0.));
#42578=DIRECTION('center_axis',(-1.,-1.46081976924362E-16,0.));
#42579=DIRECTION('ref_axis',(-1.46081976924362E-16,1.,0.));
#42580=DIRECTION('',(1.,1.46081976924362E-16,0.));
#42581=DIRECTION('center_axis',(-1.,-1.92420077553238E-16,0.));
#42582=DIRECTION('ref_axis',(-1.92420077553238E-16,1.,0.));
#42583=DIRECTION('',(1.,1.46081976924362E-16,0.));
#42584=DIRECTION('center_axis',(1.,1.46081976924362E-16,0.));
#42585=DIRECTION('ref_axis',(-1.46081976924362E-16,1.,0.));
#42586=DIRECTION('center_axis',(-1.,-1.46081976924362E-16,0.));
#42587=DIRECTION('ref_axis',(-1.46081976924362E-16,1.,0.));
#42588=DIRECTION('',(1.,1.46081976924362E-16,0.));
#42589=DIRECTION('center_axis',(-1.,-1.92420077553238E-16,0.));
#42590=DIRECTION('ref_axis',(-1.92420077553238E-16,1.,0.));
#42591=DIRECTION('',(1.,1.46081976924362E-16,0.));
#42592=DIRECTION('center_axis',(1.,1.46081976924362E-16,0.));
#42593=DIRECTION('ref_axis',(-1.46081976924362E-16,1.,0.));
#42594=DIRECTION('center_axis',(-1.,-1.46081976924362E-16,0.));
#42595=DIRECTION('ref_axis',(-1.46081976924362E-16,1.,0.));
#42596=DIRECTION('',(1.,1.46081976924362E-16,0.));
#42597=DIRECTION('center_axis',(-1.,-1.92420077553238E-16,0.));
#42598=DIRECTION('ref_axis',(-1.92420077553238E-16,1.,0.));
#42599=DIRECTION('',(1.,1.46081976924362E-16,0.));
#42600=DIRECTION('center_axis',(1.,1.46081976924362E-16,0.));
#42601=DIRECTION('ref_axis',(-1.46081976924362E-16,1.,0.));
#42602=DIRECTION('center_axis',(-1.,-1.46081976924362E-16,0.));
#42603=DIRECTION('ref_axis',(-1.46081976924362E-16,1.,0.));
#42604=DIRECTION('',(1.,1.46081976924362E-16,0.));
#42605=DIRECTION('center_axis',(-1.,-1.92420077553238E-16,0.));
#42606=DIRECTION('ref_axis',(-1.92420077553238E-16,1.,0.));
#42607=DIRECTION('',(1.,1.46081976924362E-16,0.));
#42608=DIRECTION('center_axis',(1.,1.46081976924362E-16,0.));
#42609=DIRECTION('ref_axis',(-1.46081976924362E-16,1.,0.));
#42610=DIRECTION('center_axis',(1.,1.46081976924362E-16,0.));
#42611=DIRECTION('ref_axis',(-1.46081976924362E-16,1.,0.));
#42612=DIRECTION('',(1.,1.46081976924362E-16,0.));
#42613=DIRECTION('center_axis',(1.,1.92420077553238E-16,0.));
#42614=DIRECTION('ref_axis',(-1.92420077553238E-16,1.,0.));
#42615=DIRECTION('',(1.,1.46081976924362E-16,0.));
#42616=DIRECTION('center_axis',(1.,1.46081976924362E-16,0.));
#42617=DIRECTION('ref_axis',(-1.46081976924362E-16,1.,0.));
#42618=DIRECTION('center_axis',(1.,1.46081976924362E-16,0.));
#42619=DIRECTION('ref_axis',(-1.46081976924362E-16,1.,0.));
#42620=DIRECTION('',(1.,1.46081976924362E-16,0.));
#42621=DIRECTION('center_axis',(1.,1.92420077553238E-16,0.));
#42622=DIRECTION('ref_axis',(-1.92420077553238E-16,1.,0.));
#42623=DIRECTION('',(1.,1.46081976924362E-16,0.));
#42624=DIRECTION('center_axis',(1.,1.46081976924362E-16,0.));
#42625=DIRECTION('ref_axis',(-1.46081976924362E-16,1.,0.));
#42626=DIRECTION('center_axis',(1.,1.46081976924362E-16,0.));
#42627=DIRECTION('ref_axis',(-1.46081976924362E-16,1.,0.));
#42628=DIRECTION('',(1.,1.46081976924362E-16,0.));
#42629=DIRECTION('center_axis',(1.,1.92420077553238E-16,0.));
#42630=DIRECTION('ref_axis',(-1.92420077553238E-16,1.,0.));
#42631=DIRECTION('',(1.,1.46081976924362E-16,0.));
#42632=DIRECTION('center_axis',(1.,1.46081976924362E-16,0.));
#42633=DIRECTION('ref_axis',(-1.46081976924362E-16,1.,0.));
#42634=DIRECTION('center_axis',(1.,1.46081976924362E-16,0.));
#42635=DIRECTION('ref_axis',(-1.46081976924362E-16,1.,0.));
#42636=DIRECTION('',(1.,1.46081976924362E-16,0.));
#42637=DIRECTION('center_axis',(1.,1.92420077553238E-16,0.));
#42638=DIRECTION('ref_axis',(-1.92420077553238E-16,1.,0.));
#42639=DIRECTION('',(1.,1.46081976924362E-16,0.));
#42640=DIRECTION('center_axis',(1.,1.46081976924362E-16,0.));
#42641=DIRECTION('ref_axis',(-1.46081976924362E-16,1.,0.));
#42642=DIRECTION('center_axis',(1.,1.46081976924362E-16,0.));
#42643=DIRECTION('ref_axis',(-1.46081976924362E-16,1.,0.));
#42644=DIRECTION('',(1.,1.46081976924362E-16,0.));
#42645=DIRECTION('center_axis',(1.,1.92420077553238E-16,0.));
#42646=DIRECTION('ref_axis',(-1.92420077553238E-16,1.,0.));
#42647=DIRECTION('',(1.,1.46081976924362E-16,0.));
#42648=DIRECTION('center_axis',(1.,1.46081976924362E-16,0.));
#42649=DIRECTION('ref_axis',(-1.46081976924362E-16,1.,0.));
#42650=DIRECTION('center_axis',(1.,1.46081976924362E-16,0.));
#42651=DIRECTION('ref_axis',(-1.46081976924362E-16,1.,0.));
#42652=DIRECTION('',(1.,1.46081976924362E-16,0.));
#42653=DIRECTION('center_axis',(1.,1.92420077553238E-16,0.));
#42654=DIRECTION('ref_axis',(-1.92420077553238E-16,1.,0.));
#42655=DIRECTION('',(1.,1.46081976924362E-16,0.));
#42656=DIRECTION('center_axis',(1.,1.46081976924362E-16,0.));
#42657=DIRECTION('ref_axis',(-1.46081976924362E-16,1.,0.));
#42658=DIRECTION('center_axis',(1.,1.46081976924362E-16,0.));
#42659=DIRECTION('ref_axis',(-1.46081976924362E-16,1.,0.));
#42660=DIRECTION('',(1.,1.46081976924362E-16,0.));
#42661=DIRECTION('center_axis',(1.,1.92420077553238E-16,0.));
#42662=DIRECTION('ref_axis',(-1.92420077553238E-16,1.,0.));
#42663=DIRECTION('',(1.,1.46081976924362E-16,0.));
#42664=DIRECTION('center_axis',(1.,1.46081976924362E-16,0.));
#42665=DIRECTION('ref_axis',(-1.46081976924362E-16,1.,0.));
#42666=DIRECTION('center_axis',(-1.,-1.46081976924362E-16,0.));
#42667=DIRECTION('ref_axis',(-1.46081976924362E-16,1.,0.));
#42668=DIRECTION('',(1.,1.46081976924362E-16,0.));
#42669=DIRECTION('center_axis',(-1.,-1.92420077553238E-16,0.));
#42670=DIRECTION('ref_axis',(-1.92420077553238E-16,1.,0.));
#42671=DIRECTION('',(1.,1.46081976924362E-16,0.));
#42672=DIRECTION('center_axis',(1.,1.46081976924362E-16,0.));
#42673=DIRECTION('ref_axis',(-1.46081976924362E-16,1.,0.));
#42674=DIRECTION('center_axis',(-1.,-1.46081976924362E-16,0.));
#42675=DIRECTION('ref_axis',(-1.46081976924362E-16,1.,0.));
#42676=DIRECTION('',(1.,1.46081976924362E-16,0.));
#42677=DIRECTION('center_axis',(-1.,-1.92420077553238E-16,0.));
#42678=DIRECTION('ref_axis',(-1.92420077553238E-16,1.,0.));
#42679=DIRECTION('',(1.,1.46081976924362E-16,0.));
#42680=DIRECTION('center_axis',(1.,1.46081976924362E-16,0.));
#42681=DIRECTION('ref_axis',(-1.46081976924362E-16,1.,0.));
#42682=DIRECTION('center_axis',(-1.,-1.46081976924362E-16,0.));
#42683=DIRECTION('ref_axis',(-1.46081976924362E-16,1.,0.));
#42684=DIRECTION('',(1.,1.46081976924362E-16,0.));
#42685=DIRECTION('center_axis',(-1.,-1.92420077553238E-16,0.));
#42686=DIRECTION('ref_axis',(-1.92420077553238E-16,1.,0.));
#42687=DIRECTION('',(1.,1.46081976924362E-16,0.));
#42688=DIRECTION('center_axis',(1.,1.46081976924362E-16,0.));
#42689=DIRECTION('ref_axis',(-1.46081976924362E-16,1.,0.));
#42690=DIRECTION('center_axis',(-1.,-1.46081976924362E-16,0.));
#42691=DIRECTION('ref_axis',(-1.46081976924362E-16,1.,1.15648231731787E-15));
#42692=DIRECTION('',(1.,1.46081976924362E-16,0.));
#42693=DIRECTION('center_axis',(-1.,-1.92420077553238E-16,0.));
#42694=DIRECTION('ref_axis',(-1.92420077553238E-16,1.,0.));
#42695=DIRECTION('',(1.,1.46081976924362E-16,0.));
#42696=DIRECTION('center_axis',(1.,1.46081976924362E-16,0.));
#42697=DIRECTION('ref_axis',(-1.46081976924362E-16,1.,0.));
#42698=DIRECTION('center_axis',(1.,1.46081976924362E-16,0.));
#42699=DIRECTION('ref_axis',(-1.46081976924362E-16,1.,0.));
#42700=DIRECTION('',(1.,1.46081976924362E-16,0.));
#42701=DIRECTION('center_axis',(1.,1.92420077553238E-16,0.));
#42702=DIRECTION('ref_axis',(-1.92420077553238E-16,1.,0.));
#42703=DIRECTION('',(1.,1.46081976924362E-16,0.));
#42704=DIRECTION('center_axis',(1.,1.46081976924362E-16,0.));
#42705=DIRECTION('ref_axis',(-1.46081976924362E-16,1.,0.));
#42706=DIRECTION('center_axis',(1.,1.46081976924362E-16,0.));
#42707=DIRECTION('ref_axis',(-1.46081976924362E-16,1.,0.));
#42708=DIRECTION('',(1.,1.46081976924362E-16,0.));
#42709=DIRECTION('center_axis',(1.,1.92420077553238E-16,0.));
#42710=DIRECTION('ref_axis',(-1.92420077553238E-16,1.,0.));
#42711=DIRECTION('',(1.,1.46081976924362E-16,0.));
#42712=DIRECTION('center_axis',(1.,1.46081976924362E-16,0.));
#42713=DIRECTION('ref_axis',(-1.46081976924362E-16,1.,0.));
#42714=DIRECTION('center_axis',(-1.,-1.46081976924362E-16,0.));
#42715=DIRECTION('ref_axis',(-1.46081976924362E-16,1.,0.));
#42716=DIRECTION('',(1.,1.46081976924362E-16,0.));
#42717=DIRECTION('center_axis',(-1.,-1.92420077553238E-16,0.));
#42718=DIRECTION('ref_axis',(-1.92420077553238E-16,1.,0.));
#42719=DIRECTION('',(1.,1.46081976924362E-16,0.));
#42720=DIRECTION('center_axis',(1.,1.46081976924362E-16,0.));
#42721=DIRECTION('ref_axis',(-1.46081976924362E-16,1.,0.));
#42722=DIRECTION('center_axis',(1.,1.46081976924362E-16,0.));
#42723=DIRECTION('ref_axis',(-1.46081976924362E-16,1.,0.));
#42724=DIRECTION('',(1.,1.46081976924362E-16,0.));
#42725=DIRECTION('center_axis',(1.,1.92420077553238E-16,0.));
#42726=DIRECTION('ref_axis',(-1.92420077553238E-16,1.,0.));
#42727=DIRECTION('',(1.,1.46081976924362E-16,0.));
#42728=DIRECTION('center_axis',(1.,1.46081976924362E-16,0.));
#42729=DIRECTION('ref_axis',(-1.46081976924362E-16,1.,0.));
#42730=DIRECTION('center_axis',(-1.,-1.46081976924362E-16,0.));
#42731=DIRECTION('ref_axis',(-1.46081976924362E-16,1.,0.));
#42732=DIRECTION('',(1.,1.46081976924362E-16,0.));
#42733=DIRECTION('center_axis',(-1.,-1.92420077553238E-16,0.));
#42734=DIRECTION('ref_axis',(-1.92420077553238E-16,1.,0.));
#42735=DIRECTION('',(1.,1.46081976924362E-16,0.));
#42736=DIRECTION('center_axis',(1.,1.46081976924362E-16,0.));
#42737=DIRECTION('ref_axis',(-1.46081976924362E-16,1.,0.));
#42738=DIRECTION('center_axis',(-1.,-1.46081976924362E-16,0.));
#42739=DIRECTION('ref_axis',(-1.46081976924362E-16,1.,0.));
#42740=DIRECTION('',(1.,1.46081976924362E-16,0.));
#42741=DIRECTION('center_axis',(-1.,-1.92420077553238E-16,0.));
#42742=DIRECTION('ref_axis',(-1.92420077553238E-16,1.,0.));
#42743=DIRECTION('',(1.,1.46081976924362E-16,0.));
#42744=DIRECTION('center_axis',(1.,1.46081976924362E-16,0.));
#42745=DIRECTION('ref_axis',(-1.46081976924362E-16,1.,0.));
#42746=DIRECTION('center_axis',(1.,1.46081976924362E-16,0.));
#42747=DIRECTION('ref_axis',(-1.46081976924362E-16,1.,0.));
#42748=DIRECTION('',(1.,1.46081976924362E-16,0.));
#42749=DIRECTION('center_axis',(1.,1.92420077553238E-16,0.));
#42750=DIRECTION('ref_axis',(-1.92420077553238E-16,1.,0.));
#42751=DIRECTION('',(1.,1.46081976924362E-16,0.));
#42752=DIRECTION('center_axis',(1.,1.46081976924362E-16,0.));
#42753=DIRECTION('ref_axis',(-1.46081976924362E-16,1.,0.));
#42754=DIRECTION('center_axis',(-1.,-1.46081976924362E-16,0.));
#42755=DIRECTION('ref_axis',(-1.46081976924362E-16,1.,0.));
#42756=DIRECTION('',(1.,1.46081976924362E-16,0.));
#42757=DIRECTION('center_axis',(-1.,-1.92420077553238E-16,0.));
#42758=DIRECTION('ref_axis',(-1.92420077553238E-16,1.,0.));
#42759=DIRECTION('',(1.,1.46081976924362E-16,0.));
#42760=DIRECTION('center_axis',(1.,1.46081976924362E-16,0.));
#42761=DIRECTION('ref_axis',(-1.46081976924362E-16,1.,0.));
#42762=DIRECTION('center_axis',(1.,1.46081976924362E-16,0.));
#42763=DIRECTION('ref_axis',(-1.46081976924362E-16,1.,0.));
#42764=DIRECTION('',(1.,1.46081976924362E-16,0.));
#42765=DIRECTION('center_axis',(1.,1.92420077553238E-16,0.));
#42766=DIRECTION('ref_axis',(-1.92420077553238E-16,1.,0.));
#42767=DIRECTION('',(1.,1.46081976924362E-16,0.));
#42768=DIRECTION('center_axis',(1.,1.46081976924362E-16,0.));
#42769=DIRECTION('ref_axis',(-1.46081976924362E-16,1.,0.));
#42770=DIRECTION('center_axis',(1.,1.46081976924362E-16,0.));
#42771=DIRECTION('ref_axis',(-1.46081976924362E-16,1.,0.));
#42772=DIRECTION('',(1.,1.46081976924362E-16,0.));
#42773=DIRECTION('center_axis',(1.,1.92420077553238E-16,0.));
#42774=DIRECTION('ref_axis',(-1.92420077553238E-16,1.,0.));
#42775=DIRECTION('',(1.,1.46081976924362E-16,0.));
#42776=DIRECTION('center_axis',(1.,1.46081976924362E-16,0.));
#42777=DIRECTION('ref_axis',(-1.46081976924362E-16,1.,0.));
#42778=DIRECTION('center_axis',(1.,1.46081976924362E-16,0.));
#42779=DIRECTION('ref_axis',(-1.46081976924362E-16,1.,0.));
#42780=DIRECTION('',(1.,1.46081976924362E-16,0.));
#42781=DIRECTION('center_axis',(1.,1.92420077553238E-16,0.));
#42782=DIRECTION('ref_axis',(-1.92420077553238E-16,1.,0.));
#42783=DIRECTION('',(1.,1.46081976924362E-16,0.));
#42784=DIRECTION('center_axis',(1.,1.46081976924362E-16,0.));
#42785=DIRECTION('ref_axis',(-1.46081976924362E-16,1.,0.));
#42786=DIRECTION('center_axis',(1.,1.46081976924362E-16,0.));
#42787=DIRECTION('ref_axis',(-1.46081976924362E-16,1.,0.));
#42788=DIRECTION('',(1.,1.46081976924362E-16,0.));
#42789=DIRECTION('center_axis',(1.,1.92420077553238E-16,0.));
#42790=DIRECTION('ref_axis',(-1.92420077553238E-16,1.,0.));
#42791=DIRECTION('',(1.,1.46081976924362E-16,0.));
#42792=DIRECTION('center_axis',(1.,1.46081976924362E-16,0.));
#42793=DIRECTION('ref_axis',(-1.46081976924362E-16,1.,0.));
#42794=DIRECTION('center_axis',(1.,1.46081976924362E-16,0.));
#42795=DIRECTION('ref_axis',(-1.46081976924362E-16,1.,0.));
#42796=DIRECTION('',(1.,1.46081976924362E-16,0.));
#42797=DIRECTION('center_axis',(1.,1.92420077553238E-16,0.));
#42798=DIRECTION('ref_axis',(-1.92420077553238E-16,1.,0.));
#42799=DIRECTION('',(1.,1.46081976924362E-16,0.));
#42800=DIRECTION('center_axis',(1.,1.46081976924362E-16,0.));
#42801=DIRECTION('ref_axis',(-1.46081976924362E-16,1.,0.));
#42802=DIRECTION('center_axis',(-1.,-1.46081976924362E-16,0.));
#42803=DIRECTION('ref_axis',(-1.46081976924362E-16,1.,0.));
#42804=DIRECTION('',(1.,1.46081976924362E-16,0.));
#42805=DIRECTION('center_axis',(-1.,-1.92420077553238E-16,0.));
#42806=DIRECTION('ref_axis',(-1.92420077553238E-16,1.,0.));
#42807=DIRECTION('',(1.,1.46081976924362E-16,0.));
#42808=DIRECTION('center_axis',(1.,1.46081976924362E-16,0.));
#42809=DIRECTION('ref_axis',(-1.46081976924362E-16,1.,0.));
#42810=DIRECTION('center_axis',(-1.,-1.46081976924362E-16,0.));
#42811=DIRECTION('ref_axis',(-1.46081976924362E-16,1.,0.));
#42812=DIRECTION('',(1.,1.46081976924362E-16,0.));
#42813=DIRECTION('center_axis',(-1.,-1.92420077553238E-16,0.));
#42814=DIRECTION('ref_axis',(-1.92420077553238E-16,1.,0.));
#42815=DIRECTION('',(1.,1.46081976924362E-16,0.));
#42816=DIRECTION('center_axis',(1.,1.46081976924362E-16,0.));
#42817=DIRECTION('ref_axis',(-1.46081976924362E-16,1.,0.));
#42818=DIRECTION('center_axis',(-1.,-1.46081976924362E-16,0.));
#42819=DIRECTION('ref_axis',(-1.46081976924362E-16,1.,0.));
#42820=DIRECTION('',(1.,1.46081976924362E-16,0.));
#42821=DIRECTION('center_axis',(-1.,-1.92420077553238E-16,0.));
#42822=DIRECTION('ref_axis',(-1.92420077553238E-16,1.,0.));
#42823=DIRECTION('',(1.,1.46081976924362E-16,0.));
#42824=DIRECTION('center_axis',(1.,1.46081976924362E-16,0.));
#42825=DIRECTION('ref_axis',(-1.46081976924362E-16,1.,0.));
#42826=DIRECTION('center_axis',(-1.,-1.46081976924362E-16,0.));
#42827=DIRECTION('ref_axis',(-1.46081976924362E-16,1.,0.));
#42828=DIRECTION('',(1.,1.46081976924362E-16,0.));
#42829=DIRECTION('center_axis',(-1.,-1.92420077553238E-16,0.));
#42830=DIRECTION('ref_axis',(-1.92420077553238E-16,1.,0.));
#42831=DIRECTION('',(1.,1.46081976924362E-16,0.));
#42832=DIRECTION('center_axis',(1.,1.46081976924362E-16,0.));
#42833=DIRECTION('ref_axis',(-1.46081976924362E-16,1.,0.));
#42834=DIRECTION('center_axis',(-1.,-1.46081976924362E-16,0.));
#42835=DIRECTION('ref_axis',(-1.46081976924362E-16,1.,0.));
#42836=DIRECTION('',(1.,1.46081976924362E-16,0.));
#42837=DIRECTION('center_axis',(-1.,-1.92420077553238E-16,0.));
#42838=DIRECTION('ref_axis',(-1.92420077553238E-16,1.,0.));
#42839=DIRECTION('',(1.,1.46081976924362E-16,0.));
#42840=DIRECTION('center_axis',(1.,1.46081976924362E-16,0.));
#42841=DIRECTION('ref_axis',(-1.46081976924362E-16,1.,0.));
#42842=DIRECTION('center_axis',(-1.,-1.46081976924362E-16,0.));
#42843=DIRECTION('ref_axis',(-1.46081976924362E-16,1.,0.));
#42844=DIRECTION('',(1.,1.46081976924362E-16,0.));
#42845=DIRECTION('center_axis',(-1.,-1.92420077553238E-16,0.));
#42846=DIRECTION('ref_axis',(-1.92420077553238E-16,1.,0.));
#42847=DIRECTION('',(1.,1.46081976924362E-16,0.));
#42848=DIRECTION('center_axis',(1.,1.46081976924362E-16,0.));
#42849=DIRECTION('ref_axis',(-1.46081976924362E-16,1.,0.));
#42850=DIRECTION('center_axis',(-1.,-1.46081976924362E-16,0.));
#42851=DIRECTION('ref_axis',(-1.46081976924362E-16,1.,0.));
#42852=DIRECTION('',(1.,1.46081976924362E-16,0.));
#42853=DIRECTION('center_axis',(-1.,-1.92420077553238E-16,0.));
#42854=DIRECTION('ref_axis',(-1.92420077553238E-16,1.,0.));
#42855=DIRECTION('',(1.,1.46081976924362E-16,0.));
#42856=DIRECTION('center_axis',(1.,1.46081976924362E-16,0.));
#42857=DIRECTION('ref_axis',(-1.46081976924362E-16,1.,0.));
#42858=DIRECTION('center_axis',(1.,1.46081976924362E-16,0.));
#42859=DIRECTION('ref_axis',(-1.46081976924362E-16,1.,0.));
#42860=DIRECTION('',(1.,1.46081976924362E-16,0.));
#42861=DIRECTION('center_axis',(1.,1.92420077553238E-16,0.));
#42862=DIRECTION('ref_axis',(-1.92420077553238E-16,1.,0.));
#42863=DIRECTION('',(1.,1.46081976924362E-16,0.));
#42864=DIRECTION('center_axis',(1.,1.46081976924362E-16,0.));
#42865=DIRECTION('ref_axis',(-1.46081976924362E-16,1.,0.));
#42866=DIRECTION('center_axis',(1.,1.46081976924362E-16,0.));
#42867=DIRECTION('ref_axis',(-1.46081976924362E-16,1.,0.));
#42868=DIRECTION('',(1.,1.46081976924362E-16,0.));
#42869=DIRECTION('center_axis',(1.,1.92420077553238E-16,0.));
#42870=DIRECTION('ref_axis',(-1.92420077553238E-16,1.,0.));
#42871=DIRECTION('',(1.,1.46081976924362E-16,0.));
#42872=DIRECTION('center_axis',(1.,1.46081976924362E-16,0.));
#42873=DIRECTION('ref_axis',(-1.46081976924362E-16,1.,0.));
#42874=DIRECTION('center_axis',(1.,1.46081976924362E-16,0.));
#42875=DIRECTION('ref_axis',(-1.46081976924362E-16,1.,0.));
#42876=DIRECTION('',(1.,1.46081976924362E-16,0.));
#42877=DIRECTION('center_axis',(1.,1.92420077553238E-16,0.));
#42878=DIRECTION('ref_axis',(-1.92420077553238E-16,1.,0.));
#42879=DIRECTION('',(1.,1.46081976924362E-16,0.));
#42880=DIRECTION('center_axis',(1.,1.46081976924362E-16,0.));
#42881=DIRECTION('ref_axis',(-1.46081976924362E-16,1.,0.));
#42882=DIRECTION('center_axis',(1.,1.46081976924362E-16,0.));
#42883=DIRECTION('ref_axis',(-1.46081976924362E-16,1.,0.));
#42884=DIRECTION('',(1.,1.46081976924362E-16,0.));
#42885=DIRECTION('center_axis',(1.,1.92420077553238E-16,0.));
#42886=DIRECTION('ref_axis',(-1.92420077553238E-16,1.,0.));
#42887=DIRECTION('',(1.,1.46081976924362E-16,0.));
#42888=DIRECTION('center_axis',(1.,1.46081976924362E-16,0.));
#42889=DIRECTION('ref_axis',(-1.46081976924362E-16,1.,0.));
#42890=DIRECTION('center_axis',(-1.,-1.46081976924362E-16,0.));
#42891=DIRECTION('ref_axis',(-1.46081976924362E-16,1.,0.));
#42892=DIRECTION('',(1.,1.46081976924362E-16,0.));
#42893=DIRECTION('center_axis',(-1.,-1.92420077553238E-16,0.));
#42894=DIRECTION('ref_axis',(-1.92420077553238E-16,1.,0.));
#42895=DIRECTION('',(1.,1.46081976924362E-16,0.));
#42896=DIRECTION('center_axis',(1.,1.46081976924362E-16,0.));
#42897=DIRECTION('ref_axis',(-1.46081976924362E-16,1.,0.));
#42898=DIRECTION('center_axis',(-1.,-1.46081976924362E-16,0.));
#42899=DIRECTION('ref_axis',(-1.46081976924362E-16,1.,0.));
#42900=DIRECTION('',(1.,1.46081976924362E-16,0.));
#42901=DIRECTION('center_axis',(-1.,-1.92420077553238E-16,0.));
#42902=DIRECTION('ref_axis',(-1.92420077553238E-16,1.,0.));
#42903=DIRECTION('',(1.,1.46081976924362E-16,0.));
#42904=DIRECTION('center_axis',(1.,1.46081976924362E-16,0.));
#42905=DIRECTION('ref_axis',(-1.46081976924362E-16,1.,0.));
#42906=DIRECTION('center_axis',(1.,1.46081976924362E-16,0.));
#42907=DIRECTION('ref_axis',(-1.46081976924362E-16,1.,0.));
#42908=DIRECTION('',(1.,1.46081976924362E-16,0.));
#42909=DIRECTION('center_axis',(1.,1.92420077553238E-16,0.));
#42910=DIRECTION('ref_axis',(-1.92420077553238E-16,1.,0.));
#42911=DIRECTION('',(1.,1.46081976924362E-16,0.));
#42912=DIRECTION('center_axis',(1.,1.46081976924362E-16,0.));
#42913=DIRECTION('ref_axis',(-1.46081976924362E-16,1.,0.));
#42914=DIRECTION('center_axis',(-1.,-1.46081976924362E-16,0.));
#42915=DIRECTION('ref_axis',(-1.46081976924362E-16,1.,0.));
#42916=DIRECTION('',(1.,1.46081976924362E-16,0.));
#42917=DIRECTION('center_axis',(-1.,-1.92420077553238E-16,0.));
#42918=DIRECTION('ref_axis',(-1.92420077553238E-16,1.,0.));
#42919=DIRECTION('',(1.,1.46081976924362E-16,0.));
#42920=DIRECTION('center_axis',(1.,1.46081976924362E-16,0.));
#42921=DIRECTION('ref_axis',(-1.46081976924362E-16,1.,0.));
#42922=DIRECTION('center_axis',(1.,1.46081976924362E-16,0.));
#42923=DIRECTION('ref_axis',(-1.46081976924362E-16,1.,0.));
#42924=DIRECTION('',(1.,1.46081976924362E-16,0.));
#42925=DIRECTION('center_axis',(1.,1.92420077553238E-16,0.));
#42926=DIRECTION('ref_axis',(-1.92420077553238E-16,1.,0.));
#42927=DIRECTION('',(1.,1.46081976924362E-16,0.));
#42928=DIRECTION('center_axis',(1.,1.46081976924362E-16,0.));
#42929=DIRECTION('ref_axis',(-1.46081976924362E-16,1.,0.));
#42930=DIRECTION('center_axis',(1.,1.46081976924362E-16,0.));
#42931=DIRECTION('ref_axis',(-1.46081976924362E-16,1.,0.));
#42932=DIRECTION('',(1.,1.46081976924362E-16,0.));
#42933=DIRECTION('center_axis',(1.,1.92420077553238E-16,0.));
#42934=DIRECTION('ref_axis',(-1.92420077553238E-16,1.,0.));
#42935=DIRECTION('',(1.,1.46081976924362E-16,0.));
#42936=DIRECTION('center_axis',(1.,1.46081976924362E-16,0.));
#42937=DIRECTION('ref_axis',(-1.46081976924362E-16,1.,0.));
#42938=DIRECTION('center_axis',(-1.,-1.46081976924362E-16,0.));
#42939=DIRECTION('ref_axis',(-1.46081976924362E-16,1.,0.));
#42940=DIRECTION('',(1.,1.46081976924362E-16,0.));
#42941=DIRECTION('center_axis',(-1.,-1.92420077553238E-16,0.));
#42942=DIRECTION('ref_axis',(-1.92420077553238E-16,1.,0.));
#42943=DIRECTION('',(1.,1.46081976924362E-16,0.));
#42944=DIRECTION('center_axis',(-1.,-4.38245930773088E-16,0.));
#42945=DIRECTION('ref_axis',(4.38245930773088E-16,-1.,0.));
#42946=DIRECTION('center_axis',(-1.,-4.38245930773088E-16,0.));
#42947=DIRECTION('ref_axis',(4.38245930773088E-16,-1.,0.));
#42948=DIRECTION('',(1.,4.38245930773088E-16,0.));
#42949=DIRECTION('center_axis',(1.,4.38245930773088E-16,0.));
#42950=DIRECTION('ref_axis',(4.38245930773088E-16,-1.,-4.62592926927148E-15));
#42951=DIRECTION('',(-1.,-4.38245930773088E-16,0.));
#42952=DIRECTION('center_axis',(-1.,-4.38245930773088E-16,0.));
#42953=DIRECTION('ref_axis',(4.38245930773088E-16,-1.,0.));
#42954=DIRECTION('center_axis',(-1.,-4.38245930773088E-16,0.));
#42955=DIRECTION('ref_axis',(4.38245930773088E-16,-1.,0.));
#42956=DIRECTION('',(1.,4.38245930773088E-16,0.));
#42957=DIRECTION('center_axis',(1.,4.38245930773088E-16,0.));
#42958=DIRECTION('ref_axis',(4.38245930773088E-16,-1.,-4.62592926927148E-15));
#42959=DIRECTION('',(-1.,-4.38245930773088E-16,0.));
#42960=DIRECTION('center_axis',(-1.,-4.38245930773088E-16,0.));
#42961=DIRECTION('ref_axis',(4.38245930773088E-16,-1.,0.));
#42962=DIRECTION('center_axis',(-1.,-4.38245930773088E-16,0.));
#42963=DIRECTION('ref_axis',(4.38245930773088E-16,-1.,0.));
#42964=DIRECTION('',(1.,4.38245930773088E-16,0.));
#42965=DIRECTION('center_axis',(1.,4.38245930773088E-16,0.));
#42966=DIRECTION('ref_axis',(4.38245930773088E-16,-1.,-1.15648231731787E-14));
#42967=DIRECTION('',(-1.,-4.38245930773088E-16,0.));
#42968=DIRECTION('center_axis',(-1.,-4.38245930773088E-16,0.));
#42969=DIRECTION('ref_axis',(4.38245930773088E-16,-1.,0.));
#42970=DIRECTION('center_axis',(-1.,-4.38245930773088E-16,0.));
#42971=DIRECTION('ref_axis',(4.38245930773088E-16,-1.,0.));
#42972=DIRECTION('',(1.,4.38245930773088E-16,0.));
#42973=DIRECTION('center_axis',(1.,4.38245930773088E-16,0.));
#42974=DIRECTION('ref_axis',(4.38245930773088E-16,-1.,0.));
#42975=DIRECTION('',(-1.,-4.38245930773088E-16,0.));
#42976=DIRECTION('center_axis',(-1.,-4.38245930773088E-16,0.));
#42977=DIRECTION('ref_axis',(4.38245930773088E-16,-1.,0.));
#42978=DIRECTION('center_axis',(-1.,-4.38245930773088E-16,0.));
#42979=DIRECTION('ref_axis',(4.38245930773088E-16,-1.,0.));
#42980=DIRECTION('',(1.,4.38245930773088E-16,0.));
#42981=DIRECTION('center_axis',(1.,4.38245930773088E-16,0.));
#42982=DIRECTION('ref_axis',(4.38245930773088E-16,-1.,4.16333634234433E-14));
#42983=DIRECTION('',(-1.,-4.38245930773088E-16,-8.64002241377108E-33));
#42984=DIRECTION('center_axis',(-1.,-4.38245930773088E-16,0.));
#42985=DIRECTION('ref_axis',(4.38245930773088E-16,-1.,0.));
#42986=DIRECTION('center_axis',(-1.,-4.38245930773088E-16,0.));
#42987=DIRECTION('ref_axis',(4.38245930773088E-16,-1.,0.));
#42988=DIRECTION('',(1.,4.38245930773088E-16,0.));
#42989=DIRECTION('center_axis',(1.,4.38245930773088E-16,0.));
#42990=DIRECTION('ref_axis',(4.38245930773088E-16,-1.,-2.31296463463574E-15));
#42991=DIRECTION('',(-1.,-4.38245930773088E-16,0.));
#42992=DIRECTION('center_axis',(-1.,-4.38245930773088E-16,0.));
#42993=DIRECTION('ref_axis',(4.38245930773088E-16,-1.,0.));
#42994=DIRECTION('center_axis',(-1.,-4.38245930773088E-16,0.));
#42995=DIRECTION('ref_axis',(4.38245930773088E-16,-1.,0.));
#42996=DIRECTION('',(1.,4.38245930773088E-16,0.));
#42997=DIRECTION('center_axis',(1.,4.38245930773088E-16,0.));
#42998=DIRECTION('ref_axis',(4.38245930773088E-16,-1.,1.04083408558608E-14));
#42999=DIRECTION('',(-1.,-4.38245930773088E-16,0.));
#43000=DIRECTION('center_axis',(-1.,-4.38245930773088E-16,0.));
#43001=DIRECTION('ref_axis',(4.38245930773088E-16,-1.,0.));
#43002=DIRECTION('center_axis',(-1.,-4.38245930773088E-16,0.));
#43003=DIRECTION('ref_axis',(4.38245930773088E-16,-1.,0.));
#43004=DIRECTION('',(1.,4.38245930773088E-16,0.));
#43005=DIRECTION('center_axis',(1.,4.38245930773088E-16,0.));
#43006=DIRECTION('ref_axis',(4.38245930773088E-16,-1.,0.));
#43007=DIRECTION('',(-1.,-4.38245930773088E-16,0.));
#43008=DIRECTION('center_axis',(-1.,-4.38245930773088E-16,0.));
#43009=DIRECTION('ref_axis',(4.38245930773088E-16,-1.,0.));
#43010=DIRECTION('center_axis',(-1.,-4.38245930773088E-16,0.));
#43011=DIRECTION('ref_axis',(4.38245930773088E-16,-1.,0.));
#43012=DIRECTION('',(1.,4.38245930773088E-16,0.));
#43013=DIRECTION('center_axis',(1.,4.38245930773088E-16,0.));
#43014=DIRECTION('ref_axis',(4.38245930773088E-16,-1.,-1.61907524424502E-14));
#43015=DIRECTION('',(-1.,-4.38245930773088E-16,0.));
#43016=DIRECTION('center_axis',(-1.,-4.38245930773088E-16,0.));
#43017=DIRECTION('ref_axis',(4.38245930773088E-16,-1.,0.));
#43018=DIRECTION('center_axis',(-1.,-4.38245930773088E-16,0.));
#43019=DIRECTION('ref_axis',(4.38245930773088E-16,-1.,0.));
#43020=DIRECTION('',(1.,4.38245930773088E-16,0.));
#43021=DIRECTION('center_axis',(1.,4.38245930773088E-16,0.));
#43022=DIRECTION('ref_axis',(4.38245930773088E-16,-1.,0.));
#43023=DIRECTION('',(-1.,-4.38245930773088E-16,0.));
#43024=DIRECTION('center_axis',(-1.,-4.38245930773088E-16,0.));
#43025=DIRECTION('ref_axis',(4.38245930773088E-16,-1.,0.));
#43026=DIRECTION('center_axis',(-1.,-4.38245930773088E-16,0.));
#43027=DIRECTION('ref_axis',(4.38245930773088E-16,-1.,0.));
#43028=DIRECTION('',(1.,4.38245930773088E-16,0.));
#43029=DIRECTION('center_axis',(1.,4.38245930773088E-16,0.));
#43030=DIRECTION('ref_axis',(4.38245930773088E-16,-1.,-1.38777878078144E-14));
#43031=DIRECTION('',(-1.,-4.38245930773088E-16,-8.64002241377108E-33));
#43032=DIRECTION('center_axis',(-1.,-4.38245930773088E-16,0.));
#43033=DIRECTION('ref_axis',(4.38245930773088E-16,-1.,0.));
#43034=DIRECTION('center_axis',(-1.,-4.38245930773088E-16,0.));
#43035=DIRECTION('ref_axis',(4.38245930773088E-16,-1.,0.));
#43036=DIRECTION('',(1.,4.38245930773088E-16,0.));
#43037=DIRECTION('center_axis',(1.,4.38245930773088E-16,0.));
#43038=DIRECTION('ref_axis',(4.38245930773088E-16,-1.,1.73472347597681E-15));
#43039=DIRECTION('',(-1.,-4.38245930773088E-16,0.));
#43040=DIRECTION('center_axis',(-1.,-4.38245930773088E-16,0.));
#43041=DIRECTION('ref_axis',(4.38245930773088E-16,-1.,0.));
#43042=DIRECTION('center_axis',(-1.,-4.38245930773088E-16,0.));
#43043=DIRECTION('ref_axis',(4.38245930773088E-16,-1.,0.));
#43044=DIRECTION('',(1.,4.38245930773088E-16,0.));
#43045=DIRECTION('center_axis',(1.,4.38245930773088E-16,0.));
#43046=DIRECTION('ref_axis',(4.38245930773088E-16,-1.,-3.98986399474665E-14));
#43047=DIRECTION('',(-1.,-4.38245930773088E-16,0.));
#43048=DIRECTION('center_axis',(-1.,-4.38245930773088E-16,0.));
#43049=DIRECTION('ref_axis',(4.38245930773088E-16,-1.,0.));
#43050=DIRECTION('center_axis',(-1.,-4.38245930773088E-16,0.));
#43051=DIRECTION('ref_axis',(4.38245930773088E-16,-1.,0.));
#43052=DIRECTION('',(1.,4.38245930773088E-16,0.));
#43053=DIRECTION('center_axis',(1.,4.38245930773088E-16,0.));
#43054=DIRECTION('ref_axis',(4.38245930773088E-16,-1.,0.));
#43055=DIRECTION('',(-1.,-4.38245930773088E-16,0.));
#43056=DIRECTION('center_axis',(-1.,-4.38245930773088E-16,0.));
#43057=DIRECTION('ref_axis',(4.38245930773088E-16,-1.,0.));
#43058=DIRECTION('center_axis',(-1.,-4.38245930773088E-16,0.));
#43059=DIRECTION('ref_axis',(4.38245930773088E-16,-1.,0.));
#43060=DIRECTION('',(1.,4.38245930773088E-16,0.));
#43061=DIRECTION('center_axis',(1.,4.38245930773088E-16,0.));
#43062=DIRECTION('ref_axis',(4.38245930773088E-16,-1.,1.15648231731787E-15));
#43063=DIRECTION('',(-1.,-4.38245930773088E-16,0.));
#43064=DIRECTION('center_axis',(-1.,-4.38245930773088E-16,0.));
#43065=DIRECTION('ref_axis',(4.38245930773088E-16,-1.,0.));
#43066=DIRECTION('center_axis',(-1.,-4.38245930773088E-16,0.));
#43067=DIRECTION('ref_axis',(4.38245930773088E-16,-1.,0.));
#43068=DIRECTION('',(1.,4.38245930773088E-16,0.));
#43069=DIRECTION('center_axis',(1.,4.38245930773088E-16,0.));
#43070=DIRECTION('ref_axis',(4.38245930773088E-16,-1.,-2.31296463463574E-14));
#43071=DIRECTION('',(-1.,-4.38245930773088E-16,0.));
#43072=DIRECTION('center_axis',(-1.,-4.38245930773088E-16,0.));
#43073=DIRECTION('ref_axis',(4.38245930773088E-16,-1.,0.));
#43074=DIRECTION('center_axis',(-1.,-4.38245930773088E-16,0.));
#43075=DIRECTION('ref_axis',(4.38245930773088E-16,-1.,0.));
#43076=DIRECTION('',(1.,4.38245930773088E-16,0.));
#43077=DIRECTION('center_axis',(1.,4.38245930773088E-16,0.));
#43078=DIRECTION('ref_axis',(4.38245930773088E-16,-1.,0.));
#43079=DIRECTION('',(-1.,-4.38245930773088E-16,0.));
#43080=DIRECTION('center_axis',(-1.,-4.38245930773088E-16,0.));
#43081=DIRECTION('ref_axis',(4.38245930773088E-16,-1.,0.));
#43082=DIRECTION('center_axis',(-1.,-4.38245930773088E-16,0.));
#43083=DIRECTION('ref_axis',(4.38245930773088E-16,-1.,0.));
#43084=DIRECTION('',(1.,4.38245930773088E-16,0.));
#43085=DIRECTION('center_axis',(1.,4.38245930773088E-16,0.));
#43086=DIRECTION('ref_axis',(4.38245930773088E-16,-1.,-3.70074341541719E-14));
#43087=DIRECTION('',(-1.,-4.38245930773088E-16,-6.16297582203917E-33));
#43088=DIRECTION('',(-1.,-4.38245930773088E-16,0.));
#43089=DIRECTION('',(1.,4.38245930773088E-16,0.));
#43090=DIRECTION('',(-1.,-4.38245930773088E-16,0.));
#43091=DIRECTION('',(1.,4.38245930773088E-16,0.));
#43092=DIRECTION('',(-1.,-4.38245930773088E-16,0.));
#43093=DIRECTION('',(1.,4.38245930773088E-16,0.));
#43094=DIRECTION('',(-1.,-4.38245930773088E-16,0.));
#43095=DIRECTION('',(1.,4.38245930773088E-16,0.));
#43096=DIRECTION('',(-1.,-4.38245930773088E-16,0.));
#43097=DIRECTION('',(1.,4.38245930773088E-16,0.));
#43098=DIRECTION('center_axis',(-1.,-4.38245930773088E-16,0.));
#43099=DIRECTION('ref_axis',(4.38245930773088E-16,-1.,0.));
#43100=DIRECTION('center_axis',(1.,4.38245930773088E-16,0.));
#43101=DIRECTION('ref_axis',(4.38245930773088E-16,-1.,0.));
#43102=DIRECTION('',(-1.,-4.38245930773088E-16,0.));
#43103=DIRECTION('center_axis',(1.,4.81050193883094E-16,1.4791141972894E-31));
#43104=DIRECTION('ref_axis',(4.81050193883094E-16,-1.,7.11528171381301E-47));
#43105=DIRECTION('center_axis',(-1.,-4.38245930773088E-16,0.));
#43106=DIRECTION('ref_axis',(4.38245930773088E-16,-1.,0.));
#43107=DIRECTION('center_axis',(-1.,-4.38245930773088E-16,0.));
#43108=DIRECTION('ref_axis',(4.38245930773088E-16,-1.,0.));
#43109=DIRECTION('',(-1.,-4.38245930773088E-16,0.));
#43110=DIRECTION('center_axis',(-1.,-4.81050193883094E-16,-1.4791141972894E-31));
#43111=DIRECTION('ref_axis',(4.81050193883094E-16,-1.,7.11528171381301E-47));
#43112=DIRECTION('center_axis',(-1.,-4.38245930773088E-16,0.));
#43113=DIRECTION('ref_axis',(4.38245930773088E-16,-1.,0.));
#43114=DIRECTION('center_axis',(1.,4.38245930773088E-16,0.));
#43115=DIRECTION('ref_axis',(4.38245930773088E-16,-1.,0.));
#43116=DIRECTION('',(-1.,-4.38245930773088E-16,0.));
#43117=DIRECTION('center_axis',(1.,4.81050193883094E-16,1.4791141972894E-31));
#43118=DIRECTION('ref_axis',(4.81050193883094E-16,-1.,7.11528171381301E-47));
#43119=DIRECTION('center_axis',(-1.,-4.38245930773088E-16,0.));
#43120=DIRECTION('ref_axis',(4.38245930773088E-16,-1.,0.));
#43121=DIRECTION('center_axis',(-1.,-4.38245930773088E-16,0.));
#43122=DIRECTION('ref_axis',(4.38245930773088E-16,-1.,0.));
#43123=DIRECTION('',(-1.,-4.38245930773088E-16,0.));
#43124=DIRECTION('center_axis',(-1.,-4.81050193883094E-16,-1.4791141972894E-31));
#43125=DIRECTION('ref_axis',(4.81050193883094E-16,-1.,7.11528171381302E-47));
#43126=DIRECTION('center_axis',(-1.,-4.38245930773088E-16,0.));
#43127=DIRECTION('ref_axis',(0.,0.,1.));
#43128=DIRECTION('center_axis',(-1.,-4.38245930773088E-16,0.));
#43129=DIRECTION('ref_axis',(0.,0.,-1.));
#43130=DIRECTION('center_axis',(-4.38245930773088E-16,1.,-2.089831575765E-16));
#43131=DIRECTION('ref_axis',(0.,-2.089831575765E-16,-1.));
#43132=DIRECTION('center_axis',(-1.,-4.38245930773088E-16,0.));
#43133=DIRECTION('ref_axis',(0.,0.,1.));
#43134=DIRECTION('center_axis',(-1.,-4.38245930773088E-16,0.));
#43135=DIRECTION('ref_axis',(0.,0.,1.));
#43136=DIRECTION('center_axis',(-1.,-4.38245930773088E-16,0.));
#43137=DIRECTION('ref_axis',(4.38245930773088E-16,-1.,0.));
#43138=DIRECTION('center_axis',(-4.38245930773088E-16,1.,-1.9456480777872E-16));
#43139=DIRECTION('ref_axis',(0.,-1.9456480777872E-16,-1.));
#43140=DIRECTION('center_axis',(-1.,-4.38245930773088E-16,0.));
#43141=DIRECTION('ref_axis',(4.38245930773088E-16,-1.,0.));
#43142=DIRECTION('center_axis',(-1.,-4.38245930773088E-16,0.));
#43143=DIRECTION('ref_axis',(0.,0.,1.));
#43144=DIRECTION('center_axis',(-1.,-4.38245930773088E-16,0.));
#43145=DIRECTION('ref_axis',(4.38245930773088E-16,-1.,0.));
#43146=DIRECTION('center_axis',(4.38245930773088E-16,-1.,2.05122036882246E-16));
#43147=DIRECTION('ref_axis',(0.,-2.05122036882246E-16,-1.));
#43148=DIRECTION('center_axis',(-1.,-4.38245930773088E-16,0.));
#43149=DIRECTION('ref_axis',(0.,0.,1.));
#43150=DIRECTION('center_axis',(1.,4.38245930773088E-16,0.));
#43151=DIRECTION('ref_axis',(0.,0.,1.));
#43152=DIRECTION('center_axis',(4.38245930773088E-16,-1.,1.91213816259009E-16));
#43153=DIRECTION('ref_axis',(0.,-1.91213816259009E-16,-1.));
#43154=DIRECTION('center_axis',(0.,1.,0.));
#43155=DIRECTION('ref_axis',(0.,0.,1.));
#43156=DIRECTION('center_axis',(0.,-1.,0.));
#43157=DIRECTION('ref_axis',(0.,0.,1.));
#43158=DIRECTION('',(0.,1.,0.));
#43159=DIRECTION('center_axis',(0.,-1.,0.));
#43160=DIRECTION('ref_axis',(0.,0.,1.));
#43161=DIRECTION('center_axis',(0.,1.,0.));
#43162=DIRECTION('ref_axis',(0.,0.,1.));
#43163=DIRECTION('center_axis',(0.,-1.,0.));
#43164=DIRECTION('ref_axis',(0.,0.,1.));
#43165=DIRECTION('',(0.,1.,0.));
#43166=DIRECTION('center_axis',(0.,-1.,0.));
#43167=DIRECTION('ref_axis',(0.,0.,1.));
#43168=DIRECTION('center_axis',(0.,1.,0.));
#43169=DIRECTION('ref_axis',(0.,0.,1.));
#43170=DIRECTION('center_axis',(0.,-1.,0.));
#43171=DIRECTION('ref_axis',(0.,0.,1.));
#43172=DIRECTION('',(0.,1.,0.));
#43173=DIRECTION('center_axis',(0.,-1.,0.));
#43174=DIRECTION('ref_axis',(0.,0.,1.));
#43175=DIRECTION('center_axis',(0.,1.,0.));
#43176=DIRECTION('ref_axis',(0.,0.,1.));
#43177=DIRECTION('center_axis',(0.,-1.,0.));
#43178=DIRECTION('ref_axis',(0.,0.,1.));
#43179=DIRECTION('',(0.,1.,0.));
#43180=DIRECTION('center_axis',(0.,-1.,0.));
#43181=DIRECTION('ref_axis',(0.,0.,1.));
#43182=DIRECTION('',(-1.,-4.38245930773088E-16,0.));
#43183=DIRECTION('',(1.,4.38245930773088E-16,0.));
#43184=DIRECTION('center_axis',(0.,-1.,0.));
#43185=DIRECTION('ref_axis',(0.,0.,-1.));
#43186=DIRECTION('',(0.,-3.77113799125394E-15,1.));
#43187=DIRECTION('',(-1.,0.,0.));
#43188=DIRECTION('',(0.,0.,-1.));
#43189=DIRECTION('center_axis',(0.,1.,0.));
#43190=DIRECTION('ref_axis',(0.,0.,1.));
#43191=DIRECTION('',(0.,0.,-1.));
#43192=DIRECTION('center_axis',(0.,1.,0.));
#43193=DIRECTION('ref_axis',(0.,0.,-1.));
#43194=DIRECTION('',(0.,0.,-1.));
#43195=DIRECTION('',(-1.,0.,0.));
#43196=DIRECTION('',(0.,-1.41417674672023E-15,1.));
#43197=DIRECTION('',(-1.,0.,0.));
#43198=DIRECTION('',(0.,0.,-1.));
#43199=DIRECTION('',(-1.,0.,0.));
#43200=DIRECTION('',(0.,0.,1.));
#43201=DIRECTION('',(-1.,0.,0.));
#43202=DIRECTION('',(3.77113799125394E-15,1.41417674672023E-15,-1.));
#43203=DIRECTION('',(-1.,0.,0.));
#43204=DIRECTION('',(0.,0.,1.));
#43205=DIRECTION('center_axis',(0.,1.,0.));
#43206=DIRECTION('ref_axis',(0.,0.,1.));
#43207=DIRECTION('',(0.,0.,-1.));
#43208=DIRECTION('center_axis',(0.,1.,0.));
#43209=DIRECTION('ref_axis',(0.,0.,-1.));
#43210=DIRECTION('',(0.,0.,1.));
#43211=DIRECTION('',(-1.,0.,0.));
#43212=DIRECTION('',(-3.77113799125394E-15,3.77113799125394E-15,-1.));
#43213=DIRECTION('',(1.,0.,0.));
#43214=DIRECTION('',(0.,0.,1.));
#43215=DIRECTION('',(1.,0.,0.));
#43216=DIRECTION('',(0.,0.,-1.));
#43217=DIRECTION('',(1.,0.,0.));
#43218=DIRECTION('',(1.,0.,0.));
#43219=DIRECTION('',(-1.,0.,0.));
#43220=DIRECTION('',(1.,0.,0.));
#43221=DIRECTION('',(0.,0.,-1.));
#43222=DIRECTION('',(-1.,0.,0.));
#43223=DIRECTION('',(-1.,0.,0.));
#43224=DIRECTION('',(-1.,0.,0.));
#43225=DIRECTION('',(0.,0.,1.));
#43226=DIRECTION('',(1.,0.,0.));
#43227=DIRECTION('',(-1.,0.,0.));
#43228=DIRECTION('',(1.,0.,0.));
#43229=DIRECTION('',(0.,0.,-1.));
#43230=DIRECTION('',(-1.,0.,0.));
#43231=DIRECTION('',(-1.,0.,0.));
#43232=DIRECTION('',(-1.,0.,0.));
#43233=DIRECTION('',(0.,0.,1.));
#43234=DIRECTION('',(1.,0.,0.));
#43235=DIRECTION('',(-1.,0.,0.));
#43236=DIRECTION('',(1.,0.,0.));
#43237=DIRECTION('',(0.,0.,-1.));
#43238=DIRECTION('',(-1.,0.,0.));
#43239=DIRECTION('',(-1.,0.,0.));
#43240=DIRECTION('',(-1.,0.,0.));
#43241=DIRECTION('',(0.,0.,1.));
#43242=DIRECTION('',(1.,0.,0.));
#43243=DIRECTION('',(-1.,0.,0.));
#43244=DIRECTION('',(1.,0.,0.));
#43245=DIRECTION('',(0.,0.,-1.));
#43246=DIRECTION('',(-1.,0.,0.));
#43247=DIRECTION('',(-1.,0.,0.));
#43248=DIRECTION('',(-1.,0.,0.));
#43249=DIRECTION('',(0.,0.,1.));
#43250=DIRECTION('center_axis',(0.,-1.,0.));
#43251=DIRECTION('ref_axis',(0.,0.,-1.));
#43252=DIRECTION('',(-1.,0.,0.));
#43253=DIRECTION('',(0.,0.,1.));
#43254=DIRECTION('',(1.,0.,0.));
#43255=DIRECTION('',(0.,0.,-1.));
#43256=DIRECTION('',(1.,0.,0.));
#43257=DIRECTION('',(0.,0.,1.));
#43258=DIRECTION('',(1.,0.,0.));
#43259=DIRECTION('',(-3.77113799125394E-15,0.,-1.));
#43260=DIRECTION('',(-1.,0.,0.));
#43261=DIRECTION('',(0.,0.,-1.));
#43262=DIRECTION('center_axis',(0.,-1.,0.));
#43263=DIRECTION('ref_axis',(0.,0.,-1.));
#43264=DIRECTION('',(0.,0.,-1.));
#43265=DIRECTION('center_axis',(0.,-1.,0.));
#43266=DIRECTION('ref_axis',(0.,0.,-1.));
#43267=DIRECTION('',(0.,0.,-1.));
#43268=DIRECTION('',(-1.,0.,0.));
#43269=DIRECTION('',(3.77113799125394E-15,0.,-1.));
#43270=DIRECTION('',(-1.,0.,0.));
#43271=DIRECTION('',(0.,0.,1.));
#43272=DIRECTION('',(-1.,0.,0.));
#43273=DIRECTION('',(0.,0.,-1.));
#43274=DIRECTION('',(-1.,0.,0.));
#43275=DIRECTION('',(0.,0.,1.));
#43276=DIRECTION('',(-1.,0.,0.));
#43277=DIRECTION('',(0.,0.,1.));
#43278=DIRECTION('center_axis',(0.,-1.,0.));
#43279=DIRECTION('ref_axis',(0.,0.,-1.));
#43280=DIRECTION('',(0.,0.,-1.));
#43281=DIRECTION('center_axis',(0.,-1.,0.));
#43282=DIRECTION('ref_axis',(0.,0.,-1.));
#43283=DIRECTION('',(0.,0.,1.));
#43284=DIRECTION('',(1.,0.,0.));
#43285=DIRECTION('',(0.,0.,-1.));
#43286=DIRECTION('',(1.,0.,0.));
#43287=DIRECTION('',(0.,0.,1.));
#43288=DIRECTION('',(1.,0.,0.));
#43289=DIRECTION('',(0.,0.,-1.));
#43290=DIRECTION('',(1.,0.,0.));
#43291=DIRECTION('',(0.,0.,1.));
#43292=DIRECTION('',(1.,0.,0.));
#43293=DIRECTION('',(0.,0.,-1.));
#43294=DIRECTION('',(1.,0.,0.));
#43295=DIRECTION('',(0.,0.,1.));
#43296=DIRECTION('',(1.,0.,0.));
#43297=DIRECTION('',(0.,0.,-1.));
#43298=DIRECTION('',(1.,0.,0.));
#43299=DIRECTION('',(0.,0.,1.));
#43300=DIRECTION('center_axis',(0.,0.,-1.));
#43301=DIRECTION('ref_axis',(-1.,0.,0.));
#43302=DIRECTION('',(0.,-1.,6.12323399573677E-17));
#43303=DIRECTION('',(0.,-1.,0.));
#43304=DIRECTION('center_axis',(0.,0.,-1.));
#43305=DIRECTION('ref_axis',(-1.,0.,0.));
#43306=DIRECTION('',(0.,-1.,6.12323399573677E-17));
#43307=DIRECTION('',(0.,1.,0.));
#43308=DIRECTION('center_axis',(0.,0.,-1.));
#43309=DIRECTION('ref_axis',(-1.,0.,0.));
#43310=DIRECTION('',(-1.15648231731787E-15,1.,0.));
#43311=DIRECTION('',(1.,0.,0.));
#43312=DIRECTION('',(0.,-1.,0.));
#43313=DIRECTION('center_axis',(0.,0.,1.));
#43314=DIRECTION('ref_axis',(-1.,1.06251812903579E-14,0.));
#43315=DIRECTION('',(-1.,-3.56237856673809E-16,0.));
#43316=DIRECTION('center_axis',(0.,0.,1.));
#43317=DIRECTION('ref_axis',(-1.,8.67361737988403E-16,0.));
#43318=DIRECTION('',(0.,-1.,0.));
#43319=DIRECTION('',(1.,0.,0.));
#43320=DIRECTION('',(-1.,0.,0.));
#43321=DIRECTION('',(1.,0.,0.));
#43322=DIRECTION('',(0.,1.,0.));
#43323=DIRECTION('',(-1.,0.,0.));
#43324=DIRECTION('',(-1.,0.,0.));
#43325=DIRECTION('',(-1.,0.,0.));
#43326=DIRECTION('',(-5.8432790769745E-16,1.,0.));
#43327=DIRECTION('',(1.,5.8432790769745E-16,0.));
#43328=DIRECTION('',(-1.,-5.8432790769745E-16,0.));
#43329=DIRECTION('',(1.,5.8432790769745E-16,0.));
#43330=DIRECTION('',(5.8432790769745E-16,-1.,0.));
#43331=DIRECTION('',(-1.,-5.8432790769745E-16,0.));
#43332=DIRECTION('',(-1.,-5.8432790769745E-16,0.));
#43333=DIRECTION('',(-1.,-5.8432790769745E-16,0.));
#43334=DIRECTION('center_axis',(0.,0.,-1.));
#43335=DIRECTION('ref_axis',(-1.,0.,0.));
#43336=DIRECTION('',(-1.,0.,0.));
#43337=DIRECTION('',(-1.15648231731787E-15,1.,0.));
#43338=DIRECTION('center_axis',(0.,0.,1.));
#43339=DIRECTION('ref_axis',(-1.,8.67361737988403E-16,0.));
#43340=DIRECTION('',(-1.,-3.56237856673809E-16,0.));
#43341=DIRECTION('center_axis',(0.,0.,1.));
#43342=DIRECTION('ref_axis',(-1.,1.06251812903579E-14,0.));
#43343=DIRECTION('',(0.,-1.,0.));
#43344=DIRECTION('',(-1.,0.,0.));
#43345=DIRECTION('',(0.,1.,0.));
#43346=DIRECTION('',(-1.,0.,0.));
#43347=DIRECTION('',(0.,-1.,0.));
#43348=DIRECTION('',(-5.8432790769745E-16,1.,0.));
#43349=DIRECTION('',(1.,5.8432790769745E-16,0.));
#43350=DIRECTION('',(5.8432790769745E-16,-1.,0.));
#43351=DIRECTION('',(1.,5.8432790769745E-16,0.));
#43352=DIRECTION('center_axis',(0.,0.,1.));
#43353=DIRECTION('ref_axis',(1.,0.,0.));
#43354=DIRECTION('',(0.,-1.,6.12323399573677E-17));
#43355=DIRECTION('',(0.,-1.,0.));
#43356=DIRECTION('center_axis',(0.,0.,1.));
#43357=DIRECTION('ref_axis',(1.,0.,0.));
#43358=DIRECTION('',(0.,-1.,6.12323399573677E-17));
#43359=DIRECTION('',(0.,1.,0.));
#43360=DIRECTION('center_axis',(1.,1.46081976924362E-16,0.));
#43361=DIRECTION('ref_axis',(-1.46081976924362E-16,1.,0.));
#43362=DIRECTION('',(1.46081976924362E-16,-1.,0.));
#43363=DIRECTION('',(-1.03295556492353E-16,0.707106781186547,0.707106781186547));
#43364=DIRECTION('',(0.,0.,-1.));
#43365=DIRECTION('',(1.03295556492353E-16,-0.707106781186547,0.707106781186547));
#43366=DIRECTION('',(1.46081976924362E-16,-1.,0.));
#43367=DIRECTION('',(0.,0.,1.));
#43368=DIRECTION('center_axis',(1.,1.46081976924362E-16,0.));
#43369=DIRECTION('ref_axis',(-1.46081976924362E-16,1.,0.));
#43370=DIRECTION('',(0.,0.,-1.));
#43371=DIRECTION('center_axis',(1.,1.46081976924362E-16,0.));
#43372=DIRECTION('ref_axis',(-1.46081976924362E-16,1.,0.));
#43373=DIRECTION('',(0.,0.,1.));
#43374=DIRECTION('',(-1.92420077553238E-16,1.,0.));
#43375=DIRECTION('',(-1.92420077553238E-16,1.,0.));
#43376=DIRECTION('center_axis',(-1.,-1.92420077553238E-16,0.));
#43377=DIRECTION('ref_axis',(-1.92420077553238E-16,1.,0.));
#43378=DIRECTION('',(-1.92420077553238E-16,1.,0.));
#43379=DIRECTION('',(-1.92420077553238E-16,1.,0.));
#43380=DIRECTION('center_axis',(-1.,-1.92420077553238E-16,0.));
#43381=DIRECTION('ref_axis',(-1.92420077553238E-16,1.,0.));
#43382=DIRECTION('',(-1.92420077553238E-16,1.,0.));
#43383=DIRECTION('',(-1.92420077553238E-16,1.,0.));
#43384=DIRECTION('center_axis',(-1.,-1.92420077553238E-16,0.));
#43385=DIRECTION('ref_axis',(-1.92420077553238E-16,1.,0.));
#43386=DIRECTION('',(-1.92420077553238E-16,1.,0.));
#43387=DIRECTION('',(-1.92420077553238E-16,1.,0.));
#43388=DIRECTION('center_axis',(-1.,-1.92420077553238E-16,0.));
#43389=DIRECTION('ref_axis',(-1.92420077553238E-16,1.,0.));
#43390=DIRECTION('',(-1.92420077553238E-16,1.,0.));
#43391=DIRECTION('',(-1.92420077553238E-16,1.,0.));
#43392=DIRECTION('center_axis',(-1.,-1.92420077553238E-16,0.));
#43393=DIRECTION('ref_axis',(-1.92420077553238E-16,1.,0.));
#43394=DIRECTION('',(-1.92420077553238E-16,1.,0.));
#43395=DIRECTION('',(-1.92420077553238E-16,1.,0.));
#43396=DIRECTION('center_axis',(-1.,-1.92420077553238E-16,0.));
#43397=DIRECTION('ref_axis',(-1.92420077553238E-16,1.,0.));
#43398=DIRECTION('',(-1.92420077553238E-16,1.,0.));
#43399=DIRECTION('',(-1.92420077553238E-16,1.,0.));
#43400=DIRECTION('center_axis',(-1.,-1.92420077553238E-16,0.));
#43401=DIRECTION('ref_axis',(-1.92420077553238E-16,1.,0.));
#43402=DIRECTION('',(-1.92420077553238E-16,1.,0.));
#43403=DIRECTION('',(-1.92420077553238E-16,1.,0.));
#43404=DIRECTION('center_axis',(-1.,-1.92420077553238E-16,0.));
#43405=DIRECTION('ref_axis',(-1.92420077553238E-16,1.,0.));
#43406=DIRECTION('',(-1.92420077553238E-16,1.,0.));
#43407=DIRECTION('',(-1.92420077553238E-16,1.,0.));
#43408=DIRECTION('center_axis',(-1.,-1.92420077553238E-16,0.));
#43409=DIRECTION('ref_axis',(-1.92420077553238E-16,1.,0.));
#43410=DIRECTION('',(-1.92420077553238E-16,1.,0.));
#43411=DIRECTION('',(-1.92420077553238E-16,1.,0.));
#43412=DIRECTION('center_axis',(-1.,-1.92420077553238E-16,0.));
#43413=DIRECTION('ref_axis',(-1.92420077553238E-16,1.,0.));
#43414=DIRECTION('',(-1.92420077553238E-16,1.,0.));
#43415=DIRECTION('',(-1.92420077553238E-16,1.,0.));
#43416=DIRECTION('center_axis',(-1.,-1.92420077553238E-16,0.));
#43417=DIRECTION('ref_axis',(-1.92420077553238E-16,1.,0.));
#43418=DIRECTION('',(-1.92420077553238E-16,1.,0.));
#43419=DIRECTION('',(-1.92420077553238E-16,1.,0.));
#43420=DIRECTION('center_axis',(-1.,-1.92420077553238E-16,0.));
#43421=DIRECTION('ref_axis',(-1.92420077553238E-16,1.,0.));
#43422=DIRECTION('',(1.92420077553238E-16,-1.,0.));
#43423=DIRECTION('center_axis',(-1.,-1.92420077553238E-16,0.));
#43424=DIRECTION('ref_axis',(-1.92420077553238E-16,1.,0.));
#43425=DIRECTION('',(1.92420077553238E-16,-1.,0.));
#43426=DIRECTION('',(1.92420077553238E-16,-1.,0.));
#43427=DIRECTION('center_axis',(-1.,-1.92420077553238E-16,0.));
#43428=DIRECTION('ref_axis',(-1.92420077553238E-16,1.,0.));
#43429=DIRECTION('',(1.92420077553238E-16,-1.,0.));
#43430=DIRECTION('',(1.92420077553238E-16,-1.,0.));
#43431=DIRECTION('center_axis',(-1.,-1.92420077553238E-16,0.));
#43432=DIRECTION('ref_axis',(-1.92420077553238E-16,1.,0.));
#43433=DIRECTION('',(1.92420077553238E-16,-1.,0.));
#43434=DIRECTION('',(1.92420077553238E-16,-1.,0.));
#43435=DIRECTION('center_axis',(-1.,-1.92420077553238E-16,0.));
#43436=DIRECTION('ref_axis',(-1.92420077553238E-16,1.,0.));
#43437=DIRECTION('',(1.92420077553238E-16,-1.,0.));
#43438=DIRECTION('',(1.92420077553238E-16,-1.,0.));
#43439=DIRECTION('center_axis',(-1.,-1.92420077553238E-16,0.));
#43440=DIRECTION('ref_axis',(-1.92420077553238E-16,1.,0.));
#43441=DIRECTION('',(1.92420077553238E-16,-1.,0.));
#43442=DIRECTION('',(1.92420077553238E-16,-1.,0.));
#43443=DIRECTION('center_axis',(-1.,-1.92420077553238E-16,0.));
#43444=DIRECTION('ref_axis',(-1.92420077553238E-16,1.,0.));
#43445=DIRECTION('',(1.92420077553238E-16,-1.,0.));
#43446=DIRECTION('',(1.92420077553238E-16,-1.,0.));
#43447=DIRECTION('center_axis',(-1.,-1.92420077553238E-16,0.));
#43448=DIRECTION('ref_axis',(-1.92420077553238E-16,1.,0.));
#43449=DIRECTION('',(1.92420077553238E-16,-1.,0.));
#43450=DIRECTION('',(1.92420077553238E-16,-1.,0.));
#43451=DIRECTION('center_axis',(-1.,-1.92420077553238E-16,0.));
#43452=DIRECTION('ref_axis',(-1.92420077553238E-16,1.,0.));
#43453=DIRECTION('',(1.92420077553238E-16,-1.,0.));
#43454=DIRECTION('',(1.92420077553238E-16,-1.,0.));
#43455=DIRECTION('center_axis',(-1.,-1.92420077553238E-16,0.));
#43456=DIRECTION('ref_axis',(-1.92420077553238E-16,1.,0.));
#43457=DIRECTION('',(1.92420077553238E-16,-1.,0.));
#43458=DIRECTION('',(1.92420077553238E-16,-1.,0.));
#43459=DIRECTION('center_axis',(-1.,-1.92420077553238E-16,0.));
#43460=DIRECTION('ref_axis',(-1.92420077553238E-16,1.,0.));
#43461=DIRECTION('',(1.92420077553238E-16,-1.,0.));
#43462=DIRECTION('',(1.92420077553238E-16,-1.,0.));
#43463=DIRECTION('center_axis',(-1.,-1.92420077553238E-16,0.));
#43464=DIRECTION('ref_axis',(-1.92420077553238E-16,1.,0.));
#43465=DIRECTION('',(1.92420077553238E-16,-1.,0.));
#43466=DIRECTION('',(1.92420077553238E-16,-1.,0.));
#43467=DIRECTION('center_axis',(-1.,-1.92420077553238E-16,0.));
#43468=DIRECTION('ref_axis',(-1.92420077553238E-16,1.,0.));
#43469=DIRECTION('',(1.92420077553238E-16,-1.,0.));
#43470=DIRECTION('',(-1.92420077553238E-16,1.,0.));
#43471=DIRECTION('center_axis',(1.,1.92420077553238E-16,0.));
#43472=DIRECTION('ref_axis',(-1.92420077553238E-16,1.,0.));
#43473=DIRECTION('',(-1.92420077553238E-16,1.,0.));
#43474=DIRECTION('',(-1.92420077553238E-16,1.,0.));
#43475=DIRECTION('center_axis',(1.,1.92420077553238E-16,0.));
#43476=DIRECTION('ref_axis',(-1.92420077553238E-16,1.,0.));
#43477=DIRECTION('',(-1.92420077553238E-16,1.,0.));
#43478=DIRECTION('',(-1.92420077553238E-16,1.,0.));
#43479=DIRECTION('center_axis',(1.,1.92420077553238E-16,0.));
#43480=DIRECTION('ref_axis',(-1.92420077553238E-16,1.,0.));
#43481=DIRECTION('',(-1.92420077553238E-16,1.,0.));
#43482=DIRECTION('',(-1.92420077553238E-16,1.,0.));
#43483=DIRECTION('center_axis',(1.,1.92420077553238E-16,0.));
#43484=DIRECTION('ref_axis',(-1.92420077553238E-16,1.,0.));
#43485=DIRECTION('',(-1.92420077553238E-16,1.,0.));
#43486=DIRECTION('',(-1.92420077553238E-16,1.,0.));
#43487=DIRECTION('center_axis',(1.,1.92420077553238E-16,0.));
#43488=DIRECTION('ref_axis',(-1.92420077553238E-16,1.,0.));
#43489=DIRECTION('',(-1.92420077553238E-16,1.,0.));
#43490=DIRECTION('',(-1.92420077553238E-16,1.,0.));
#43491=DIRECTION('center_axis',(1.,1.92420077553238E-16,0.));
#43492=DIRECTION('ref_axis',(-1.92420077553238E-16,1.,0.));
#43493=DIRECTION('',(-1.92420077553238E-16,1.,0.));
#43494=DIRECTION('',(-1.92420077553238E-16,1.,0.));
#43495=DIRECTION('center_axis',(1.,1.92420077553238E-16,0.));
#43496=DIRECTION('ref_axis',(-1.92420077553238E-16,1.,0.));
#43497=DIRECTION('',(-1.92420077553238E-16,1.,0.));
#43498=DIRECTION('',(-1.92420077553238E-16,1.,0.));
#43499=DIRECTION('center_axis',(1.,1.92420077553238E-16,0.));
#43500=DIRECTION('ref_axis',(-1.92420077553238E-16,1.,0.));
#43501=DIRECTION('',(-1.92420077553238E-16,1.,0.));
#43502=DIRECTION('',(-1.92420077553238E-16,1.,0.));
#43503=DIRECTION('center_axis',(1.,1.92420077553238E-16,0.));
#43504=DIRECTION('ref_axis',(-1.92420077553238E-16,1.,0.));
#43505=DIRECTION('',(-1.92420077553238E-16,1.,0.));
#43506=DIRECTION('',(-1.92420077553238E-16,1.,0.));
#43507=DIRECTION('center_axis',(1.,1.92420077553238E-16,0.));
#43508=DIRECTION('ref_axis',(-1.92420077553238E-16,1.,0.));
#43509=DIRECTION('',(-1.92420077553238E-16,1.,0.));
#43510=DIRECTION('',(-1.92420077553238E-16,1.,0.));
#43511=DIRECTION('center_axis',(1.,1.92420077553238E-16,0.));
#43512=DIRECTION('ref_axis',(-1.92420077553238E-16,1.,0.));
#43513=DIRECTION('',(-1.92420077553238E-16,1.,0.));
#43514=DIRECTION('',(-1.92420077553238E-16,1.,0.));
#43515=DIRECTION('center_axis',(1.,1.92420077553238E-16,0.));
#43516=DIRECTION('ref_axis',(-1.92420077553238E-16,1.,0.));
#43517=DIRECTION('',(-1.92420077553238E-16,1.,0.));
#43518=DIRECTION('',(1.92420077553238E-16,-1.,0.));
#43519=DIRECTION('',(1.92420077553238E-16,-1.,0.));
#43520=DIRECTION('center_axis',(1.,1.92420077553238E-16,0.));
#43521=DIRECTION('ref_axis',(-1.92420077553238E-16,1.,0.));
#43522=DIRECTION('',(1.92420077553238E-16,-1.,0.));
#43523=DIRECTION('',(1.92420077553238E-16,-1.,0.));
#43524=DIRECTION('center_axis',(1.,1.92420077553238E-16,0.));
#43525=DIRECTION('ref_axis',(-1.92420077553238E-16,1.,0.));
#43526=DIRECTION('',(1.92420077553238E-16,-1.,0.));
#43527=DIRECTION('',(1.92420077553238E-16,-1.,0.));
#43528=DIRECTION('center_axis',(1.,1.92420077553238E-16,0.));
#43529=DIRECTION('ref_axis',(-1.92420077553238E-16,1.,0.));
#43530=DIRECTION('',(1.92420077553238E-16,-1.,0.));
#43531=DIRECTION('',(1.92420077553238E-16,-1.,0.));
#43532=DIRECTION('center_axis',(1.,1.92420077553238E-16,0.));
#43533=DIRECTION('ref_axis',(-1.92420077553238E-16,1.,0.));
#43534=DIRECTION('',(1.92420077553238E-16,-1.,0.));
#43535=DIRECTION('',(1.92420077553238E-16,-1.,0.));
#43536=DIRECTION('center_axis',(1.,1.92420077553238E-16,0.));
#43537=DIRECTION('ref_axis',(-1.92420077553238E-16,1.,0.));
#43538=DIRECTION('',(1.92420077553238E-16,-1.,0.));
#43539=DIRECTION('',(1.92420077553238E-16,-1.,0.));
#43540=DIRECTION('center_axis',(1.,1.92420077553238E-16,0.));
#43541=DIRECTION('ref_axis',(-1.92420077553238E-16,1.,0.));
#43542=DIRECTION('',(1.92420077553238E-16,-1.,0.));
#43543=DIRECTION('',(1.92420077553238E-16,-1.,0.));
#43544=DIRECTION('center_axis',(1.,1.92420077553238E-16,0.));
#43545=DIRECTION('ref_axis',(-1.92420077553238E-16,1.,0.));
#43546=DIRECTION('',(1.92420077553238E-16,-1.,0.));
#43547=DIRECTION('',(1.92420077553238E-16,-1.,0.));
#43548=DIRECTION('center_axis',(1.,1.92420077553238E-16,0.));
#43549=DIRECTION('ref_axis',(-1.92420077553238E-16,1.,0.));
#43550=DIRECTION('',(1.92420077553238E-16,-1.,0.));
#43551=DIRECTION('',(1.92420077553238E-16,-1.,0.));
#43552=DIRECTION('center_axis',(1.,1.92420077553238E-16,0.));
#43553=DIRECTION('ref_axis',(-1.92420077553238E-16,1.,0.));
#43554=DIRECTION('',(1.92420077553238E-16,-1.,0.));
#43555=DIRECTION('',(1.92420077553238E-16,-1.,0.));
#43556=DIRECTION('center_axis',(1.,1.92420077553238E-16,0.));
#43557=DIRECTION('ref_axis',(-1.92420077553238E-16,1.,0.));
#43558=DIRECTION('',(1.92420077553238E-16,-1.,0.));
#43559=DIRECTION('',(1.92420077553238E-16,-1.,0.));
#43560=DIRECTION('center_axis',(1.,1.92420077553238E-16,0.));
#43561=DIRECTION('ref_axis',(-1.92420077553238E-16,1.,0.));
#43562=DIRECTION('',(1.92420077553238E-16,-1.,0.));
#43563=DIRECTION('',(1.92420077553238E-16,-1.,0.));
#43564=DIRECTION('center_axis',(1.,1.92420077553238E-16,0.));
#43565=DIRECTION('ref_axis',(-1.92420077553238E-16,1.,0.));
#43566=DIRECTION('center_axis',(1.,1.46081976924362E-16,0.));
#43567=DIRECTION('ref_axis',(-1.46081976924362E-16,1.,0.));
#43568=DIRECTION('',(0.,0.,-1.));
#43569=DIRECTION('',(1.03295556492353E-16,-0.707106781186547,-0.707106781186547));
#43570=DIRECTION('',(1.46081976924362E-16,-1.,0.));
#43571=DIRECTION('',(0.,0.,-1.));
#43572=DIRECTION('center_axis',(1.,1.46081976924362E-16,0.));
#43573=DIRECTION('ref_axis',(-1.46081976924362E-16,1.,0.));
#43574=DIRECTION('',(0.,0.,-1.));
#43575=DIRECTION('center_axis',(-1.,-8.82055185704388E-15,0.));
#43576=DIRECTION('ref_axis',(0.,0.,1.));
#43577=DIRECTION('',(0.,0.,-1.));
#43578=DIRECTION('',(1.46081976924362E-16,-1.,0.));
#43579=DIRECTION('',(-1.03295556492353E-16,0.707106781186547,-0.707106781186547));
#43580=DIRECTION('',(1.46081976924362E-16,-1.,0.));
#43581=DIRECTION('center_axis',(1.,1.46081976924362E-16,0.));
#43582=DIRECTION('ref_axis',(-1.46081976924362E-16,1.,0.));
#43583=DIRECTION('',(1.46081976924362E-16,-1.,0.));
#43584=DIRECTION('',(1.46081976924362E-16,-1.,0.));
#43585=DIRECTION('center_axis',(1.,1.46081976924362E-16,0.));
#43586=DIRECTION('ref_axis',(-1.46081976924362E-16,1.,0.));
#43587=DIRECTION('',(1.46081976924362E-16,-1.,0.));
#43588=DIRECTION('',(-1.46081976924362E-16,1.,0.));
#43589=DIRECTION('center_axis',(-1.,-1.46081976924362E-16,0.));
#43590=DIRECTION('ref_axis',(-1.46081976924362E-16,1.,0.));
#43591=DIRECTION('',(-1.46081976924362E-16,1.,0.));
#43592=DIRECTION('',(-1.46081976924362E-16,1.,0.));
#43593=DIRECTION('center_axis',(-1.,-1.46081976924362E-16,0.));
#43594=DIRECTION('ref_axis',(-1.46081976924362E-16,1.,0.));
#43595=DIRECTION('',(-1.46081976924362E-16,1.,0.));
#43596=DIRECTION('',(-1.46081976924362E-16,1.,0.));
#43597=DIRECTION('center_axis',(-1.,-1.46081976924362E-16,0.));
#43598=DIRECTION('ref_axis',(-1.46081976924362E-16,1.,0.));
#43599=DIRECTION('',(-1.46081976924362E-16,1.,0.));
#43600=DIRECTION('',(-1.46081976924362E-16,1.,0.));
#43601=DIRECTION('center_axis',(-1.,-1.46081976924362E-16,0.));
#43602=DIRECTION('ref_axis',(-1.46081976924362E-16,1.,0.));
#43603=DIRECTION('',(-1.46081976924362E-16,1.,0.));
#43604=DIRECTION('',(-1.46081976924362E-16,1.,0.));
#43605=DIRECTION('center_axis',(-1.,-1.46081976924362E-16,0.));
#43606=DIRECTION('ref_axis',(-1.46081976924362E-16,1.,0.));
#43607=DIRECTION('',(-1.46081976924362E-16,1.,0.));
#43608=DIRECTION('',(1.46081976924362E-16,-1.,0.));
#43609=DIRECTION('center_axis',(1.,1.46081976924362E-16,0.));
#43610=DIRECTION('ref_axis',(-1.46081976924362E-16,1.,0.));
#43611=DIRECTION('',(1.46081976924362E-16,-1.,0.));
#43612=DIRECTION('',(1.46081976924362E-16,-1.,0.));
#43613=DIRECTION('center_axis',(1.,1.46081976924362E-16,0.));
#43614=DIRECTION('ref_axis',(-1.46081976924362E-16,1.,0.));
#43615=DIRECTION('',(1.46081976924362E-16,-1.,0.));
#43616=DIRECTION('',(1.46081976924362E-16,-1.,0.));
#43617=DIRECTION('center_axis',(1.,1.46081976924362E-16,0.));
#43618=DIRECTION('ref_axis',(-1.46081976924362E-16,1.,0.));
#43619=DIRECTION('',(1.46081976924362E-16,-1.,0.));
#43620=DIRECTION('',(1.46081976924362E-16,-1.,0.));
#43621=DIRECTION('center_axis',(1.,1.46081976924362E-16,0.));
#43622=DIRECTION('ref_axis',(-1.46081976924362E-16,1.,0.));
#43623=DIRECTION('',(1.46081976924362E-16,-1.,0.));
#43624=DIRECTION('',(1.46081976924362E-16,-1.,0.));
#43625=DIRECTION('center_axis',(1.,1.46081976924362E-16,0.));
#43626=DIRECTION('ref_axis',(-1.46081976924362E-16,1.,0.));
#43627=DIRECTION('',(1.46081976924362E-16,-1.,0.));
#43628=DIRECTION('',(-1.46081976924362E-16,1.,0.));
#43629=DIRECTION('center_axis',(-1.,-1.46081976924362E-16,0.));
#43630=DIRECTION('ref_axis',(-1.46081976924362E-16,1.,0.));
#43631=DIRECTION('',(-1.46081976924362E-16,1.,0.));
#43632=DIRECTION('',(1.46081976924362E-16,-1.,0.));
#43633=DIRECTION('',(1.46081976924362E-16,-1.,0.));
#43634=DIRECTION('center_axis',(-1.,-1.46081976924362E-16,0.));
#43635=DIRECTION('ref_axis',(-1.46081976924362E-16,1.,0.));
#43636=DIRECTION('',(-1.46081976924362E-16,1.,0.));
#43637=DIRECTION('',(-1.46081976924362E-16,1.,0.));
#43638=DIRECTION('center_axis',(1.,1.46081976924362E-16,0.));
#43639=DIRECTION('ref_axis',(-1.46081976924362E-16,1.,0.));
#43640=DIRECTION('',(-1.46081976924362E-16,1.,0.));
#43641=DIRECTION('',(-1.46081976924362E-16,1.,0.));
#43642=DIRECTION('center_axis',(1.,1.46081976924362E-16,0.));
#43643=DIRECTION('ref_axis',(-1.46081976924362E-16,1.,0.));
#43644=DIRECTION('',(1.46081976924362E-16,-1.,0.));
#43645=DIRECTION('',(1.46081976924362E-16,-1.,0.));
#43646=DIRECTION('center_axis',(-1.,-1.46081976924362E-16,0.));
#43647=DIRECTION('ref_axis',(-1.46081976924362E-16,1.,0.));
#43648=DIRECTION('',(1.46081976924362E-16,-1.,0.));
#43649=DIRECTION('',(1.46081976924362E-16,-1.,0.));
#43650=DIRECTION('center_axis',(-1.,-1.46081976924362E-16,0.));
#43651=DIRECTION('ref_axis',(-1.46081976924362E-16,1.,0.));
#43652=DIRECTION('',(-1.46081976924362E-16,1.,0.));
#43653=DIRECTION('',(-1.46081976924362E-16,1.,0.));
#43654=DIRECTION('center_axis',(1.,1.46081976924362E-16,0.));
#43655=DIRECTION('ref_axis',(-1.46081976924362E-16,1.,0.));
#43656=DIRECTION('',(-1.46081976924362E-16,1.,0.));
#43657=DIRECTION('',(-1.46081976924362E-16,1.,0.));
#43658=DIRECTION('center_axis',(1.,1.46081976924362E-16,0.));
#43659=DIRECTION('ref_axis',(-1.46081976924362E-16,1.,0.));
#43660=DIRECTION('',(-1.46081976924362E-16,1.,0.));
#43661=DIRECTION('',(-1.46081976924362E-16,1.,0.));
#43662=DIRECTION('center_axis',(1.,1.46081976924362E-16,0.));
#43663=DIRECTION('ref_axis',(-1.46081976924362E-16,1.,0.));
#43664=DIRECTION('',(-1.46081976924362E-16,1.,0.));
#43665=DIRECTION('',(-1.46081976924362E-16,1.,0.));
#43666=DIRECTION('center_axis',(1.,1.46081976924362E-16,0.));
#43667=DIRECTION('ref_axis',(-1.46081976924362E-16,1.,0.));
#43668=DIRECTION('',(-1.46081976924362E-16,1.,0.));
#43669=DIRECTION('',(-1.46081976924362E-16,1.,0.));
#43670=DIRECTION('center_axis',(1.,1.46081976924362E-16,0.));
#43671=DIRECTION('ref_axis',(-1.46081976924362E-16,1.,0.));
#43672=DIRECTION('',(-1.46081976924362E-16,1.,0.));
#43673=DIRECTION('',(-1.46081976924362E-16,1.,0.));
#43674=DIRECTION('center_axis',(1.,1.46081976924362E-16,0.));
#43675=DIRECTION('ref_axis',(-1.46081976924362E-16,1.,0.));
#43676=DIRECTION('',(-1.46081976924362E-16,1.,0.));
#43677=DIRECTION('',(-1.46081976924362E-16,1.,0.));
#43678=DIRECTION('center_axis',(1.,1.46081976924362E-16,0.));
#43679=DIRECTION('ref_axis',(-1.46081976924362E-16,1.,0.));
#43680=DIRECTION('',(1.46081976924362E-16,-1.,0.));
#43681=DIRECTION('',(1.46081976924362E-16,-1.,0.));
#43682=DIRECTION('center_axis',(-1.,-1.46081976924362E-16,0.));
#43683=DIRECTION('ref_axis',(-1.46081976924362E-16,1.,0.));
#43684=DIRECTION('',(1.46081976924362E-16,-1.,0.));
#43685=DIRECTION('',(1.46081976924362E-16,-1.,0.));
#43686=DIRECTION('center_axis',(-1.,-1.46081976924362E-16,0.));
#43687=DIRECTION('ref_axis',(-1.46081976924362E-16,1.,0.));
#43688=DIRECTION('',(1.46081976924362E-16,-1.,0.));
#43689=DIRECTION('',(1.46081976924362E-16,-1.,0.));
#43690=DIRECTION('center_axis',(-1.,-1.46081976924362E-16,0.));
#43691=DIRECTION('ref_axis',(-1.46081976924362E-16,1.,0.));
#43692=DIRECTION('',(-1.46081976924362E-16,1.,0.));
#43693=DIRECTION('',(-1.46081976924362E-16,1.,0.));
#43694=DIRECTION('center_axis',(1.,1.46081976924362E-16,0.));
#43695=DIRECTION('ref_axis',(-1.46081976924362E-16,1.,0.));
#43696=DIRECTION('',(1.46081976924362E-16,-1.,0.));
#43697=DIRECTION('',(1.46081976924362E-16,-1.,0.));
#43698=DIRECTION('center_axis',(-1.,-1.46081976924362E-16,0.));
#43699=DIRECTION('ref_axis',(-1.46081976924362E-16,1.,0.));
#43700=DIRECTION('',(1.46081976924362E-16,-1.,0.));
#43701=DIRECTION('',(1.46081976924362E-16,-1.,0.));
#43702=DIRECTION('center_axis',(-1.,-1.46081976924362E-16,0.));
#43703=DIRECTION('ref_axis',(-1.46081976924362E-16,1.,0.));
#43704=DIRECTION('',(1.46081976924362E-16,-1.,0.));
#43705=DIRECTION('',(1.46081976924362E-16,-1.,0.));
#43706=DIRECTION('center_axis',(-1.,-1.46081976924362E-16,0.));
#43707=DIRECTION('ref_axis',(-1.46081976924362E-16,1.,0.));
#43708=DIRECTION('',(1.46081976924362E-16,-1.,0.));
#43709=DIRECTION('',(1.46081976924362E-16,-1.,0.));
#43710=DIRECTION('center_axis',(-1.,-1.46081976924362E-16,0.));
#43711=DIRECTION('ref_axis',(-1.46081976924362E-16,1.,0.));
#43712=DIRECTION('',(1.46081976924362E-16,-1.,0.));
#43713=DIRECTION('',(1.46081976924362E-16,-1.,0.));
#43714=DIRECTION('center_axis',(-1.,-1.46081976924362E-16,0.));
#43715=DIRECTION('ref_axis',(-1.46081976924362E-16,1.,0.));
#43716=DIRECTION('',(-1.46081976924362E-16,1.,0.));
#43717=DIRECTION('',(-1.46081976924362E-16,1.,0.));
#43718=DIRECTION('center_axis',(1.,1.46081976924362E-16,0.));
#43719=DIRECTION('ref_axis',(-1.46081976924362E-16,1.,0.));
#43720=DIRECTION('',(1.46081976924362E-16,-1.,0.));
#43721=DIRECTION('',(1.46081976924362E-16,-1.,0.));
#43722=DIRECTION('center_axis',(-1.,-1.46081976924362E-16,0.));
#43723=DIRECTION('ref_axis',(-1.46081976924362E-16,1.,0.));
#43724=DIRECTION('',(-1.46081976924362E-16,1.,0.));
#43725=DIRECTION('',(-1.46081976924362E-16,1.,0.));
#43726=DIRECTION('center_axis',(1.,1.46081976924362E-16,0.));
#43727=DIRECTION('ref_axis',(-1.46081976924362E-16,1.,0.));
#43728=DIRECTION('',(-1.46081976924362E-16,1.,0.));
#43729=DIRECTION('center_axis',(-1.,-1.46081976924362E-16,0.));
#43730=DIRECTION('ref_axis',(-1.46081976924362E-16,1.,0.));
#43731=DIRECTION('',(-1.46081976924362E-16,1.,0.));
#43732=DIRECTION('',(-1.46081976924362E-16,1.,0.));
#43733=DIRECTION('center_axis',(-1.,-1.46081976924362E-16,0.));
#43734=DIRECTION('ref_axis',(-1.46081976924362E-16,1.,0.));
#43735=DIRECTION('',(-1.46081976924362E-16,1.,0.));
#43736=DIRECTION('',(-1.46081976924362E-16,1.,0.));
#43737=DIRECTION('center_axis',(-1.,-1.46081976924362E-16,0.));
#43738=DIRECTION('ref_axis',(-1.46081976924362E-16,1.,0.));
#43739=DIRECTION('',(-1.46081976924362E-16,1.,0.));
#43740=DIRECTION('',(-1.46081976924362E-16,1.,0.));
#43741=DIRECTION('center_axis',(-1.,-1.46081976924362E-16,0.));
#43742=DIRECTION('ref_axis',(-1.46081976924362E-16,1.,0.));
#43743=DIRECTION('',(-1.46081976924362E-16,1.,0.));
#43744=DIRECTION('',(1.46081976924362E-16,-1.,0.));
#43745=DIRECTION('center_axis',(1.,1.46081976924362E-16,0.));
#43746=DIRECTION('ref_axis',(-1.46081976924362E-16,1.,0.));
#43747=DIRECTION('',(1.46081976924362E-16,-1.,0.));
#43748=DIRECTION('',(1.46081976924362E-16,-1.,0.));
#43749=DIRECTION('center_axis',(1.,1.46081976924362E-16,0.));
#43750=DIRECTION('ref_axis',(-1.46081976924362E-16,1.,0.));
#43751=DIRECTION('',(1.46081976924362E-16,-1.,0.));
#43752=DIRECTION('',(1.46081976924362E-16,-1.,0.));
#43753=DIRECTION('center_axis',(1.,1.46081976924362E-16,0.));
#43754=DIRECTION('ref_axis',(-1.46081976924362E-16,1.,0.));
#43755=DIRECTION('',(1.46081976924362E-16,-1.,0.));
#43756=DIRECTION('',(1.46081976924362E-16,-1.,0.));
#43757=DIRECTION('center_axis',(1.,1.46081976924362E-16,0.));
#43758=DIRECTION('ref_axis',(-1.46081976924362E-16,1.,0.));
#43759=DIRECTION('',(1.46081976924362E-16,-1.,0.));
#43760=DIRECTION('',(-1.46081976924362E-16,1.,0.));
#43761=DIRECTION('center_axis',(-1.,-1.46081976924362E-16,0.));
#43762=DIRECTION('ref_axis',(-1.46081976924362E-16,1.,0.));
#43763=DIRECTION('',(-1.46081976924362E-16,1.,0.));
#43764=DIRECTION('',(1.46081976924362E-16,-1.,0.));
#43765=DIRECTION('center_axis',(1.,1.46081976924362E-16,0.));
#43766=DIRECTION('ref_axis',(-1.46081976924362E-16,1.,0.));
#43767=DIRECTION('',(1.46081976924362E-16,-1.,0.));
#43768=DIRECTION('',(-1.46081976924362E-16,1.,0.));
#43769=DIRECTION('center_axis',(-1.,-1.46081976924362E-16,0.));
#43770=DIRECTION('ref_axis',(-1.46081976924362E-16,1.,0.));
#43771=DIRECTION('',(-1.46081976924362E-16,1.,0.));
#43772=DIRECTION('center_axis',(-3.79532109154651E-16,0.866025403784439,
0.499999999999999));
#43773=DIRECTION('ref_axis',(-7.94699513894569E-33,-0.499999999999999,0.866025403784439));
#43774=DIRECTION('',(-3.46944695195361E-16,0.499999999999999,-0.866025403784439));
#43775=DIRECTION('',(2.19122965386544E-16,-0.499999999999999,0.866025403784439));
#43776=DIRECTION('',(-1.,-4.38245930773088E-16,0.));
#43777=DIRECTION('center_axis',(-3.79532109154651E-16,0.866025403784439,
0.499999999999999));
#43778=DIRECTION('ref_axis',(-7.94699513894569E-33,-0.499999999999999,0.866025403784439));
#43779=DIRECTION('',(2.19122965386544E-16,-0.499999999999999,0.866025403784439));
#43780=DIRECTION('',(-1.,-4.38245930773088E-16,0.));
#43781=DIRECTION('',(-3.46944695195361E-16,0.499999999999999,-0.866025403784439));
#43782=DIRECTION('center_axis',(3.79532109154651E-16,-0.866025403784439,
-0.499999999999999));
#43783=DIRECTION('ref_axis',(1.5326347767966E-32,0.499999999999999,-0.866025403784439));
#43784=DIRECTION('',(3.46944695195362E-16,-0.499999999999999,0.866025403784439));
#43785=DIRECTION('',(1.,4.38245930773088E-16,0.));
#43786=DIRECTION('',(-2.19122965386544E-16,0.499999999999999,-0.866025403784439));
#43787=DIRECTION('',(-1.,-4.38245930773088E-16,0.));
#43788=DIRECTION('center_axis',(-3.79532109154651E-16,0.866025403784438,
-0.5));
#43789=DIRECTION('ref_axis',(1.94620289117031E-33,0.5,0.866025403784438));
#43790=DIRECTION('',(-2.19122965386544E-16,0.5,0.866025403784438));
#43791=DIRECTION('',(0.,-0.5,-0.866025403784438));
#43792=DIRECTION('',(1.,4.38245930773088E-16,8.64002241377108E-33));
#43793=DIRECTION('center_axis',(3.79532109154651E-16,-0.866025403784438,
0.5));
#43794=DIRECTION('ref_axis',(-1.94620289117031E-33,-0.5,-0.866025403784438));
#43795=DIRECTION('',(0.,0.5,0.866025403784438));
#43796=DIRECTION('',(1.,4.38245930773088E-16,8.64002241377108E-33));
#43797=DIRECTION('',(2.19122965386544E-16,-0.5,-0.866025403784438));
#43798=DIRECTION('',(-1.,-4.38245930773088E-16,-8.64002241377108E-33));
#43799=DIRECTION('center_axis',(0.,0.,-1.));
#43800=DIRECTION('ref_axis',(-1.,0.,0.));
#43801=DIRECTION('',(-4.38245930773088E-16,1.,0.));
#43802=DIRECTION('',(4.38245930773088E-16,-1.,0.));
#43803=DIRECTION('',(1.,4.38245930773088E-16,0.));
#43804=DIRECTION('center_axis',(0.,0.,1.));
#43805=DIRECTION('ref_axis',(1.,0.,0.));
#43806=DIRECTION('',(-4.38245930773088E-16,1.,0.));
#43807=DIRECTION('',(4.38245930773088E-16,-1.,0.));
#43808=DIRECTION('',(-1.,-4.38245930773088E-16,0.));
#43809=DIRECTION('center_axis',(3.79532109154651E-16,-0.866025403784439,
-0.5));
#43810=DIRECTION('ref_axis',(-8.35245407460559E-33,0.5,-0.866025403784439));
#43811=DIRECTION('',(-2.19122965386544E-16,0.5,-0.866025403784439));
#43812=DIRECTION('',(-1.,-4.38245930773088E-16,0.));
#43813=DIRECTION('',(0.,-0.5,0.866025403784439));
#43814=DIRECTION('',(1.,4.38245930773088E-16,0.));
#43815=DIRECTION('center_axis',(3.79532109154651E-16,-0.866025403784438,
0.5));
#43816=DIRECTION('ref_axis',(2.27057003969863E-32,-0.5,-0.866025403784438));
#43817=DIRECTION('',(2.19122965386544E-16,-0.5,-0.866025403784438));
#43818=DIRECTION('',(-1.,-4.38245930773088E-16,0.));
#43819=DIRECTION('',(-3.46944695195361E-16,0.5,0.866025403784438));
#43820=DIRECTION('',(1.,4.38245930773088E-16,0.));
#43821=DIRECTION('center_axis',(-3.79532109154651E-16,0.866025403784439,
-0.5));
#43822=DIRECTION('ref_axis',(-1.08662994757006E-32,0.5,0.866025403784439));
#43823=DIRECTION('',(3.46944695195361E-16,-0.5,-0.866025403784438));
#43824=DIRECTION('',(1.,4.38245930773088E-16,0.));
#43825=DIRECTION('',(-2.19122965386544E-16,0.5,0.866025403784438));
#43826=DIRECTION('center_axis',(0.,0.,1.));
#43827=DIRECTION('ref_axis',(1.,0.,0.));
#43828=DIRECTION('',(4.38245930773088E-16,-1.,0.));
#43829=DIRECTION('',(-1.,-4.38245930773088E-16,0.));
#43830=DIRECTION('',(-4.38245930773088E-16,1.,0.));
#43831=DIRECTION('',(1.,4.38245930773088E-16,0.));
#43832=DIRECTION('center_axis',(0.,0.,-1.));
#43833=DIRECTION('ref_axis',(-1.,0.,0.));
#43834=DIRECTION('',(-4.38245930773088E-16,1.,0.));
#43835=DIRECTION('',(-1.,-4.38245930773088E-16,0.));
#43836=DIRECTION('',(4.38245930773088E-16,-1.,0.));
#43837=DIRECTION('',(1.,4.38245930773088E-16,0.));
#43838=DIRECTION('center_axis',(-3.79532109154651E-16,0.866025403784439,
0.499999999999999));
#43839=DIRECTION('ref_axis',(-7.94699513894569E-33,-0.499999999999999,0.866025403784439));
#43840=DIRECTION('',(-3.46944695195361E-16,0.499999999999999,-0.866025403784439));
#43841=DIRECTION('',(2.19122965386544E-16,-0.499999999999999,0.866025403784439));
#43842=DIRECTION('',(-1.,-4.38245930773088E-16,0.));
#43843=DIRECTION('center_axis',(-3.79532109154651E-16,0.866025403784439,
0.499999999999999));
#43844=DIRECTION('ref_axis',(-7.94699513894569E-33,-0.499999999999999,0.866025403784439));
#43845=DIRECTION('',(2.19122965386544E-16,-0.499999999999999,0.866025403784439));
#43846=DIRECTION('',(-1.,-4.38245930773088E-16,0.));
#43847=DIRECTION('',(-3.46944695195361E-16,0.499999999999999,-0.866025403784439));
#43848=DIRECTION('center_axis',(3.79532109154651E-16,-0.866025403784439,
-0.499999999999999));
#43849=DIRECTION('ref_axis',(1.5326347767966E-32,0.499999999999999,-0.866025403784439));
#43850=DIRECTION('',(3.46944695195362E-16,-0.499999999999999,0.866025403784439));
#43851=DIRECTION('',(1.,4.38245930773088E-16,0.));
#43852=DIRECTION('',(-2.19122965386544E-16,0.499999999999999,-0.866025403784439));
#43853=DIRECTION('',(-1.,-4.38245930773088E-16,0.));
#43854=DIRECTION('center_axis',(-3.79532109154651E-16,0.866025403784438,
-0.5));
#43855=DIRECTION('ref_axis',(1.94620289117031E-33,0.5,0.866025403784438));
#43856=DIRECTION('',(-2.19122965386544E-16,0.5,0.866025403784438));
#43857=DIRECTION('',(0.,-0.5,-0.866025403784438));
#43858=DIRECTION('',(1.,4.38245930773088E-16,8.64002241377108E-33));
#43859=DIRECTION('center_axis',(3.79532109154651E-16,-0.866025403784438,
0.5));
#43860=DIRECTION('ref_axis',(-1.94620289117031E-33,-0.5,-0.866025403784438));
#43861=DIRECTION('',(0.,0.5,0.866025403784438));
#43862=DIRECTION('',(1.,4.38245930773088E-16,6.16297582203917E-33));
#43863=DIRECTION('',(2.19122965386544E-16,-0.5,-0.866025403784438));
#43864=DIRECTION('',(-1.,-4.38245930773088E-16,-8.64002241377108E-33));
#43865=DIRECTION('center_axis',(0.,0.,-1.));
#43866=DIRECTION('ref_axis',(-1.,0.,0.));
#43867=DIRECTION('',(-4.38245930773088E-16,1.,0.));
#43868=DIRECTION('',(4.38245930773088E-16,-1.,0.));
#43869=DIRECTION('',(1.,4.38245930773088E-16,0.));
#43870=DIRECTION('center_axis',(0.,0.,1.));
#43871=DIRECTION('ref_axis',(1.,0.,0.));
#43872=DIRECTION('',(-4.38245930773088E-16,1.,0.));
#43873=DIRECTION('',(4.38245930773088E-16,-1.,0.));
#43874=DIRECTION('',(-1.,-4.38245930773088E-16,0.));
#43875=DIRECTION('center_axis',(3.79532109154651E-16,-0.866025403784439,
-0.5));
#43876=DIRECTION('ref_axis',(-8.35245407460559E-33,0.5,-0.866025403784439));
#43877=DIRECTION('',(-2.19122965386544E-16,0.5,-0.866025403784439));
#43878=DIRECTION('',(-1.,-4.38245930773088E-16,0.));
#43879=DIRECTION('',(0.,-0.5,0.866025403784439));
#43880=DIRECTION('',(1.,4.38245930773088E-16,0.));
#43881=DIRECTION('center_axis',(3.79532109154651E-16,-0.866025403784438,
0.5));
#43882=DIRECTION('ref_axis',(2.27057003969863E-32,-0.5,-0.866025403784438));
#43883=DIRECTION('',(2.19122965386544E-16,-0.5,-0.866025403784438));
#43884=DIRECTION('',(-1.,-4.38245930773088E-16,0.));
#43885=DIRECTION('',(-3.46944695195361E-16,0.5,0.866025403784438));
#43886=DIRECTION('',(1.,4.38245930773088E-16,0.));
#43887=DIRECTION('center_axis',(-3.79532109154651E-16,0.866025403784439,
-0.5));
#43888=DIRECTION('ref_axis',(-1.08662994757006E-32,0.5,0.866025403784439));
#43889=DIRECTION('',(3.46944695195361E-16,-0.5,-0.866025403784438));
#43890=DIRECTION('',(1.,4.38245930773088E-16,0.));
#43891=DIRECTION('',(-2.19122965386544E-16,0.5,0.866025403784438));
#43892=DIRECTION('center_axis',(0.,0.,1.));
#43893=DIRECTION('ref_axis',(1.,0.,0.));
#43894=DIRECTION('',(4.38245930773088E-16,-1.,0.));
#43895=DIRECTION('',(-1.,-4.38245930773088E-16,0.));
#43896=DIRECTION('',(-4.38245930773088E-16,1.,0.));
#43897=DIRECTION('',(1.,4.38245930773088E-16,0.));
#43898=DIRECTION('center_axis',(0.,0.,-1.));
#43899=DIRECTION('ref_axis',(-1.,0.,0.));
#43900=DIRECTION('',(-4.38245930773088E-16,1.,0.));
#43901=DIRECTION('',(-1.,-4.38245930773088E-16,0.));
#43902=DIRECTION('',(4.38245930773088E-16,-1.,0.));
#43903=DIRECTION('',(1.,4.38245930773088E-16,0.));
#43904=DIRECTION('',(-1.,-4.38245930773088E-16,0.));
#43905=DIRECTION('',(1.,4.38245930773088E-16,0.));
#43906=DIRECTION('center_axis',(-1.,-4.38245930773088E-16,0.));
#43907=DIRECTION('ref_axis',(0.,0.,1.));
#43908=DIRECTION('center_axis',(-1.,-4.38245930773088E-16,0.));
#43909=DIRECTION('ref_axis',(4.38245930773088E-16,-1.,0.));
#43910=DIRECTION('center_axis',(-1.,-4.38245930773088E-16,0.));
#43911=DIRECTION('ref_axis',(4.38245930773088E-16,-1.,0.));
#43912=DIRECTION('center_axis',(-1.,-4.38245930773088E-16,0.));
#43913=DIRECTION('ref_axis',(4.38245930773088E-16,-1.,0.));
#43914=DIRECTION('center_axis',(-1.,-4.38245930773088E-16,0.));
#43915=DIRECTION('ref_axis',(4.38245930773088E-16,-1.,0.));
#43916=DIRECTION('',(2.19122965386544E-16,-0.5,-0.866025403784438));
#43917=DIRECTION('center_axis',(-1.,-4.38245930773088E-16,0.));
#43918=DIRECTION('ref_axis',(4.38245930773088E-16,-1.,0.));
#43919=DIRECTION('center_axis',(-1.,-4.38245930773088E-16,0.));
#43920=DIRECTION('ref_axis',(4.38245930773088E-16,-1.,0.));
#43921=DIRECTION('',(2.19122965386544E-16,-0.499999999999999,0.866025403784439));
#43922=DIRECTION('',(4.38245930773088E-16,-1.,0.));
#43923=DIRECTION('center_axis',(-1.,-4.38245930773088E-16,0.));
#43924=DIRECTION('ref_axis',(4.38245930773088E-16,-1.,0.));
#43925=DIRECTION('',(-2.19122965386544E-16,0.5,0.866025403784438));
#43926=DIRECTION('center_axis',(-1.,-4.38245930773088E-16,0.));
#43927=DIRECTION('ref_axis',(4.38245930773088E-16,-1.,0.));
#43928=DIRECTION('center_axis',(-1.,-4.38245930773088E-16,0.));
#43929=DIRECTION('ref_axis',(4.38245930773088E-16,-1.,0.));
#43930=DIRECTION('',(2.19122965386544E-16,-0.499999999999999,0.866025403784439));
#43931=DIRECTION('center_axis',(-1.,-4.38245930773088E-16,0.));
#43932=DIRECTION('ref_axis',(4.38245930773088E-16,-1.,0.));
#43933=DIRECTION('',(-4.38245930773088E-16,1.,0.));
#43934=DIRECTION('center_axis',(-1.,-4.38245930773088E-16,0.));
#43935=DIRECTION('ref_axis',(4.38245930773088E-16,-1.,0.));
#43936=DIRECTION('center_axis',(-1.,-4.38245930773088E-16,0.));
#43937=DIRECTION('ref_axis',(4.38245930773088E-16,-1.,0.));
#43938=DIRECTION('',(-2.19122965386544E-16,0.5,0.866025403784438));
#43939=DIRECTION('center_axis',(-1.,-4.38245930773088E-16,0.));
#43940=DIRECTION('ref_axis',(4.38245930773088E-16,-1.,0.));
#43941=DIRECTION('center_axis',(-1.,-4.38245930773088E-16,0.));
#43942=DIRECTION('ref_axis',(4.38245930773088E-16,-1.,0.));
#43943=DIRECTION('',(-2.19122965386544E-16,0.499999999999999,-0.866025403784439));
#43944=DIRECTION('center_axis',(-1.,-4.38245930773088E-16,0.));
#43945=DIRECTION('ref_axis',(4.38245930773088E-16,-1.,0.));
#43946=DIRECTION('',(-4.38245930773088E-16,1.,0.));
#43947=DIRECTION('center_axis',(-1.,-4.38245930773088E-16,0.));
#43948=DIRECTION('ref_axis',(4.38245930773088E-16,-1.,0.));
#43949=DIRECTION('center_axis',(-1.,-4.38245930773088E-16,0.));
#43950=DIRECTION('ref_axis',(4.38245930773088E-16,-1.,0.));
#43951=DIRECTION('',(2.19122965386544E-16,-0.5,-0.866025403784438));
#43952=DIRECTION('center_axis',(-1.,-4.38245930773088E-16,0.));
#43953=DIRECTION('ref_axis',(4.38245930773088E-16,-1.,0.));
#43954=DIRECTION('',(-2.19122965386544E-16,0.5,-0.866025403784439));
#43955=DIRECTION('center_axis',(-1.,-4.38245930773088E-16,0.));
#43956=DIRECTION('ref_axis',(4.38245930773088E-16,-1.,0.));
#43957=DIRECTION('center_axis',(-1.,-4.38245930773088E-16,0.));
#43958=DIRECTION('ref_axis',(4.38245930773088E-16,-1.,0.));
#43959=DIRECTION('',(4.38245930773088E-16,-1.,0.));
#43960=DIRECTION('center_axis',(-1.,-4.38245930773088E-16,0.));
#43961=DIRECTION('ref_axis',(4.38245930773088E-16,-1.,0.));
#43962=DIRECTION('center_axis',(-1.,-4.38245930773088E-16,0.));
#43963=DIRECTION('ref_axis',(4.38245930773088E-16,-1.,0.));
#43964=DIRECTION('center_axis',(-1.,-4.38245930773088E-16,0.));
#43965=DIRECTION('ref_axis',(4.38245930773088E-16,-1.,0.));
#43966=DIRECTION('center_axis',(-1.,-4.38245930773088E-16,0.));
#43967=DIRECTION('ref_axis',(4.38245930773088E-16,-1.,0.));
#43968=DIRECTION('center_axis',(-1.,-4.38245930773088E-16,0.));
#43969=DIRECTION('ref_axis',(4.38245930773088E-16,-1.,0.));
#43970=DIRECTION('center_axis',(-1.,-4.38245930773088E-16,0.));
#43971=DIRECTION('ref_axis',(4.38245930773088E-16,-1.,0.));
#43972=DIRECTION('center_axis',(-1.,-4.38245930773088E-16,0.));
#43973=DIRECTION('ref_axis',(4.38245930773088E-16,-1.,0.));
#43974=DIRECTION('center_axis',(-1.,-4.38245930773088E-16,0.));
#43975=DIRECTION('ref_axis',(4.38245930773088E-16,-1.,0.));
#43976=DIRECTION('center_axis',(-1.,-4.38245930773088E-16,0.));
#43977=DIRECTION('ref_axis',(4.38245930773088E-16,-1.,0.));
#43978=DIRECTION('center_axis',(-1.,-4.38245930773088E-16,0.));
#43979=DIRECTION('ref_axis',(4.38245930773088E-16,-1.,0.));
#43980=DIRECTION('center_axis',(-1.,-4.38245930773088E-16,0.));
#43981=DIRECTION('ref_axis',(4.38245930773088E-16,-1.,0.));
#43982=DIRECTION('center_axis',(-1.,-4.38245930773088E-16,0.));
#43983=DIRECTION('ref_axis',(4.38245930773088E-16,-1.,0.));
#43984=DIRECTION('center_axis',(-1.,-4.38245930773088E-16,0.));
#43985=DIRECTION('ref_axis',(4.38245930773088E-16,-1.,0.));
#43986=DIRECTION('center_axis',(-1.,-4.38245930773088E-16,0.));
#43987=DIRECTION('ref_axis',(4.38245930773088E-16,-1.,0.));
#43988=DIRECTION('center_axis',(-1.,-4.38245930773088E-16,0.));
#43989=DIRECTION('ref_axis',(4.38245930773088E-16,-1.,0.));
#43990=DIRECTION('center_axis',(-1.,-4.38245930773088E-16,0.));
#43991=DIRECTION('ref_axis',(4.38245930773088E-16,-1.,0.));
#43992=DIRECTION('center_axis',(-1.,-4.38245930773088E-16,0.));
#43993=DIRECTION('ref_axis',(4.38245930773088E-16,-1.,0.));
#43994=DIRECTION('center_axis',(-1.,-4.38245930773088E-16,0.));
#43995=DIRECTION('ref_axis',(4.38245930773088E-16,-1.,0.));
#43996=DIRECTION('center_axis',(-1.,-4.38245930773088E-16,0.));
#43997=DIRECTION('ref_axis',(4.38245930773088E-16,-1.,0.));
#43998=DIRECTION('center_axis',(-1.,-4.38245930773088E-16,0.));
#43999=DIRECTION('ref_axis',(4.38245930773088E-16,-1.,0.));
#44000=DIRECTION('center_axis',(-1.,-4.38245930773088E-16,0.));
#44001=DIRECTION('ref_axis',(4.38245930773088E-16,-1.,0.));
#44002=DIRECTION('center_axis',(-1.,-4.38245930773088E-16,0.));
#44003=DIRECTION('ref_axis',(4.38245930773088E-16,-1.,0.));
#44004=DIRECTION('center_axis',(-1.,-4.38245930773088E-16,0.));
#44005=DIRECTION('ref_axis',(4.38245930773088E-16,-1.,0.));
#44006=DIRECTION('center_axis',(-1.,-4.38245930773088E-16,0.));
#44007=DIRECTION('ref_axis',(4.38245930773088E-16,-1.,0.));
#44008=DIRECTION('center_axis',(-1.,-4.38245930773088E-16,0.));
#44009=DIRECTION('ref_axis',(4.38245930773088E-16,-1.,0.));
#44010=DIRECTION('center_axis',(-1.,-4.38245930773088E-16,0.));
#44011=DIRECTION('ref_axis',(4.38245930773088E-16,-1.,0.));
#44012=DIRECTION('center_axis',(-1.,-4.38245930773088E-16,0.));
#44013=DIRECTION('ref_axis',(4.38245930773088E-16,-1.,0.));
#44014=DIRECTION('center_axis',(-1.,-4.38245930773088E-16,0.));
#44015=DIRECTION('ref_axis',(4.38245930773088E-16,-1.,0.));
#44016=DIRECTION('center_axis',(-1.,-4.38245930773088E-16,0.));
#44017=DIRECTION('ref_axis',(4.38245930773088E-16,-1.,0.));
#44018=DIRECTION('center_axis',(-1.,-4.38245930773088E-16,0.));
#44019=DIRECTION('ref_axis',(4.38245930773088E-16,-1.,0.));
#44020=DIRECTION('center_axis',(-1.,-4.38245930773088E-16,0.));
#44021=DIRECTION('ref_axis',(4.38245930773088E-16,-1.,0.));
#44022=DIRECTION('center_axis',(-1.,-4.38245930773088E-16,0.));
#44023=DIRECTION('ref_axis',(4.38245930773088E-16,-1.,0.));
#44024=DIRECTION('center_axis',(-1.,-4.38245930773088E-16,0.));
#44025=DIRECTION('ref_axis',(4.38245930773088E-16,-1.,0.));
#44026=DIRECTION('center_axis',(-1.,-4.38245930773088E-16,0.));
#44027=DIRECTION('ref_axis',(4.38245930773088E-16,-1.,0.));
#44028=DIRECTION('center_axis',(-3.79532109154651E-16,0.866025403784439,
0.499999999999999));
#44029=DIRECTION('ref_axis',(-7.94699513894569E-33,-0.499999999999999,0.866025403784439));
#44030=DIRECTION('',(-3.46944695195361E-16,0.499999999999999,-0.866025403784439));
#44031=DIRECTION('',(-1.,-4.38245930773088E-16,0.));
#44032=DIRECTION('',(1.,4.38245930773088E-16,0.));
#44033=DIRECTION('',(-1.,-4.38245930773088E-16,0.));
#44034=DIRECTION('',(-1.,-4.38245930773088E-16,0.));
#44035=DIRECTION('center_axis',(-1.,-4.38245930773088E-16,0.));
#44036=DIRECTION('ref_axis',(4.38245930773088E-16,-1.,0.));
#44037=DIRECTION('',(0.,0.,-1.));
#44038=DIRECTION('',(3.09886669477061E-16,-0.707106781186547,-0.707106781186547));
#44039=DIRECTION('',(-4.38245930773088E-16,1.,0.));
#44040=DIRECTION('',(0.,0.,-1.));
#44041=DIRECTION('center_axis',(-1.,-4.38245930773088E-16,0.));
#44042=DIRECTION('ref_axis',(4.38245930773088E-16,-1.,0.));
#44043=DIRECTION('',(0.,0.,-1.));
#44044=DIRECTION('center_axis',(-1.,-4.38245930773088E-16,0.));
#44045=DIRECTION('ref_axis',(4.38245930773088E-16,-1.,0.));
#44046=DIRECTION('',(0.,0.,-1.));
#44047=DIRECTION('',(-4.38245930773088E-16,1.,0.));
#44048=DIRECTION('',(-3.09886669477061E-16,0.707106781186547,-0.707106781186547));
#44049=DIRECTION('',(0.,2.77555756156289E-15,1.));
#44050=DIRECTION('',(0.,-1.,0.));
#44051=DIRECTION('',(0.,-4.16333634234433E-15,-1.));
#44052=DIRECTION('',(0.,1.,0.));
#44053=DIRECTION('center_axis',(-1.,-4.38245930773088E-16,0.));
#44054=DIRECTION('ref_axis',(4.38245930773088E-16,-1.,0.));
#44055=DIRECTION('',(0.,1.,0.));
#44056=DIRECTION('center_axis',(-1.,-4.38245930773088E-16,0.));
#44057=DIRECTION('ref_axis',(4.38245930773088E-16,-1.,0.));
#44058=DIRECTION('',(0.,0.707106781186552,0.707106781186543));
#44059=DIRECTION('center_axis',(-1.,-4.38245930773088E-16,0.));
#44060=DIRECTION('ref_axis',(4.38245930773088E-16,-1.,0.));
#44061=DIRECTION('',(0.,1.8333618114597E-15,1.));
#44062=DIRECTION('center_axis',(-1.,-4.38245930773088E-16,0.));
#44063=DIRECTION('ref_axis',(4.38245930773088E-16,-1.,0.));
#44064=DIRECTION('',(0.,-0.707106781186551,0.707106781186544));
#44065=DIRECTION('center_axis',(-1.,-4.38245930773088E-16,0.));
#44066=DIRECTION('ref_axis',(4.38245930773088E-16,-1.,0.));
#44067=DIRECTION('',(0.,-1.,-1.3325595315168E-15));
#44068=DIRECTION('center_axis',(-1.,-4.38245930773088E-16,0.));
#44069=DIRECTION('ref_axis',(4.38245930773088E-16,-1.,0.));
#44070=DIRECTION('',(0.,0.,-1.));
#44071=DIRECTION('center_axis',(-1.,-4.38245930773088E-16,0.));
#44072=DIRECTION('ref_axis',(4.38245930773088E-16,-1.,0.));
#44073=DIRECTION('',(-4.38245930773088E-16,1.,0.));
#44074=DIRECTION('',(-3.09886669477061E-16,0.707106781186547,0.707106781186547));
#44075=DIRECTION('',(0.,0.,-1.));
#44076=DIRECTION('',(3.09886669477061E-16,-0.707106781186547,0.707106781186547));
#44077=DIRECTION('',(-4.38245930773088E-16,1.,0.));
#44078=DIRECTION('',(0.,0.,1.));
#44079=DIRECTION('center_axis',(-1.,-4.38245930773088E-16,0.));
#44080=DIRECTION('ref_axis',(4.38245930773088E-16,-1.,0.));
#44081=DIRECTION('',(0.,0.,-1.));
#44082=DIRECTION('center_axis',(1.,6.12323399573677E-17,0.));
#44083=DIRECTION('ref_axis',(0.,0.,1.));
#44084=DIRECTION('',(0.,0.,1.));
#44085=DIRECTION('',(4.38245930773088E-16,-1.,0.));
#44086=DIRECTION('',(-1.21637680698141E-30,2.77555756156289E-15,1.));
#44087=DIRECTION('',(-4.38245930773088E-16,1.,0.));
#44088=DIRECTION('',(1.82456521047212E-30,-4.16333634234433E-15,-1.));
#44089=DIRECTION('',(-4.38245930773088E-16,1.,0.));
#44090=DIRECTION('center_axis',(-1.,-4.38245930773088E-16,0.));
#44091=DIRECTION('ref_axis',(4.38245930773088E-16,-1.,0.));
#44092=DIRECTION('',(0.,0.,-1.));
#44093=DIRECTION('center_axis',(-1.,-4.38245930773088E-16,0.));
#44094=DIRECTION('ref_axis',(4.38245930773088E-16,-1.,0.));
#44095=DIRECTION('',(4.38245930773088E-16,-1.,-1.3325595315168E-15));
#44096=DIRECTION('center_axis',(-1.,-4.38245930773088E-16,0.));
#44097=DIRECTION('ref_axis',(4.38245930773088E-16,-1.,0.));
#44098=DIRECTION('',(3.09886669477062E-16,-0.707106781186551,0.707106781186544));
#44099=DIRECTION('center_axis',(-1.,-4.38245930773088E-16,0.));
#44100=DIRECTION('ref_axis',(4.38245930773088E-16,-1.,0.));
#44101=DIRECTION('',(-8.03463353506993E-31,1.8333618114597E-15,1.));
#44102=DIRECTION('center_axis',(-1.,-4.38245930773088E-16,0.));
#44103=DIRECTION('ref_axis',(4.38245930773088E-16,-1.,0.));
#44104=DIRECTION('',(-3.09886669477063E-16,0.707106781186552,0.707106781186543));
#44105=DIRECTION('center_axis',(-1.,-4.38245930773088E-16,0.));
#44106=DIRECTION('ref_axis',(4.38245930773088E-16,-1.,0.));
#44107=DIRECTION('center_axis',(0.,1.,0.));
#44108=DIRECTION('ref_axis',(0.,0.,1.));
#44109=DIRECTION('',(0.,-1.,-1.11022302462516E-14));
#44110=DIRECTION('',(0.,1.,0.));
#44111=DIRECTION('',(0.,-1.,-1.11022302462516E-14));
#44112=DIRECTION('center_axis',(-1.,0.,0.));
#44113=DIRECTION('ref_axis',(0.,0.,1.));
#44114=DIRECTION('center_axis',(0.,1.,0.));
#44115=DIRECTION('ref_axis',(0.,0.,1.));
#44116=DIRECTION('',(0.,1.,0.));
#44117=DIRECTION('',(0.,1.,0.));
#44118=DIRECTION('',(0.,1.,0.));
#44119=DIRECTION('center_axis',(-1.,0.,0.));
#44120=DIRECTION('ref_axis',(0.,0.,1.));
#44121=DIRECTION('center_axis',(0.,1.,0.));
#44122=DIRECTION('ref_axis',(0.,0.,1.));
#44123=DIRECTION('',(-2.22044604925031E-14,-1.,-2.22044604925031E-14));
#44124=DIRECTION('',(0.,1.,0.));
#44125=DIRECTION('',(-2.22044604925031E-14,-1.,-2.22044604925031E-14));
#44126=DIRECTION('center_axis',(1.,0.,0.));
#44127=DIRECTION('ref_axis',(0.,0.,-1.));
#44128=DIRECTION('center_axis',(0.,1.,0.));
#44129=DIRECTION('ref_axis',(0.,0.,1.));
#44130=DIRECTION('',(0.,1.,0.));
#44131=DIRECTION('',(0.,1.,0.));
#44132=DIRECTION('',(0.,1.,0.));
#44133=DIRECTION('center_axis',(1.,0.,0.));
#44134=DIRECTION('ref_axis',(0.,0.,-1.));
#44135=DIRECTION('',(-1.,0.,0.));
#44136=DIRECTION('',(-1.,0.,0.));
#44137=DIRECTION('',(1.,-1.42247325030098E-14,4.44089209850062E-14));
#44138=DIRECTION('',(1.,-1.42247325030098E-14,4.44089209850062E-14));
#44139=DIRECTION('center_axis',(0.,0.,-1.));
#44140=DIRECTION('ref_axis',(-1.,0.,0.));
#44141=DIRECTION('center_axis',(0.,0.,-1.));
#44142=DIRECTION('ref_axis',(-1.,0.,0.));
#44143=DIRECTION('center_axis',(-6.12323399573677E-17,1.,0.));
#44144=DIRECTION('ref_axis',(0.,0.,1.));
#44145=DIRECTION('',(1.,6.12323399573677E-17,0.));
#44146=DIRECTION('',(1.,6.12323399573677E-17,0.));
#44147=DIRECTION('center_axis',(0.,0.,-1.));
#44148=DIRECTION('ref_axis',(-1.,0.,0.));
#44149=DIRECTION('',(1.,0.,0.));
#44150=DIRECTION('center_axis',(0.,1.,0.));
#44151=DIRECTION('ref_axis',(0.,0.,1.));
#44152=DIRECTION('',(-1.,0.,0.));
#44153=DIRECTION('',(1.,0.,0.));
#44154=DIRECTION('center_axis',(0.,0.,1.));
#44155=DIRECTION('ref_axis',(1.,0.,0.));
#44156=DIRECTION('',(-1.,0.,0.));
#44157=DIRECTION('',(-1.,-6.12323399573677E-17,0.));
#44158=DIRECTION('center_axis',(-6.12323399573677E-17,1.,0.));
#44159=DIRECTION('ref_axis',(0.,0.,1.));
#44160=DIRECTION('',(1.,6.12323399573677E-17,0.));
#44161=DIRECTION('center_axis',(1.,6.12323399573677E-17,0.));
#44162=DIRECTION('ref_axis',(0.,0.,1.));
#44163=DIRECTION('center_axis',(1.,6.12323399573677E-17,0.));
#44164=DIRECTION('ref_axis',(0.,0.,1.));
#44165=DIRECTION('',(-1.,0.,1.11022302462514E-14));
#44166=DIRECTION('',(-1.,0.,1.11022302462514E-14));
#44167=DIRECTION('',(1.,-1.73472347597679E-15,1.11022302462514E-14));
#44168=DIRECTION('',(1.,-1.73472347597679E-15,1.11022302462514E-14));
#44169=DIRECTION('center_axis',(0.,0.,1.));
#44170=DIRECTION('ref_axis',(1.,0.,0.));
#44171=DIRECTION('center_axis',(0.,0.,1.));
#44172=DIRECTION('ref_axis',(1.,0.,0.));
#44173=DIRECTION('center_axis',(-8.82055185704388E-15,1.,0.));
#44174=DIRECTION('ref_axis',(0.,0.,-1.));
#44175=DIRECTION('',(1.,8.82055185704388E-15,0.));
#44176=DIRECTION('',(-1.,-8.82055185704388E-15,0.));
#44177=DIRECTION('center_axis',(0.,0.,-1.));
#44178=DIRECTION('ref_axis',(-1.,0.,0.));
#44179=DIRECTION('',(-1.,0.,0.));
#44180=DIRECTION('center_axis',(0.,1.,0.));
#44181=DIRECTION('ref_axis',(0.,0.,1.));
#44182=DIRECTION('',(-1.,0.,0.));
#44183=DIRECTION('',(1.,0.,0.));
#44184=DIRECTION('center_axis',(0.,0.,-1.));
#44185=DIRECTION('ref_axis',(-1.,0.,0.));
#44186=DIRECTION('',(1.,0.,0.));
#44187=DIRECTION('',(1.,8.82055185704388E-15,0.));
#44188=DIRECTION('center_axis',(-8.82055185704388E-15,1.,0.));
#44189=DIRECTION('ref_axis',(0.,0.,-1.));
#44190=DIRECTION('',(-1.,-8.82055185704388E-15,0.));
#44191=DIRECTION('center_axis',(-1.,-8.82055185704388E-15,0.));
#44192=DIRECTION('ref_axis',(0.,0.,1.));
#44193=DIRECTION('center_axis',(-1.,-8.82055185704388E-15,0.));
#44194=DIRECTION('ref_axis',(0.,0.,1.));
#44195=DIRECTION('center_axis',(0.,0.,1.));
#44196=DIRECTION('ref_axis',(1.,0.,0.));
#44197=DIRECTION('center_axis',(0.,0.,1.));
#44198=DIRECTION('ref_axis',(1.,0.,0.));
#44199=DIRECTION('center_axis',(0.,0.,1.));
#44200=DIRECTION('ref_axis',(1.,0.,0.));
#44201=DIRECTION('center_axis',(0.,0.,1.));
#44202=DIRECTION('ref_axis',(1.,0.,0.));
#44203=DIRECTION('center_axis',(0.,0.,-1.));
#44204=DIRECTION('ref_axis',(1.,-8.67361737988403E-16,0.));
#44205=DIRECTION('center_axis',(0.,0.,-1.));
#44206=DIRECTION('ref_axis',(1.,8.67361737988403E-16,0.));
#44207=DIRECTION('center_axis',(0.,0.,1.));
#44208=DIRECTION('ref_axis',(1.,0.,0.));
#44209=DIRECTION('center_axis',(0.,0.,1.));
#44210=DIRECTION('ref_axis',(1.,0.,0.));
#44211=DIRECTION('',(0.,0.,1.));
#44212=DIRECTION('center_axis',(0.,0.,-1.));
#44213=DIRECTION('ref_axis',(1.,8.67361737988403E-16,0.));
#44214=DIRECTION('center_axis',(0.,0.,1.));
#44215=DIRECTION('ref_axis',(1.,0.,0.));
#44216=DIRECTION('center_axis',(0.,0.,-1.));
#44217=DIRECTION('ref_axis',(1.,-3.18755438710738E-14,0.));
#44218=DIRECTION('',(0.,0.,-1.));
#44219=DIRECTION('center_axis',(0.,0.,1.));
#44220=DIRECTION('ref_axis',(1.,0.,0.));
#44221=DIRECTION('center_axis',(0.,0.,-1.));
#44222=DIRECTION('ref_axis',(-1.,0.,0.));
#44223=DIRECTION('center_axis',(0.,0.,-1.));
#44224=DIRECTION('ref_axis',(1.,-7.2280144832367E-16,0.));
#44225=DIRECTION('',(-0.42443387623072,-0.905458935958868,0.));
#44226=DIRECTION('center_axis',(0.,0.,1.));
#44227=DIRECTION('ref_axis',(1.,0.,0.));
#44228=DIRECTION('',(-1.,0.,0.));
#44229=DIRECTION('center_axis',(0.,0.,1.));
#44230=DIRECTION('ref_axis',(1.,0.,0.));
#44231=DIRECTION('',(-0.42443387623072,0.905458935958868,0.));
#44232=DIRECTION('center_axis',(0.,0.,-1.));
#44233=DIRECTION('ref_axis',(1.,-3.61400724161833E-15,0.));
#44234=DIRECTION('',(-0.424433876230721,0.905458935958868,0.));
#44235=DIRECTION('center_axis',(0.,0.,1.));
#44236=DIRECTION('ref_axis',(1.,0.,0.));
#44237=DIRECTION('',(-1.,0.,0.));
#44238=DIRECTION('center_axis',(0.,0.,1.));
#44239=DIRECTION('ref_axis',(1.,0.,0.));
#44240=DIRECTION('',(-0.424433876230721,-0.905458935958868,0.));
#44241=DIRECTION('center_axis',(0.,0.,-1.));
#44242=DIRECTION('ref_axis',(-0.42443387623072,-0.905458935958868,0.));
#44243=DIRECTION('center_axis',(0.,0.,1.));
#44244=DIRECTION('ref_axis',(1.,0.,0.));
#44245=DIRECTION('',(-0.42443387623072,0.905458935958868,0.));
#44246=DIRECTION('center_axis',(0.,0.,-1.));
#44247=DIRECTION('ref_axis',(1.,1.15648231731787E-14,0.));
#44248=DIRECTION('',(-1.,0.,0.));
#44249=DIRECTION('center_axis',(0.,0.,-1.));
#44250=DIRECTION('ref_axis',(1.,-1.73472347597681E-15,0.));
#44251=DIRECTION('',(-0.42443387623072,-0.905458935958868,0.));
#44252=DIRECTION('center_axis',(0.,0.,1.));
#44253=DIRECTION('ref_axis',(1.,0.,0.));
#44254=DIRECTION('',(-0.424433876230721,-0.905458935958868,0.));
#44255=DIRECTION('center_axis',(0.,0.,-1.));
#44256=DIRECTION('ref_axis',(1.,0.,0.));
#44257=DIRECTION('',(-1.,0.,0.));
#44258=DIRECTION('center_axis',(0.,0.,-1.));
#44259=DIRECTION('ref_axis',(1.,1.69701209606427E-15,0.));
#44260=DIRECTION('',(-0.42443387623072,0.905458935958868,0.));
#44261=DIRECTION('center_axis',(0.,0.,1.));
#44262=DIRECTION('ref_axis',(1.,0.,0.));
#44263=DIRECTION('',(0.,0.,1.));
#44264=DIRECTION('',(0.,0.,-1.));
#44265=DIRECTION('center_axis',(0.,0.,1.));
#44266=DIRECTION('ref_axis',(1.,0.,0.));
#44267=DIRECTION('',(0.,0.,1.));
#44268=DIRECTION('',(0.,0.,-1.));
#44269=DIRECTION('center_axis',(-0.905458935958868,0.42443387623072,0.));
#44270=DIRECTION('ref_axis',(-0.42443387623072,-0.905458935958868,0.));
#44271=DIRECTION('center_axis',(0.905458935958868,0.42443387623072,0.));
#44272=DIRECTION('ref_axis',(-0.42443387623072,0.905458935958868,0.));
#44273=DIRECTION('center_axis',(0.,1.,0.));
#44274=DIRECTION('ref_axis',(0.,0.,1.));
#44275=DIRECTION('center_axis',(0.,0.,1.));
#44276=DIRECTION('ref_axis',(1.,0.,0.));
#44277=DIRECTION('',(0.,0.,-1.));
#44278=DIRECTION('',(0.,0.,1.));
#44279=DIRECTION('center_axis',(0.,0.,1.));
#44280=DIRECTION('ref_axis',(1.,0.,0.));
#44281=DIRECTION('',(0.,0.,-1.));
#44282=DIRECTION('',(0.,0.,1.));
#44283=DIRECTION('center_axis',(0.,0.,1.));
#44284=DIRECTION('ref_axis',(1.,0.,0.));
#44285=DIRECTION('',(0.,0.,-1.));
#44286=DIRECTION('center_axis',(0.,0.,1.));
#44287=DIRECTION('ref_axis',(1.,0.,0.));
#44288=DIRECTION('',(0.,0.,1.));
#44289=DIRECTION('center_axis',(-0.905458935958868,0.42443387623072,0.));
#44290=DIRECTION('ref_axis',(-0.42443387623072,-0.905458935958868,0.));
#44291=DIRECTION('center_axis',(0.905458935958868,0.42443387623072,0.));
#44292=DIRECTION('ref_axis',(-0.42443387623072,0.905458935958868,0.));
#44293=DIRECTION('center_axis',(0.,1.,0.));
#44294=DIRECTION('ref_axis',(0.,0.,1.));
#44295=DIRECTION('center_axis',(0.,0.,1.));
#44296=DIRECTION('ref_axis',(1.,0.,0.));
#44297=DIRECTION('center_axis',(0.,0.,1.));
#44298=DIRECTION('ref_axis',(1.,0.,0.));
#44299=DIRECTION('center_axis',(0.,0.,1.));
#44300=DIRECTION('ref_axis',(1.,0.,0.));
#44301=DIRECTION('center_axis',(0.,0.,1.));
#44302=DIRECTION('ref_axis',(1.,0.,0.));
#44303=DIRECTION('center_axis',(0.,0.,-1.));
#44304=DIRECTION('ref_axis',(1.,-8.67361737988403E-16,0.));
#44305=DIRECTION('center_axis',(0.,0.,-1.));
#44306=DIRECTION('ref_axis',(1.,8.67361737988403E-16,0.));
#44307=DIRECTION('center_axis',(0.,0.,1.));
#44308=DIRECTION('ref_axis',(1.,0.,0.));
#44309=DIRECTION('center_axis',(0.,0.,1.));
#44310=DIRECTION('ref_axis',(1.,0.,0.));
#44311=DIRECTION('',(0.,0.,1.));
#44312=DIRECTION('center_axis',(0.,0.,-1.));
#44313=DIRECTION('ref_axis',(1.,8.67361737988403E-16,0.));
#44314=DIRECTION('center_axis',(0.,0.,1.));
#44315=DIRECTION('ref_axis',(1.,0.,0.));
#44316=DIRECTION('center_axis',(0.,0.,-1.));
#44317=DIRECTION('ref_axis',(1.,-3.18755438710738E-14,0.));
#44318=DIRECTION('',(0.,0.,-1.));
#44319=DIRECTION('center_axis',(0.,0.,1.));
#44320=DIRECTION('ref_axis',(1.,0.,0.));
#44321=DIRECTION('center_axis',(0.,0.,-1.));
#44322=DIRECTION('ref_axis',(-1.,0.,0.));
#44323=DIRECTION('center_axis',(0.,0.,-1.));
#44324=DIRECTION('ref_axis',(1.,-7.2280144832367E-16,0.));
#44325=DIRECTION('',(-0.42443387623072,-0.905458935958868,0.));
#44326=DIRECTION('center_axis',(0.,0.,1.));
#44327=DIRECTION('ref_axis',(1.,0.,0.));
#44328=DIRECTION('',(-1.,0.,0.));
#44329=DIRECTION('center_axis',(0.,0.,1.));
#44330=DIRECTION('ref_axis',(1.,0.,0.));
#44331=DIRECTION('',(-0.42443387623072,0.905458935958868,0.));
#44332=DIRECTION('center_axis',(0.,0.,-1.));
#44333=DIRECTION('ref_axis',(1.,-3.61400724161833E-15,0.));
#44334=DIRECTION('',(-0.424433876230721,0.905458935958868,0.));
#44335=DIRECTION('center_axis',(0.,0.,1.));
#44336=DIRECTION('ref_axis',(1.,0.,0.));
#44337=DIRECTION('',(-1.,0.,0.));
#44338=DIRECTION('center_axis',(0.,0.,1.));
#44339=DIRECTION('ref_axis',(1.,0.,0.));
#44340=DIRECTION('',(-0.424433876230721,-0.905458935958868,0.));
#44341=DIRECTION('center_axis',(0.,0.,-1.));
#44342=DIRECTION('ref_axis',(-0.42443387623072,-0.905458935958868,0.));
#44343=DIRECTION('center_axis',(0.,0.,1.));
#44344=DIRECTION('ref_axis',(1.,0.,0.));
#44345=DIRECTION('',(-0.42443387623072,0.905458935958868,0.));
#44346=DIRECTION('center_axis',(0.,0.,-1.));
#44347=DIRECTION('ref_axis',(1.,1.15648231731787E-14,0.));
#44348=DIRECTION('',(-1.,0.,0.));
#44349=DIRECTION('center_axis',(0.,0.,-1.));
#44350=DIRECTION('ref_axis',(1.,-1.73472347597681E-15,0.));
#44351=DIRECTION('',(-0.42443387623072,-0.905458935958868,0.));
#44352=DIRECTION('center_axis',(0.,0.,1.));
#44353=DIRECTION('ref_axis',(1.,0.,0.));
#44354=DIRECTION('',(-0.424433876230721,-0.905458935958868,0.));
#44355=DIRECTION('center_axis',(0.,0.,-1.));
#44356=DIRECTION('ref_axis',(1.,0.,0.));
#44357=DIRECTION('',(-1.,0.,0.));
#44358=DIRECTION('center_axis',(0.,0.,-1.));
#44359=DIRECTION('ref_axis',(1.,1.69701209606427E-15,0.));
#44360=DIRECTION('',(-0.42443387623072,0.905458935958868,0.));
#44361=DIRECTION('center_axis',(0.,0.,1.));
#44362=DIRECTION('ref_axis',(1.,0.,0.));
#44363=DIRECTION('',(0.,0.,1.));
#44364=DIRECTION('',(0.,0.,-1.));
#44365=DIRECTION('center_axis',(0.,0.,1.));
#44366=DIRECTION('ref_axis',(1.,0.,0.));
#44367=DIRECTION('',(0.,0.,1.));
#44368=DIRECTION('',(0.,0.,-1.));
#44369=DIRECTION('center_axis',(-0.905458935958868,0.42443387623072,0.));
#44370=DIRECTION('ref_axis',(-0.42443387623072,-0.905458935958868,0.));
#44371=DIRECTION('center_axis',(0.905458935958868,0.42443387623072,0.));
#44372=DIRECTION('ref_axis',(-0.42443387623072,0.905458935958868,0.));
#44373=DIRECTION('center_axis',(0.,1.,0.));
#44374=DIRECTION('ref_axis',(0.,0.,1.));
#44375=DIRECTION('center_axis',(0.,0.,1.));
#44376=DIRECTION('ref_axis',(1.,0.,0.));
#44377=DIRECTION('',(0.,0.,-1.));
#44378=DIRECTION('',(0.,0.,1.));
#44379=DIRECTION('center_axis',(0.,0.,1.));
#44380=DIRECTION('ref_axis',(1.,0.,0.));
#44381=DIRECTION('',(0.,0.,-1.));
#44382=DIRECTION('',(0.,0.,1.));
#44383=DIRECTION('center_axis',(0.,0.,1.));
#44384=DIRECTION('ref_axis',(1.,0.,0.));
#44385=DIRECTION('',(0.,0.,-1.));
#44386=DIRECTION('center_axis',(0.,0.,1.));
#44387=DIRECTION('ref_axis',(1.,0.,0.));
#44388=DIRECTION('',(0.,0.,1.));
#44389=DIRECTION('center_axis',(-0.905458935958868,0.42443387623072,0.));
#44390=DIRECTION('ref_axis',(-0.42443387623072,-0.905458935958868,0.));
#44391=DIRECTION('center_axis',(0.905458935958868,0.42443387623072,0.));
#44392=DIRECTION('ref_axis',(-0.42443387623072,0.905458935958868,0.));
#44393=DIRECTION('center_axis',(0.,1.,0.));
#44394=DIRECTION('ref_axis',(0.,0.,1.));
#44395=DIRECTION('center_axis',(0.,0.,1.));
#44396=DIRECTION('ref_axis',(1.,0.,0.));
#44397=DIRECTION('center_axis',(0.,0.,1.));
#44398=DIRECTION('ref_axis',(1.,0.,0.));
#44399=DIRECTION('center_axis',(0.,0.,1.));
#44400=DIRECTION('ref_axis',(1.,0.,0.));
#44401=DIRECTION('center_axis',(0.,0.,1.));
#44402=DIRECTION('ref_axis',(1.,0.,0.));
#44403=DIRECTION('center_axis',(0.,0.,-1.));
#44404=DIRECTION('ref_axis',(1.,0.,0.));
#44405=DIRECTION('center_axis',(0.,0.,-1.));
#44406=DIRECTION('ref_axis',(1.,8.67361737988403E-16,0.));
#44407=DIRECTION('center_axis',(0.,0.,1.));
#44408=DIRECTION('ref_axis',(1.,0.,0.));
#44409=DIRECTION('center_axis',(0.,0.,1.));
#44410=DIRECTION('ref_axis',(1.,0.,0.));
#44411=DIRECTION('',(0.,0.,1.));
#44412=DIRECTION('center_axis',(0.,0.,-1.));
#44413=DIRECTION('ref_axis',(1.,8.67361737988403E-16,0.));
#44414=DIRECTION('center_axis',(0.,0.,1.));
#44415=DIRECTION('ref_axis',(1.,0.,0.));
#44416=DIRECTION('center_axis',(0.,0.,-1.));
#44417=DIRECTION('ref_axis',(1.,0.,0.));
#44418=DIRECTION('',(0.,0.,-1.));
#44419=DIRECTION('center_axis',(0.,0.,1.));
#44420=DIRECTION('ref_axis',(1.,0.,0.));
#44421=DIRECTION('center_axis',(0.,0.,-1.));
#44422=DIRECTION('ref_axis',(-1.,0.,0.));
#44423=DIRECTION('center_axis',(0.,0.,-1.));
#44424=DIRECTION('ref_axis',(1.,-7.2280144832367E-16,0.));
#44425=DIRECTION('',(-0.42443387623072,-0.905458935958868,0.));
#44426=DIRECTION('center_axis',(0.,0.,1.));
#44427=DIRECTION('ref_axis',(1.,0.,0.));
#44428=DIRECTION('',(-1.,0.,0.));
#44429=DIRECTION('center_axis',(0.,0.,1.));
#44430=DIRECTION('ref_axis',(1.,0.,0.));
#44431=DIRECTION('',(-0.42443387623072,0.905458935958868,0.));
#44432=DIRECTION('center_axis',(0.,0.,-1.));
#44433=DIRECTION('ref_axis',(1.,-7.2280144832367E-16,0.));
#44434=DIRECTION('',(-0.424433876230721,0.905458935958868,0.));
#44435=DIRECTION('center_axis',(0.,0.,1.));
#44436=DIRECTION('ref_axis',(1.,0.,0.));
#44437=DIRECTION('',(-1.,0.,0.));
#44438=DIRECTION('center_axis',(0.,0.,1.));
#44439=DIRECTION('ref_axis',(1.,0.,0.));
#44440=DIRECTION('',(-0.424433876230721,-0.905458935958868,0.));
#44441=DIRECTION('center_axis',(0.,0.,-1.));
#44442=DIRECTION('ref_axis',(-0.42443387623072,-0.905458935958868,0.));
#44443=DIRECTION('center_axis',(0.,0.,1.));
#44444=DIRECTION('ref_axis',(1.,0.,0.));
#44445=DIRECTION('',(-0.42443387623072,0.905458935958868,0.));
#44446=DIRECTION('center_axis',(0.,0.,-1.));
#44447=DIRECTION('ref_axis',(1.,0.,0.));
#44448=DIRECTION('',(-1.,0.,0.));
#44449=DIRECTION('center_axis',(0.,0.,-1.));
#44450=DIRECTION('ref_axis',(1.,-1.73472347597681E-15,0.));
#44451=DIRECTION('',(-0.42443387623072,-0.905458935958868,0.));
#44452=DIRECTION('center_axis',(0.,0.,1.));
#44453=DIRECTION('ref_axis',(1.,0.,0.));
#44454=DIRECTION('',(-0.424433876230721,-0.905458935958868,0.));
#44455=DIRECTION('center_axis',(0.,0.,-1.));
#44456=DIRECTION('ref_axis',(1.,0.,0.));
#44457=DIRECTION('',(-1.,0.,0.));
#44458=DIRECTION('center_axis',(0.,0.,-1.));
#44459=DIRECTION('ref_axis',(1.,1.69701209606427E-15,0.));
#44460=DIRECTION('',(-0.424433876230721,0.905458935958868,0.));
#44461=DIRECTION('center_axis',(0.,0.,1.));
#44462=DIRECTION('ref_axis',(1.,0.,0.));
#44463=DIRECTION('',(0.,0.,1.));
#44464=DIRECTION('',(0.,0.,-1.));
#44465=DIRECTION('center_axis',(0.,0.,1.));
#44466=DIRECTION('ref_axis',(1.,0.,0.));
#44467=DIRECTION('',(0.,0.,1.));
#44468=DIRECTION('',(0.,0.,-1.));
#44469=DIRECTION('center_axis',(-0.905458935958868,0.42443387623072,0.));
#44470=DIRECTION('ref_axis',(-0.42443387623072,-0.905458935958868,0.));
#44471=DIRECTION('center_axis',(0.905458935958868,0.42443387623072,0.));
#44472=DIRECTION('ref_axis',(-0.42443387623072,0.905458935958868,0.));
#44473=DIRECTION('center_axis',(0.,1.,0.));
#44474=DIRECTION('ref_axis',(0.,0.,1.));
#44475=DIRECTION('center_axis',(0.,0.,1.));
#44476=DIRECTION('ref_axis',(1.,0.,0.));
#44477=DIRECTION('',(0.,0.,-1.));
#44478=DIRECTION('',(0.,0.,1.));
#44479=DIRECTION('center_axis',(0.,0.,1.));
#44480=DIRECTION('ref_axis',(1.,0.,0.));
#44481=DIRECTION('',(0.,0.,-1.));
#44482=DIRECTION('',(0.,0.,1.));
#44483=DIRECTION('center_axis',(0.,0.,1.));
#44484=DIRECTION('ref_axis',(1.,0.,0.));
#44485=DIRECTION('',(0.,0.,-1.));
#44486=DIRECTION('center_axis',(0.,0.,1.));
#44487=DIRECTION('ref_axis',(1.,0.,0.));
#44488=DIRECTION('',(0.,0.,1.));
#44489=DIRECTION('center_axis',(-0.905458935958868,0.42443387623072,0.));
#44490=DIRECTION('ref_axis',(-0.42443387623072,-0.905458935958868,0.));
#44491=DIRECTION('center_axis',(0.905458935958868,0.42443387623072,0.));
#44492=DIRECTION('ref_axis',(-0.42443387623072,0.905458935958868,0.));
#44493=DIRECTION('center_axis',(0.,1.,0.));
#44494=DIRECTION('ref_axis',(0.,0.,1.));
#44495=DIRECTION('center_axis',(0.,0.,1.));
#44496=DIRECTION('ref_axis',(1.,0.,0.));
#44497=DIRECTION('center_axis',(0.,0.,1.));
#44498=DIRECTION('ref_axis',(1.,0.,0.));
#44499=DIRECTION('center_axis',(0.,0.,1.));
#44500=DIRECTION('ref_axis',(1.,0.,0.));
#44501=DIRECTION('center_axis',(0.,0.,1.));
#44502=DIRECTION('ref_axis',(1.,0.,0.));
#44503=DIRECTION('center_axis',(0.,0.,-1.));
#44504=DIRECTION('ref_axis',(1.,0.,0.));
#44505=DIRECTION('center_axis',(0.,0.,-1.));
#44506=DIRECTION('ref_axis',(1.,8.67361737988403E-16,0.));
#44507=DIRECTION('center_axis',(0.,0.,1.));
#44508=DIRECTION('ref_axis',(1.,0.,0.));
#44509=DIRECTION('center_axis',(0.,0.,1.));
#44510=DIRECTION('ref_axis',(1.,0.,0.));
#44511=DIRECTION('',(0.,0.,1.));
#44512=DIRECTION('center_axis',(0.,0.,-1.));
#44513=DIRECTION('ref_axis',(1.,8.67361737988403E-16,0.));
#44514=DIRECTION('center_axis',(0.,0.,1.));
#44515=DIRECTION('ref_axis',(1.,0.,0.));
#44516=DIRECTION('center_axis',(0.,0.,-1.));
#44517=DIRECTION('ref_axis',(1.,0.,0.));
#44518=DIRECTION('',(0.,0.,-1.));
#44519=DIRECTION('center_axis',(0.,0.,1.));
#44520=DIRECTION('ref_axis',(1.,0.,0.));
#44521=DIRECTION('center_axis',(0.,0.,-1.));
#44522=DIRECTION('ref_axis',(-1.,0.,0.));
#44523=DIRECTION('center_axis',(0.,0.,-1.));
#44524=DIRECTION('ref_axis',(1.,-7.2280144832367E-16,0.));
#44525=DIRECTION('',(-0.42443387623072,-0.905458935958868,0.));
#44526=DIRECTION('center_axis',(0.,0.,1.));
#44527=DIRECTION('ref_axis',(1.,0.,0.));
#44528=DIRECTION('',(-1.,0.,0.));
#44529=DIRECTION('center_axis',(0.,0.,1.));
#44530=DIRECTION('ref_axis',(1.,0.,0.));
#44531=DIRECTION('',(-0.42443387623072,0.905458935958868,0.));
#44532=DIRECTION('center_axis',(0.,0.,-1.));
#44533=DIRECTION('ref_axis',(1.,-7.2280144832367E-16,0.));
#44534=DIRECTION('',(-0.42443387623072,0.905458935958868,0.));
#44535=DIRECTION('center_axis',(0.,0.,1.));
#44536=DIRECTION('ref_axis',(1.,0.,0.));
#44537=DIRECTION('',(-1.,0.,0.));
#44538=DIRECTION('center_axis',(0.,0.,1.));
#44539=DIRECTION('ref_axis',(1.,0.,0.));
#44540=DIRECTION('',(-0.42443387623072,-0.905458935958868,0.));
#44541=DIRECTION('center_axis',(0.,0.,-1.));
#44542=DIRECTION('ref_axis',(-0.42443387623072,-0.905458935958868,0.));
#44543=DIRECTION('center_axis',(0.,0.,1.));
#44544=DIRECTION('ref_axis',(1.,0.,0.));
#44545=DIRECTION('',(-0.42443387623072,0.905458935958868,0.));
#44546=DIRECTION('center_axis',(0.,0.,-1.));
#44547=DIRECTION('ref_axis',(1.,0.,0.));
#44548=DIRECTION('',(-1.,0.,0.));
#44549=DIRECTION('center_axis',(0.,0.,-1.));
#44550=DIRECTION('ref_axis',(1.,-1.73472347597681E-15,0.));
#44551=DIRECTION('',(-0.42443387623072,-0.905458935958868,0.));
#44552=DIRECTION('center_axis',(0.,0.,1.));
#44553=DIRECTION('ref_axis',(1.,0.,0.));
#44554=DIRECTION('',(-0.42443387623072,-0.905458935958868,0.));
#44555=DIRECTION('center_axis',(0.,0.,-1.));
#44556=DIRECTION('ref_axis',(1.,0.,0.));
#44557=DIRECTION('',(-1.,0.,0.));
#44558=DIRECTION('center_axis',(0.,0.,-1.));
#44559=DIRECTION('ref_axis',(1.,1.69701209606427E-15,0.));
#44560=DIRECTION('',(-0.42443387623072,0.905458935958868,0.));
#44561=DIRECTION('center_axis',(0.,0.,1.));
#44562=DIRECTION('ref_axis',(1.,0.,0.));
#44563=DIRECTION('',(0.,0.,1.));
#44564=DIRECTION('',(0.,0.,-1.));
#44565=DIRECTION('center_axis',(0.,0.,1.));
#44566=DIRECTION('ref_axis',(1.,0.,0.));
#44567=DIRECTION('',(0.,0.,1.));
#44568=DIRECTION('',(0.,0.,-1.));
#44569=DIRECTION('center_axis',(-0.905458935958868,0.42443387623072,0.));
#44570=DIRECTION('ref_axis',(-0.42443387623072,-0.905458935958868,0.));
#44571=DIRECTION('center_axis',(0.905458935958868,0.42443387623072,0.));
#44572=DIRECTION('ref_axis',(-0.42443387623072,0.905458935958868,0.));
#44573=DIRECTION('center_axis',(0.,1.,0.));
#44574=DIRECTION('ref_axis',(0.,0.,1.));
#44575=DIRECTION('center_axis',(0.,0.,1.));
#44576=DIRECTION('ref_axis',(1.,0.,0.));
#44577=DIRECTION('',(0.,0.,-1.));
#44578=DIRECTION('',(0.,0.,1.));
#44579=DIRECTION('center_axis',(0.,0.,1.));
#44580=DIRECTION('ref_axis',(1.,0.,0.));
#44581=DIRECTION('',(0.,0.,-1.));
#44582=DIRECTION('',(0.,0.,1.));
#44583=DIRECTION('center_axis',(0.,0.,1.));
#44584=DIRECTION('ref_axis',(1.,0.,0.));
#44585=DIRECTION('',(0.,0.,-1.));
#44586=DIRECTION('center_axis',(0.,0.,1.));
#44587=DIRECTION('ref_axis',(1.,0.,0.));
#44588=DIRECTION('',(0.,0.,1.));
#44589=DIRECTION('center_axis',(-0.905458935958868,0.42443387623072,0.));
#44590=DIRECTION('ref_axis',(-0.42443387623072,-0.905458935958868,0.));
#44591=DIRECTION('center_axis',(0.905458935958868,0.42443387623072,0.));
#44592=DIRECTION('ref_axis',(-0.42443387623072,0.905458935958868,0.));
#44593=DIRECTION('center_axis',(0.,1.,0.));
#44594=DIRECTION('ref_axis',(0.,0.,1.));
#44595=DIRECTION('center_axis',(-1.,-4.38245930773088E-16,0.));
#44596=DIRECTION('ref_axis',(0.,0.,1.));
#44597=DIRECTION('center_axis',(1.,4.38245930773088E-16,0.));
#44598=DIRECTION('ref_axis',(4.38245930773088E-16,-1.,0.));
#44599=DIRECTION('center_axis',(1.,4.38245930773088E-16,0.));
#44600=DIRECTION('ref_axis',(4.38245930773088E-16,-1.,0.));
#44601=DIRECTION('',(-3.46944695195361E-16,0.5,0.866025403784438));
#44602=DIRECTION('center_axis',(1.,4.38245930773088E-16,0.));
#44603=DIRECTION('ref_axis',(4.38245930773088E-16,-1.,2.31296463463574E-15));
#44604=DIRECTION('center_axis',(1.,4.38245930773088E-16,0.));
#44605=DIRECTION('ref_axis',(4.38245930773088E-16,-1.,2.31296463463574E-15));
#44606=DIRECTION('',(3.46944695195361E-16,-0.5,-0.866025403784438));
#44607=DIRECTION('center_axis',(1.,4.38245930773088E-16,0.));
#44608=DIRECTION('ref_axis',(4.38245930773088E-16,-1.,0.));
#44609=DIRECTION('',(-4.38245930773088E-16,1.,0.));
#44610=DIRECTION('center_axis',(1.,4.38245930773088E-16,0.));
#44611=DIRECTION('ref_axis',(4.38245930773088E-16,-1.,0.));
#44612=DIRECTION('center_axis',(1.,4.38245930773088E-16,0.));
#44613=DIRECTION('ref_axis',(4.38245930773088E-16,-1.,0.));
#44614=DIRECTION('',(4.38245930773088E-16,-1.,0.));
#44615=DIRECTION('center_axis',(1.,4.38245930773088E-16,0.));
#44616=DIRECTION('ref_axis',(4.38245930773088E-16,-1.,0.));
#44617=DIRECTION('',(-3.46944695195361E-16,0.499999999999999,-0.866025403784439));
#44618=DIRECTION('center_axis',(1.,4.38245930773088E-16,0.));
#44619=DIRECTION('ref_axis',(4.38245930773088E-16,-1.,0.));
#44620=DIRECTION('center_axis',(1.,4.38245930773088E-16,0.));
#44621=DIRECTION('ref_axis',(4.38245930773088E-16,-1.,0.));
#44622=DIRECTION('',(3.46944695195362E-16,-0.499999999999999,0.866025403784439));
#44623=DIRECTION('center_axis',(1.,4.38245930773088E-16,0.));
#44624=DIRECTION('ref_axis',(4.38245930773088E-16,-1.,4.62592926927148E-15));
#44625=DIRECTION('center_axis',(1.,4.38245930773088E-16,0.));
#44626=DIRECTION('ref_axis',(4.38245930773088E-16,-1.,-9.25185853854296E-15));
#44627=DIRECTION('',(0.,-0.5,-0.866025403784438));
#44628=DIRECTION('center_axis',(1.,4.38245930773088E-16,0.));
#44629=DIRECTION('ref_axis',(4.38245930773088E-16,-1.,0.));
#44630=DIRECTION('',(0.,0.5,0.866025403784438));
#44631=DIRECTION('center_axis',(1.,4.38245930773088E-16,0.));
#44632=DIRECTION('ref_axis',(4.38245930773088E-16,-1.,4.62592926927148E-15));
#44633=DIRECTION('center_axis',(1.,4.38245930773088E-16,0.));
#44634=DIRECTION('ref_axis',(4.38245930773088E-16,-1.,0.));
#44635=DIRECTION('',(4.38245930773088E-16,-1.,0.));
#44636=DIRECTION('',(-4.38245930773088E-16,1.,0.));
#44637=DIRECTION('center_axis',(1.,4.38245930773088E-16,0.));
#44638=DIRECTION('ref_axis',(4.38245930773088E-16,-1.,0.));
#44639=DIRECTION('center_axis',(1.,4.38245930773088E-16,0.));
#44640=DIRECTION('ref_axis',(4.38245930773088E-16,-1.,0.));
#44641=DIRECTION('',(0.,-0.5,0.866025403784439));
#44642=DIRECTION('center_axis',(1.,4.38245930773088E-16,0.));
#44643=DIRECTION('ref_axis',(4.38245930773088E-16,-1.,0.));
#44644=DIRECTION('center_axis',(1.,4.38245930773088E-16,0.));
#44645=DIRECTION('ref_axis',(4.38245930773088E-16,-1.,0.));
#44646=DIRECTION('center_axis',(1.,4.38245930773088E-16,0.));
#44647=DIRECTION('ref_axis',(4.38245930773088E-16,-1.,0.));
#44648=DIRECTION('center_axis',(1.,4.38245930773088E-16,0.));
#44649=DIRECTION('ref_axis',(4.38245930773088E-16,-1.,2.89120579329468E-15));
#44650=DIRECTION('center_axis',(1.,4.38245930773088E-16,0.));
#44651=DIRECTION('ref_axis',(4.38245930773088E-16,-1.,1.73472347597681E-15));
#44652=DIRECTION('center_axis',(1.,4.38245930773088E-16,0.));
#44653=DIRECTION('ref_axis',(4.38245930773088E-16,-1.,0.));
#44654=DIRECTION('center_axis',(1.,4.38245930773088E-16,0.));
#44655=DIRECTION('ref_axis',(4.38245930773088E-16,-1.,0.));
#44656=DIRECTION('center_axis',(1.,4.38245930773088E-16,0.));
#44657=DIRECTION('ref_axis',(4.38245930773088E-16,-1.,0.));
#44658=DIRECTION('center_axis',(1.,4.38245930773088E-16,0.));
#44659=DIRECTION('ref_axis',(4.38245930773088E-16,-1.,0.));
#44660=DIRECTION('center_axis',(1.,4.38245930773088E-16,0.));
#44661=DIRECTION('ref_axis',(4.38245930773088E-16,-1.,4.62592926927148E-15));
#44662=DIRECTION('center_axis',(1.,4.38245930773088E-16,0.));
#44663=DIRECTION('ref_axis',(4.38245930773088E-16,-1.,-4.62592926927148E-15));
#44664=DIRECTION('center_axis',(1.,4.38245930773088E-16,0.));
#44665=DIRECTION('ref_axis',(4.38245930773088E-16,-1.,0.));
#44666=DIRECTION('center_axis',(1.,4.38245930773088E-16,0.));
#44667=DIRECTION('ref_axis',(4.38245930773088E-16,-1.,-4.62592926927148E-15));
#44668=DIRECTION('center_axis',(1.,4.38245930773088E-16,0.));
#44669=DIRECTION('ref_axis',(4.38245930773088E-16,-1.,0.));
#44670=DIRECTION('center_axis',(1.,4.38245930773088E-16,0.));
#44671=DIRECTION('ref_axis',(4.38245930773088E-16,-1.,9.25185853854296E-15));
#44672=DIRECTION('center_axis',(1.,4.38245930773088E-16,0.));
#44673=DIRECTION('ref_axis',(4.38245930773088E-16,-1.,0.));
#44674=DIRECTION('center_axis',(1.,4.38245930773088E-16,0.));
#44675=DIRECTION('ref_axis',(4.38245930773088E-16,-1.,0.));
#44676=DIRECTION('center_axis',(1.,4.38245930773088E-16,0.));
#44677=DIRECTION('ref_axis',(4.38245930773088E-16,-1.,1.15648231731787E-15));
#44678=DIRECTION('center_axis',(1.,4.38245930773088E-16,0.));
#44679=DIRECTION('ref_axis',(4.38245930773088E-16,-1.,1.15648231731787E-15));
#44680=DIRECTION('center_axis',(1.,4.38245930773088E-16,0.));
#44681=DIRECTION('ref_axis',(4.38245930773088E-16,-1.,1.80700362080917E-15));
#44682=DIRECTION('center_axis',(1.,4.38245930773088E-16,0.));
#44683=DIRECTION('ref_axis',(4.38245930773088E-16,-1.,-8.67361737988403E-16));
#44684=DIRECTION('center_axis',(1.,4.38245930773088E-16,0.));
#44685=DIRECTION('ref_axis',(4.38245930773088E-16,-1.,6.36065274524829E-15));
#44686=DIRECTION('center_axis',(1.,4.38245930773088E-16,0.));
#44687=DIRECTION('ref_axis',(4.38245930773088E-16,-1.,8.67361737988403E-16));
#44688=DIRECTION('center_axis',(1.,4.38245930773088E-16,0.));
#44689=DIRECTION('ref_axis',(4.38245930773088E-16,-1.,0.));
#44690=DIRECTION('center_axis',(1.,4.38245930773088E-16,0.));
#44691=DIRECTION('ref_axis',(4.38245930773088E-16,-1.,0.));
#44692=DIRECTION('center_axis',(1.,4.38245930773088E-16,0.));
#44693=DIRECTION('ref_axis',(4.38245930773088E-16,-1.,0.));
#44694=DIRECTION('center_axis',(1.,4.38245930773088E-16,0.));
#44695=DIRECTION('ref_axis',(4.38245930773088E-16,-1.,0.));
#44696=DIRECTION('center_axis',(1.,4.38245930773088E-16,0.));
#44697=DIRECTION('ref_axis',(4.38245930773088E-16,-1.,4.62592926927148E-15));
#44698=DIRECTION('center_axis',(1.,4.38245930773088E-16,0.));
#44699=DIRECTION('ref_axis',(4.38245930773088E-16,-1.,0.));
#44700=DIRECTION('center_axis',(1.,4.38245930773088E-16,0.));
#44701=DIRECTION('ref_axis',(4.38245930773088E-16,-1.,4.62592926927148E-15));
#44702=DIRECTION('center_axis',(1.,4.38245930773088E-16,0.));
#44703=DIRECTION('ref_axis',(4.38245930773088E-16,-1.,9.25185853854296E-15));
#44704=DIRECTION('center_axis',(1.,4.38245930773088E-16,0.));
#44705=DIRECTION('ref_axis',(4.38245930773088E-16,-1.,-4.62592926927148E-15));
#44706=DIRECTION('center_axis',(1.,4.38245930773088E-16,0.));
#44707=DIRECTION('ref_axis',(4.38245930773088E-16,-1.,4.62592926927148E-15));
#44708=DIRECTION('center_axis',(1.,4.38245930773088E-16,0.));
#44709=DIRECTION('ref_axis',(4.38245930773088E-16,-1.,0.));
#44710=DIRECTION('center_axis',(1.,4.38245930773088E-16,0.));
#44711=DIRECTION('ref_axis',(4.38245930773088E-16,-1.,0.));
#44712=DIRECTION('center_axis',(1.,4.38245930773088E-16,0.));
#44713=DIRECTION('ref_axis',(4.38245930773088E-16,-1.,-1.73472347597681E-15));
#44714=DIRECTION('center_axis',(1.,4.38245930773088E-16,0.));
#44715=DIRECTION('ref_axis',(4.38245930773088E-16,-1.,-1.73472347597681E-15));
#44716=DIRECTION('',(1.,4.38245930773088E-16,0.));
#44717=DIRECTION('',(-1.,-4.38245930773088E-16,0.));
#44718=DIRECTION('center_axis',(-3.79532109154651E-16,0.866025403784439,
0.499999999999999));
#44719=DIRECTION('ref_axis',(-7.94699513894569E-33,-0.499999999999999,0.866025403784439));
#44720=DIRECTION('',(-1.,-4.38245930773088E-16,0.));
#44721=DIRECTION('center_axis',(3.79532109154651E-16,-0.866025403784439,
-0.499999999999999));
#44722=DIRECTION('ref_axis',(1.5326347767966E-32,0.499999999999999,-0.866025403784439));
#44723=DIRECTION('',(1.,4.38245930773088E-16,0.));
#44724=DIRECTION('',(-1.,-4.38245930773088E-16,0.));
#44725=DIRECTION('center_axis',(-3.79532109154651E-16,0.866025403784438,
-0.5));
#44726=DIRECTION('ref_axis',(1.94620289117031E-33,0.5,0.866025403784438));
#44727=DIRECTION('',(1.,4.38245930773088E-16,8.64002241377108E-33));
#44728=DIRECTION('center_axis',(3.79532109154651E-16,-0.866025403784438,
0.5));
#44729=DIRECTION('ref_axis',(-1.94620289117031E-33,-0.5,-0.866025403784438));
#44730=DIRECTION('',(1.,4.38245930773088E-16,8.64002241377108E-33));
#44731=DIRECTION('',(-1.,-4.38245930773088E-16,-8.64002241377108E-33));
#44732=DIRECTION('center_axis',(0.,0.,-1.));
#44733=DIRECTION('ref_axis',(-1.,0.,0.));
#44734=DIRECTION('',(1.,4.38245930773088E-16,0.));
#44735=DIRECTION('center_axis',(0.,0.,1.));
#44736=DIRECTION('ref_axis',(1.,0.,0.));
#44737=DIRECTION('',(-1.,-4.38245930773088E-16,0.));
#44738=DIRECTION('center_axis',(3.79532109154651E-16,-0.866025403784439,
-0.5));
#44739=DIRECTION('ref_axis',(-8.35245407460559E-33,0.5,-0.866025403784439));
#44740=DIRECTION('',(-1.,-4.38245930773088E-16,0.));
#44741=DIRECTION('',(1.,4.38245930773088E-16,0.));
#44742=DIRECTION('center_axis',(3.79532109154651E-16,-0.866025403784438,
0.5));
#44743=DIRECTION('ref_axis',(2.27057003969863E-32,-0.5,-0.866025403784438));
#44744=DIRECTION('',(-1.,-4.38245930773088E-16,0.));
#44745=DIRECTION('',(1.,4.38245930773088E-16,0.));
#44746=DIRECTION('center_axis',(-3.79532109154651E-16,0.866025403784439,
-0.5));
#44747=DIRECTION('ref_axis',(-1.08662994757006E-32,0.5,0.866025403784439));
#44748=DIRECTION('',(1.,4.38245930773088E-16,0.));
#44749=DIRECTION('center_axis',(0.,0.,1.));
#44750=DIRECTION('ref_axis',(1.,0.,0.));
#44751=DIRECTION('',(-1.,-4.38245930773088E-16,0.));
#44752=DIRECTION('',(1.,4.38245930773088E-16,0.));
#44753=DIRECTION('center_axis',(0.,0.,-1.));
#44754=DIRECTION('ref_axis',(-1.,0.,0.));
#44755=DIRECTION('',(-1.,-4.38245930773088E-16,0.));
#44756=DIRECTION('',(1.,4.38245930773088E-16,0.));
#44757=DIRECTION('',(-1.,-4.38245930773088E-16,0.));
#44758=DIRECTION('',(1.,4.38245930773088E-16,0.));
#44759=DIRECTION('',(1.,4.38245930773088E-16,0.));
#44760=DIRECTION('',(-1.,-4.38245930773088E-16,0.));
#44761=DIRECTION('',(1.,4.38245930773088E-16,0.));
#44762=DIRECTION('',(-1.,-4.38245930773088E-16,0.));
#44763=DIRECTION('',(-1.,-4.38245930773088E-16,0.));
#44764=DIRECTION('',(1.,4.38245930773088E-16,0.));
#44765=DIRECTION('',(1.,4.38245930773088E-16,0.));
#44766=DIRECTION('',(-1.,-4.38245930773088E-16,0.));
#44767=DIRECTION('',(-1.,-4.38245930773088E-16,0.));
#44768=DIRECTION('',(1.,4.38245930773088E-16,0.));
#44769=DIRECTION('',(-1.,-4.38245930773088E-16,0.));
#44770=DIRECTION('',(1.,4.38245930773088E-16,0.));
#44771=DIRECTION('',(-1.,-4.38245930773088E-16,0.));
#44772=DIRECTION('',(-1.,-4.38245930773088E-16,0.));
#44773=DIRECTION('',(-1.,-4.38245930773088E-16,0.));
#44774=DIRECTION('',(1.,4.38245930773088E-16,0.));
#44775=DIRECTION('',(1.,4.38245930773088E-16,0.));
#44776=DIRECTION('',(-1.,-4.38245930773088E-16,0.));
#44777=DIRECTION('',(1.,4.38245930773088E-16,0.));
#44778=DIRECTION('',(-1.,-4.38245930773088E-16,0.));
#44779=DIRECTION('',(-1.,-4.38245930773088E-16,0.));
#44780=DIRECTION('',(1.,4.38245930773088E-16,0.));
#44781=DIRECTION('',(1.,4.38245930773088E-16,0.));
#44782=DIRECTION('',(-1.,-4.38245930773088E-16,0.));
#44783=DIRECTION('',(-1.,-4.38245930773088E-16,0.));
#44784=DIRECTION('',(1.,4.38245930773088E-16,0.));
#44785=DIRECTION('',(-1.,-4.38245930773088E-16,0.));
#44786=DIRECTION('',(1.,4.38245930773088E-16,0.));
#44787=DIRECTION('',(-1.,-4.38245930773088E-16,0.));
#44788=DIRECTION('',(-1.,-4.38245930773088E-16,0.));
#44789=DIRECTION('',(1.,4.38245930773088E-16,0.));
#44790=DIRECTION('',(-1.,-4.38245930773088E-16,0.));
#44791=DIRECTION('',(-1.,-4.38245930773088E-16,0.));
#44792=DIRECTION('',(1.,4.38245930773088E-16,0.));
#44793=DIRECTION('',(-1.,-4.38245930773088E-16,0.));
#44794=DIRECTION('',(1.,4.38245930773088E-16,0.));
#44795=DIRECTION('',(-1.,-4.38245930773088E-16,0.));
#44796=DIRECTION('',(1.,4.38245930773088E-16,0.));
#44797=DIRECTION('',(-1.,-4.38245930773088E-16,0.));
#44798=DIRECTION('center_axis',(-1.,-4.38245930773088E-16,0.));
#44799=DIRECTION('ref_axis',(4.38245930773088E-16,-1.,0.));
#44800=DIRECTION('center_axis',(-1.,-4.38245930773088E-16,0.));
#44801=DIRECTION('ref_axis',(4.38245930773088E-16,-1.,0.));
#44802=DIRECTION('center_axis',(-1.,-4.38245930773088E-16,0.));
#44803=DIRECTION('ref_axis',(-3.3768778812357E-16,0.770544035692177,0.637386765676236));
#44804=DIRECTION('center_axis',(-1.,-4.38245930773088E-16,0.));
#44805=DIRECTION('ref_axis',(4.38245930773088E-16,-1.,0.));
#44806=DIRECTION('center_axis',(-1.,-4.38245930773088E-16,0.));
#44807=DIRECTION('ref_axis',(-3.26063191989391E-16,0.744018755437613,0.668158732306228));
#44808=DIRECTION('center_axis',(-1.,-4.38245930773088E-16,0.));
#44809=DIRECTION('ref_axis',(4.38245930773088E-16,-1.,0.));
#44810=DIRECTION('center_axis',(-1.,-4.38245930773088E-16,0.));
#44811=DIRECTION('ref_axis',(-4.18556581656484E-16,0.955072374358683,-0.296372670360928));
#44812=DIRECTION('center_axis',(-1.,-4.38245930773088E-16,0.));
#44813=DIRECTION('ref_axis',(4.38245930773088E-16,-1.,0.));
#44814=DIRECTION('center_axis',(-1.,-4.38245930773088E-16,0.));
#44815=DIRECTION('ref_axis',(4.38245930773088E-16,-1.,0.));
#44816=DIRECTION('center_axis',(-1.,-4.38245930773088E-16,0.));
#44817=DIRECTION('ref_axis',(-4.18556584246465E-16,0.955072380268563,0.296372651316112));
#44818=DIRECTION('center_axis',(-1.,-4.38245930773088E-16,0.));
#44819=DIRECTION('ref_axis',(4.38245930773088E-16,-1.,0.));
#44820=DIRECTION('center_axis',(-1.,-4.38245930773088E-16,0.));
#44821=DIRECTION('ref_axis',(-3.21714447165222E-16,0.734095685948987,-0.679046039581328));
#44822=DIRECTION('center_axis',(-1.,-4.38245930773088E-16,0.));
#44823=DIRECTION('ref_axis',(-3.21714455957828E-16,0.734095706012164,0.679046017891647));
#44824=DIRECTION('center_axis',(-1.,-4.38245930773088E-16,0.));
#44825=DIRECTION('ref_axis',(4.38245930773088E-16,-1.,0.));
#44826=DIRECTION('center_axis',(-1.,-4.38245930773088E-16,0.));
#44827=DIRECTION('ref_axis',(4.38245930773088E-16,-1.,0.));
#44828=DIRECTION('center_axis',(-1.,-4.38245930773088E-16,0.));
#44829=DIRECTION('ref_axis',(4.38245930773088E-16,-1.,0.));
#44830=DIRECTION('center_axis',(-1.,-4.38245930773088E-16,0.));
#44831=DIRECTION('ref_axis',(-4.27911362366366E-16,0.976418335731055,0.215887085413176));
#44832=DIRECTION('center_axis',(-1.,-4.38245930773088E-16,0.));
#44833=DIRECTION('ref_axis',(4.38245930773088E-16,-1.,0.));
#44834=DIRECTION('center_axis',(-1.,-4.38245930773088E-16,0.));
#44835=DIRECTION('ref_axis',(4.38245930773088E-16,-1.,0.));
#44836=DIRECTION('center_axis',(-1.,-4.38245930773088E-16,0.));
#44837=DIRECTION('ref_axis',(-4.27911362366367E-16,0.976418335731058,-0.215887085413164));
#44838=DIRECTION('center_axis',(-1.,-4.38245930773088E-16,0.));
#44839=DIRECTION('ref_axis',(4.38245930773088E-16,-1.,0.));
#44840=DIRECTION('center_axis',(-1.,-4.38245930773088E-16,0.));
#44841=DIRECTION('ref_axis',(4.38245930773088E-16,-1.,0.));
#44842=DIRECTION('center_axis',(-1.,-4.38245930773088E-16,0.));
#44843=DIRECTION('ref_axis',(4.38245930773088E-16,-1.,0.));
#44844=DIRECTION('center_axis',(-1.,-4.38245930773088E-16,0.));
#44845=DIRECTION('ref_axis',(-4.16621911423142E-16,0.950657797753421,-0.310241440769309));
#44846=DIRECTION('center_axis',(-1.,-4.38245930773088E-16,0.));
#44847=DIRECTION('ref_axis',(4.38245930773088E-16,-1.,0.));
#44848=DIRECTION('center_axis',(-1.,-4.38245930773088E-16,0.));
#44849=DIRECTION('ref_axis',(4.38245930773088E-16,-1.,0.));
#44850=DIRECTION('center_axis',(-1.,-4.38245930773088E-16,0.));
#44851=DIRECTION('ref_axis',(-4.16621911423141E-16,0.950657797753419,0.310241440769313));
#44852=DIRECTION('center_axis',(-1.,-4.38245930773088E-16,0.));
#44853=DIRECTION('ref_axis',(4.38245930773088E-16,-1.,0.));
#44854=DIRECTION('center_axis',(-1.,-4.38245930773088E-16,0.));
#44855=DIRECTION('ref_axis',(-3.26063191989868E-16,0.7440187554387,-0.668158732305017));
#44856=DIRECTION('center_axis',(-1.,-4.38245930773088E-16,0.));
#44857=DIRECTION('ref_axis',(4.38245930773088E-16,-1.,0.));
#44858=DIRECTION('center_axis',(-1.,-4.38245930773088E-16,0.));
#44859=DIRECTION('ref_axis',(4.38245930773088E-16,-1.,0.));
#44860=DIRECTION('center_axis',(-1.,-4.38245930773088E-16,0.));
#44861=DIRECTION('ref_axis',(4.38245930773088E-16,-1.,0.));
#44862=DIRECTION('center_axis',(-1.,-4.38245930773088E-16,0.));
#44863=DIRECTION('ref_axis',(-4.30076690142246E-16,0.981359232209114,0.192182354439575));
#44864=DIRECTION('center_axis',(-1.,-4.38245930773088E-16,0.));
#44865=DIRECTION('ref_axis',(4.38245930773088E-16,-1.,0.));
#44866=DIRECTION('center_axis',(-1.,-4.38245930773088E-16,0.));
#44867=DIRECTION('ref_axis',(4.38245930773088E-16,-1.,0.));
#44868=DIRECTION('center_axis',(-1.,-4.38245930773088E-16,0.));
#44869=DIRECTION('ref_axis',(-4.30076690142246E-16,0.981359232209114,-0.192182354439576));
#44870=DIRECTION('center_axis',(-1.,-4.38245930773088E-16,0.));
#44871=DIRECTION('ref_axis',(4.38245930773088E-16,-1.,0.));
#44872=DIRECTION('center_axis',(-1.,-4.38245930773088E-16,0.));
#44873=DIRECTION('ref_axis',(4.38245930773088E-16,-1.,0.));
#44874=DIRECTION('center_axis',(-1.,-4.38245930773088E-16,0.));
#44875=DIRECTION('ref_axis',(4.38245930773088E-16,-1.,0.));
#44876=DIRECTION('center_axis',(-1.,-4.38245930773088E-16,0.));
#44877=DIRECTION('ref_axis',(-4.10746190391092E-16,0.937250437594515,-0.348656876067132));
#44878=DIRECTION('center_axis',(-1.,-4.38245930773088E-16,0.));
#44879=DIRECTION('ref_axis',(4.38245930773088E-16,-1.,0.));
#44880=DIRECTION('center_axis',(-1.,-4.38245930773088E-16,0.));
#44881=DIRECTION('ref_axis',(4.38245930773088E-16,-1.,0.));
#44882=DIRECTION('center_axis',(-1.,-4.38245930773088E-16,0.));
#44883=DIRECTION('ref_axis',(-4.10746190391092E-16,0.937250437594514,0.348656876067132));
#44884=DIRECTION('center_axis',(-1.,-4.38245930773088E-16,0.));
#44885=DIRECTION('ref_axis',(4.38245930773088E-16,-1.,0.));
#44886=DIRECTION('center_axis',(-1.,-4.38245930773088E-16,0.));
#44887=DIRECTION('ref_axis',(-3.3768778811311E-16,0.770544035668309,-0.637386765705091));
#44888=DIRECTION('center_axis',(-1.,-4.38245930773088E-16,0.));
#44889=DIRECTION('ref_axis',(4.38245930773088E-16,-1.,0.));
#44890=DIRECTION('center_axis',(-1.,-4.38245930773088E-16,0.));
#44891=DIRECTION('ref_axis',(4.38245930773088E-16,-1.,0.));
#44892=DIRECTION('center_axis',(-1.,-4.38245930773088E-16,0.));
#44893=DIRECTION('ref_axis',(4.38245930773088E-16,-1.,0.));
#44894=DIRECTION('center_axis',(-1.,-4.38245930773088E-16,0.));
#44895=DIRECTION('ref_axis',(-4.36006704245932E-16,0.994890479591663,0.100960059517961));
#44896=DIRECTION('center_axis',(-1.,-4.38245930773088E-16,0.));
#44897=DIRECTION('ref_axis',(4.38245930773088E-16,-1.,0.));
#44898=DIRECTION('center_axis',(-1.,-4.38245930773088E-16,0.));
#44899=DIRECTION('ref_axis',(4.38245930773088E-16,-1.,0.));
#44900=DIRECTION('center_axis',(-1.,-4.38245930773088E-16,0.));
#44901=DIRECTION('ref_axis',(-4.36006704245932E-16,0.994890479591662,-0.100960059517976));
#44902=DIRECTION('center_axis',(-1.,-4.38245930773088E-16,0.));
#44903=DIRECTION('ref_axis',(4.38245930773088E-16,-1.,0.));
#44904=DIRECTION('center_axis',(-1.,-4.38245930773088E-16,0.));
#44905=DIRECTION('ref_axis',(4.38245930773088E-16,-1.,0.));
#44906=DIRECTION('center_axis',(-1.,-4.38245930773088E-16,0.));
#44907=DIRECTION('ref_axis',(4.38245930773088E-16,-1.,0.));
#44908=DIRECTION('',(-1.,-4.38245930773088E-16,0.));
#44909=DIRECTION('',(-1.,-4.38245930773088E-16,0.));
#44910=DIRECTION('center_axis',(0.,0.,1.));
#44911=DIRECTION('ref_axis',(1.,0.,0.));
#44912=DIRECTION('',(-1.,-4.38245930773088E-16,0.));
#44913=DIRECTION('center_axis',(-1.,-4.38245930773088E-16,0.));
#44914=DIRECTION('ref_axis',(4.38245930773088E-16,-1.,0.));
#44915=DIRECTION('',(-1.,-4.38245930773088E-16,0.));
#44916=DIRECTION('center_axis',(3.09886669477059E-16,-0.707106781186543,
0.707106781186552));
#44917=DIRECTION('ref_axis',(-1.02926399073076E-32,-0.707106781186552,-0.707106781186543));
#44918=DIRECTION('',(-1.,-4.38245930773088E-16,0.));
#44919=DIRECTION('center_axis',(-1.,-4.38245930773088E-16,0.));
#44920=DIRECTION('ref_axis',(4.38245930773088E-16,-1.,0.));
#44921=DIRECTION('',(-1.,-4.38245930773088E-16,0.));
#44922=DIRECTION('center_axis',(4.38245930773088E-16,-1.,1.8333618114597E-15));
#44923=DIRECTION('ref_axis',(1.09941607071732E-47,-1.8333618114597E-15,
-1.));
#44924=DIRECTION('',(-1.,-4.38245930773088E-16,0.));
#44925=DIRECTION('center_axis',(-1.,-4.38245930773088E-16,0.));
#44926=DIRECTION('ref_axis',(4.38245930773088E-16,-1.,0.));
#44927=DIRECTION('',(-1.,-4.38245930773088E-16,0.));
#44928=DIRECTION('center_axis',(3.09886669477059E-16,-0.707106781186544,
-0.707106781186551));
#44929=DIRECTION('ref_axis',(8.09901984815823E-33,0.707106781186551,-0.707106781186544));
#44930=DIRECTION('',(-1.,-4.38245930773088E-16,0.));
#44931=DIRECTION('center_axis',(-1.,-4.38245930773088E-16,0.));
#44932=DIRECTION('ref_axis',(4.38245930773088E-16,-1.,0.));
#44933=DIRECTION('',(-1.,-4.38245930773088E-16,0.));
#44934=DIRECTION('center_axis',(-5.83988792200131E-31,1.3325595315168E-15,
-1.));
#44935=DIRECTION('ref_axis',(0.,1.,1.3325595315168E-15));
#44936=DIRECTION('',(-1.,-4.38245930773088E-16,0.));
#44937=DIRECTION('center_axis',(-1.,-4.38245930773088E-16,0.));
#44938=DIRECTION('ref_axis',(4.38245930773088E-16,-1.,0.));
#44939=DIRECTION('',(-1.,-4.38245930773088E-16,0.));
#44940=DIRECTION('center_axis',(-4.38245930773088E-16,1.,0.));
#44941=DIRECTION('ref_axis',(-1.,-4.38245930773088E-16,0.));
#44942=DIRECTION('center_axis',(4.38245930773088E-16,-1.,2.77555756156289E-15));
#44943=DIRECTION('ref_axis',(1.03714524497726E-47,-2.77555756156289E-15,
-1.));
#44944=DIRECTION('',(-1.,-4.38245930773088E-16,0.));
#44945=DIRECTION('',(-1.,-4.38245930773088E-16,0.));
#44946=DIRECTION('center_axis',(0.,0.,-1.));
#44947=DIRECTION('ref_axis',(-1.,0.,0.));
#44948=DIRECTION('',(-1.,-4.38245930773088E-16,0.));
#44949=DIRECTION('center_axis',(-4.38245930773088E-16,1.,-4.16333634234433E-15));
#44950=DIRECTION('ref_axis',(3.63000835742038E-47,4.16333634234433E-15,
1.));
#44951=DIRECTION('',(-1.,-4.38245930773088E-16,0.));
#44952=DIRECTION('center_axis',(0.,0.,1.));
#44953=DIRECTION('ref_axis',(1.,0.,0.));
#44954=DIRECTION('center_axis',(0.,-0.707106781186548,-0.707106781186548));
#44955=DIRECTION('ref_axis',(1.,0.,0.));
#44956=DIRECTION('center_axis',(0.,0.707106781186548,0.707106781186548));
#44957=DIRECTION('ref_axis',(-1.,0.,0.));
#44958=DIRECTION('center_axis',(0.,-0.707106781186548,0.707106781186548));
#44959=DIRECTION('ref_axis',(1.,0.,0.));
#44960=DIRECTION('center_axis',(0.,-0.707106781186548,0.707106781186548));
#44961=DIRECTION('ref_axis',(1.,0.,0.));
#44962=DIRECTION('center_axis',(0.,0.,-1.));
#44963=DIRECTION('ref_axis',(-1.,0.,0.));
#44964=DIRECTION('',(1.,1.46081976924362E-16,0.));
#44965=DIRECTION('center_axis',(1.,1.46081976924362E-16,0.));
#44966=DIRECTION('ref_axis',(1.46081976924362E-16,-1.,1.22464679914735E-16));
#44967=DIRECTION('',(1.,1.46081976924362E-16,0.));
#44968=DIRECTION('center_axis',(0.,0.,-1.));
#44969=DIRECTION('ref_axis',(-1.,0.,0.));
#44970=DIRECTION('center_axis',(0.,0.,1.));
#44971=DIRECTION('ref_axis',(1.,0.,0.));
#44972=DIRECTION('',(1.,1.46081976924362E-16,0.));
#44973=DIRECTION('center_axis',(0.,0.,1.));
#44974=DIRECTION('ref_axis',(1.,0.,0.));
#44975=DIRECTION('',(1.,1.46081976924362E-16,0.));
#44976=DIRECTION('center_axis',(1.,1.46081976924362E-16,0.));
#44977=DIRECTION('ref_axis',(1.46081976924362E-16,-1.,1.22464679914735E-16));
#44978=DIRECTION('center_axis',(0.,0.,1.));
#44979=DIRECTION('ref_axis',(1.,0.,0.));
#44980=DIRECTION('',(1.,1.46081976924362E-16,0.));
#44981=DIRECTION('center_axis',(0.,0.,1.));
#44982=DIRECTION('ref_axis',(1.,0.,0.));
#44983=DIRECTION('',(1.,1.46081976924362E-16,0.));
#44984=DIRECTION('center_axis',(1.,1.46081976924362E-16,0.));
#44985=DIRECTION('ref_axis',(1.46081976924362E-16,-1.,1.22464679914735E-16));
#44986=DIRECTION('center_axis',(0.,0.,-1.));
#44987=DIRECTION('ref_axis',(-1.,0.,0.));
#44988=DIRECTION('',(1.,1.46081976924362E-16,0.));
#44989=DIRECTION('center_axis',(1.,1.46081976924362E-16,0.));
#44990=DIRECTION('ref_axis',(1.46081976924362E-16,-1.,1.22464679914735E-16));
#44991=DIRECTION('',(1.,1.46081976924362E-16,0.));
#44992=DIRECTION('center_axis',(0.,0.,-1.));
#44993=DIRECTION('ref_axis',(-1.,0.,0.));
#44994=DIRECTION('center_axis',(0.,0.,1.));
#44995=DIRECTION('ref_axis',(1.,0.,0.));
#44996=DIRECTION('',(1.,1.46081976924362E-16,0.));
#44997=DIRECTION('center_axis',(0.,0.,1.));
#44998=DIRECTION('ref_axis',(1.,0.,0.));
#44999=DIRECTION('',(1.,1.46081976924362E-16,0.));
#45000=DIRECTION('center_axis',(1.,1.46081976924362E-16,0.));
#45001=DIRECTION('ref_axis',(1.46081976924362E-16,-1.,1.22464679914735E-16));
#45002=DIRECTION('center_axis',(0.,0.,-1.));
#45003=DIRECTION('ref_axis',(-1.,0.,0.));
#45004=DIRECTION('',(1.,1.46081976924362E-16,0.));
#45005=DIRECTION('center_axis',(1.,1.46081976924362E-16,0.));
#45006=DIRECTION('ref_axis',(1.46081976924362E-16,-1.,1.22464679914735E-16));
#45007=DIRECTION('',(1.,1.46081976924362E-16,0.));
#45008=DIRECTION('center_axis',(0.,0.,-1.));
#45009=DIRECTION('ref_axis',(-1.,0.,0.));
#45010=DIRECTION('center_axis',(0.,0.,-1.));
#45011=DIRECTION('ref_axis',(-1.,0.,0.));
#45012=DIRECTION('',(1.,1.46081976924362E-16,0.));
#45013=DIRECTION('center_axis',(1.,1.46081976924362E-16,0.));
#45014=DIRECTION('ref_axis',(1.46081976924362E-16,-1.,1.22464679914735E-16));
#45015=DIRECTION('',(1.,1.46081976924362E-16,0.));
#45016=DIRECTION('center_axis',(0.,0.,-1.));
#45017=DIRECTION('ref_axis',(-1.,0.,0.));
#45018=DIRECTION('center_axis',(0.,0.,1.));
#45019=DIRECTION('ref_axis',(1.,0.,0.));
#45020=DIRECTION('',(1.,1.46081976924362E-16,0.));
#45021=DIRECTION('center_axis',(0.,0.,1.));
#45022=DIRECTION('ref_axis',(1.,0.,0.));
#45023=DIRECTION('',(1.,1.46081976924362E-16,0.));
#45024=DIRECTION('center_axis',(1.,1.46081976924362E-16,0.));
#45025=DIRECTION('ref_axis',(1.46081976924362E-16,-1.,1.22464679914735E-16));
#45026=DIRECTION('center_axis',(0.,0.,1.));
#45027=DIRECTION('ref_axis',(1.,0.,0.));
#45028=DIRECTION('',(1.,1.46081976924362E-16,0.));
#45029=DIRECTION('center_axis',(0.,0.,1.));
#45030=DIRECTION('ref_axis',(1.,0.,0.));
#45031=DIRECTION('',(1.,1.46081976924362E-16,0.));
#45032=DIRECTION('center_axis',(1.,1.46081976924362E-16,0.));
#45033=DIRECTION('ref_axis',(1.46081976924362E-16,-1.,1.22464679914735E-16));
#45034=DIRECTION('center_axis',(0.,0.,1.));
#45035=DIRECTION('ref_axis',(1.,0.,0.));
#45036=DIRECTION('',(1.,1.46081976924362E-16,0.));
#45037=DIRECTION('center_axis',(0.,0.,1.));
#45038=DIRECTION('ref_axis',(1.,0.,0.));
#45039=DIRECTION('',(1.,1.46081976924362E-16,0.));
#45040=DIRECTION('center_axis',(1.,1.46081976924362E-16,0.));
#45041=DIRECTION('ref_axis',(1.46081976924362E-16,-1.,1.22464679914735E-16));
#45042=DIRECTION('center_axis',(0.,0.,1.));
#45043=DIRECTION('ref_axis',(1.,0.,0.));
#45044=DIRECTION('',(1.,1.46081976924362E-16,0.));
#45045=DIRECTION('center_axis',(0.,0.,1.));
#45046=DIRECTION('ref_axis',(1.,0.,0.));
#45047=DIRECTION('',(1.,1.46081976924362E-16,0.));
#45048=DIRECTION('center_axis',(1.,1.46081976924362E-16,0.));
#45049=DIRECTION('ref_axis',(1.46081976924362E-16,-1.,1.22464679914735E-16));
#45050=DIRECTION('center_axis',(0.,0.,-1.));
#45051=DIRECTION('ref_axis',(-1.,0.,0.));
#45052=DIRECTION('',(1.,1.46081976924362E-16,0.));
#45053=DIRECTION('center_axis',(1.,1.46081976924362E-16,0.));
#45054=DIRECTION('ref_axis',(1.46081976924362E-16,-1.,1.22464679914735E-16));
#45055=DIRECTION('',(1.,1.46081976924362E-16,0.));
#45056=DIRECTION('center_axis',(0.,0.,-1.));
#45057=DIRECTION('ref_axis',(-1.,0.,0.));
#45058=DIRECTION('center_axis',(0.,0.,-1.));
#45059=DIRECTION('ref_axis',(-1.,0.,0.));
#45060=DIRECTION('',(1.,1.46081976924362E-16,0.));
#45061=DIRECTION('center_axis',(1.,1.46081976924362E-16,0.));
#45062=DIRECTION('ref_axis',(1.46081976924362E-16,-1.,1.22464679914735E-16));
#45063=DIRECTION('',(1.,1.46081976924362E-16,0.));
#45064=DIRECTION('center_axis',(0.,0.,-1.));
#45065=DIRECTION('ref_axis',(-1.,0.,0.));
#45066=DIRECTION('center_axis',(0.,0.,-1.));
#45067=DIRECTION('ref_axis',(-1.,0.,0.));
#45068=DIRECTION('',(1.,1.46081976924362E-16,0.));
#45069=DIRECTION('center_axis',(1.,1.46081976924362E-16,0.));
#45070=DIRECTION('ref_axis',(1.46081976924362E-16,-1.,1.22464679914735E-16));
#45071=DIRECTION('',(1.,1.46081976924362E-16,0.));
#45072=DIRECTION('center_axis',(0.,0.,-1.));
#45073=DIRECTION('ref_axis',(-1.,0.,0.));
#45074=DIRECTION('center_axis',(0.,0.,-1.));
#45075=DIRECTION('ref_axis',(-1.,0.,0.));
#45076=DIRECTION('',(1.,1.46081976924362E-16,0.));
#45077=DIRECTION('center_axis',(1.,1.46081976924362E-16,0.));
#45078=DIRECTION('ref_axis',(1.46081976924362E-16,-1.,1.22464679914735E-16));
#45079=DIRECTION('',(1.,1.46081976924362E-16,0.));
#45080=DIRECTION('center_axis',(0.,0.,-1.));
#45081=DIRECTION('ref_axis',(-1.,0.,0.));
#45082=DIRECTION('center_axis',(0.,0.,-1.));
#45083=DIRECTION('ref_axis',(-1.,0.,0.));
#45084=DIRECTION('',(1.,1.46081976924362E-16,0.));
#45085=DIRECTION('center_axis',(1.,1.46081976924362E-16,0.));
#45086=DIRECTION('ref_axis',(1.46081976924362E-16,-1.,1.22464679914735E-16));
#45087=DIRECTION('',(1.,1.46081976924362E-16,0.));
#45088=DIRECTION('center_axis',(0.,0.,-1.));
#45089=DIRECTION('ref_axis',(-1.,0.,0.));
#45090=DIRECTION('center_axis',(0.,0.,-1.));
#45091=DIRECTION('ref_axis',(-1.,0.,0.));
#45092=DIRECTION('',(1.,1.46081976924362E-16,0.));
#45093=DIRECTION('center_axis',(1.,1.46081976924362E-16,0.));
#45094=DIRECTION('ref_axis',(1.46081976924362E-16,-1.,1.22464679914735E-16));
#45095=DIRECTION('',(1.,1.46081976924362E-16,0.));
#45096=DIRECTION('center_axis',(0.,0.,-1.));
#45097=DIRECTION('ref_axis',(-1.,0.,0.));
#45098=DIRECTION('center_axis',(0.,0.,-1.));
#45099=DIRECTION('ref_axis',(-1.,0.,0.));
#45100=DIRECTION('',(1.,1.46081976924362E-16,0.));
#45101=DIRECTION('center_axis',(1.,1.46081976924362E-16,0.));
#45102=DIRECTION('ref_axis',(1.46081976924362E-16,-1.,1.22464679914735E-16));
#45103=DIRECTION('',(1.,1.46081976924362E-16,0.));
#45104=DIRECTION('center_axis',(0.,0.,-1.));
#45105=DIRECTION('ref_axis',(-1.,0.,0.));
#45106=DIRECTION('center_axis',(0.,0.,1.));
#45107=DIRECTION('ref_axis',(1.,0.,0.));
#45108=DIRECTION('',(1.,1.46081976924362E-16,0.));
#45109=DIRECTION('center_axis',(0.,0.,1.));
#45110=DIRECTION('ref_axis',(1.,0.,0.));
#45111=DIRECTION('',(1.,1.46081976924362E-16,0.));
#45112=DIRECTION('center_axis',(1.,1.46081976924362E-16,0.));
#45113=DIRECTION('ref_axis',(1.46081976924362E-16,-1.,1.22464679914735E-16));
#45114=DIRECTION('center_axis',(0.,0.,1.));
#45115=DIRECTION('ref_axis',(1.,0.,0.));
#45116=DIRECTION('',(1.,1.46081976924362E-16,0.));
#45117=DIRECTION('center_axis',(0.,0.,1.));
#45118=DIRECTION('ref_axis',(1.,0.,0.));
#45119=DIRECTION('',(1.,1.46081976924362E-16,0.));
#45120=DIRECTION('center_axis',(1.,1.46081976924362E-16,0.));
#45121=DIRECTION('ref_axis',(1.46081976924362E-16,-1.,1.22464679914735E-16));
#45122=DIRECTION('center_axis',(0.,0.,1.));
#45123=DIRECTION('ref_axis',(1.,0.,0.));
#45124=DIRECTION('',(1.,1.46081976924362E-16,0.));
#45125=DIRECTION('center_axis',(0.,0.,1.));
#45126=DIRECTION('ref_axis',(1.,0.,0.));
#45127=DIRECTION('',(1.,1.46081976924362E-16,0.));
#45128=DIRECTION('center_axis',(1.,1.46081976924362E-16,0.));
#45129=DIRECTION('ref_axis',(1.46081976924362E-16,-1.,1.22464679914735E-16));
#45130=DIRECTION('center_axis',(0.,0.,1.));
#45131=DIRECTION('ref_axis',(1.,0.,0.));
#45132=DIRECTION('',(1.,1.46081976924362E-16,0.));
#45133=DIRECTION('center_axis',(0.,0.,1.));
#45134=DIRECTION('ref_axis',(1.,0.,0.));
#45135=DIRECTION('',(1.,1.46081976924362E-16,0.));
#45136=DIRECTION('center_axis',(1.,1.46081976924362E-16,0.));
#45137=DIRECTION('ref_axis',(1.46081976924362E-16,-1.,1.22464679914735E-16));
#45138=DIRECTION('center_axis',(0.,0.,1.));
#45139=DIRECTION('ref_axis',(1.,0.,0.));
#45140=DIRECTION('',(1.,1.46081976924362E-16,0.));
#45141=DIRECTION('center_axis',(0.,0.,1.));
#45142=DIRECTION('ref_axis',(1.,0.,0.));
#45143=DIRECTION('',(1.,1.46081976924362E-16,0.));
#45144=DIRECTION('center_axis',(1.,1.46081976924362E-16,0.));
#45145=DIRECTION('ref_axis',(1.46081976924362E-16,-1.,1.22464679914735E-16));
#45146=DIRECTION('center_axis',(0.,0.,-1.));
#45147=DIRECTION('ref_axis',(-1.,0.,0.));
#45148=DIRECTION('',(1.,1.46081976924362E-16,0.));
#45149=DIRECTION('center_axis',(1.,1.46081976924362E-16,0.));
#45150=DIRECTION('ref_axis',(1.46081976924362E-16,-1.,1.22464679914735E-16));
#45151=DIRECTION('',(1.,1.46081976924362E-16,0.));
#45152=DIRECTION('center_axis',(0.,0.,-1.));
#45153=DIRECTION('ref_axis',(-1.,0.,0.));
#45154=DIRECTION('center_axis',(0.,0.,-1.));
#45155=DIRECTION('ref_axis',(-1.,0.,0.));
#45156=DIRECTION('',(1.,1.46081976924362E-16,0.));
#45157=DIRECTION('center_axis',(1.,1.46081976924362E-16,0.));
#45158=DIRECTION('ref_axis',(1.46081976924362E-16,-1.,1.22464679914735E-16));
#45159=DIRECTION('',(1.,1.46081976924362E-16,0.));
#45160=DIRECTION('center_axis',(0.,0.,-1.));
#45161=DIRECTION('ref_axis',(-1.,0.,0.));
#45162=DIRECTION('center_axis',(0.,0.,1.));
#45163=DIRECTION('ref_axis',(1.,0.,0.));
#45164=DIRECTION('',(1.,1.46081976924362E-16,0.));
#45165=DIRECTION('center_axis',(1.,1.46081976924362E-16,0.));
#45166=DIRECTION('ref_axis',(1.46081976924362E-16,-1.,1.22464679914735E-16));
#45167=DIRECTION('',(1.,1.46081976924362E-16,0.));
#45168=DIRECTION('center_axis',(0.,0.,1.));
#45169=DIRECTION('ref_axis',(1.,0.,0.));
#45170=DIRECTION('center_axis',(0.,0.,1.));
#45171=DIRECTION('ref_axis',(1.,0.,0.));
#45172=DIRECTION('',(1.,1.46081976924362E-16,0.));
#45173=DIRECTION('center_axis',(1.,1.46081976924362E-16,0.));
#45174=DIRECTION('ref_axis',(1.46081976924362E-16,-1.,1.22464679914735E-16));
#45175=DIRECTION('',(1.,1.46081976924362E-16,0.));
#45176=DIRECTION('center_axis',(0.,0.,1.));
#45177=DIRECTION('ref_axis',(1.,0.,0.));
#45178=DIRECTION('center_axis',(0.,0.,-1.));
#45179=DIRECTION('ref_axis',(-1.,0.,0.));
#45180=DIRECTION('',(1.,1.46081976924362E-16,0.));
#45181=DIRECTION('center_axis',(1.,1.46081976924362E-16,0.));
#45182=DIRECTION('ref_axis',(1.46081976924362E-16,-1.,1.22464679914735E-16));
#45183=DIRECTION('',(1.,1.46081976924362E-16,0.));
#45184=DIRECTION('center_axis',(0.,0.,-1.));
#45185=DIRECTION('ref_axis',(-1.,0.,0.));
#45186=DIRECTION('center_axis',(0.,0.,1.));
#45187=DIRECTION('ref_axis',(1.,0.,0.));
#45188=DIRECTION('',(1.,1.46081976924362E-16,0.));
#45189=DIRECTION('center_axis',(1.,1.46081976924362E-16,0.));
#45190=DIRECTION('ref_axis',(1.46081976924362E-16,-1.,1.22464679914735E-16));
#45191=DIRECTION('',(1.,1.46081976924362E-16,0.));
#45192=DIRECTION('center_axis',(0.,0.,1.));
#45193=DIRECTION('ref_axis',(1.,0.,0.));
#45194=DIRECTION('center_axis',(0.,0.,-1.));
#45195=DIRECTION('ref_axis',(-1.,0.,0.));
#45196=DIRECTION('',(1.,1.46081976924362E-16,0.));
#45197=DIRECTION('center_axis',(1.,1.46081976924362E-16,0.));
#45198=DIRECTION('ref_axis',(1.46081976924362E-16,-1.,1.22464679914735E-16));
#45199=DIRECTION('',(1.,1.46081976924362E-16,0.));
#45200=DIRECTION('center_axis',(0.,0.,-1.));
#45201=DIRECTION('ref_axis',(-1.,0.,0.));
#45202=DIRECTION('center_axis',(0.,0.,-1.));
#45203=DIRECTION('ref_axis',(-1.,0.,0.));
#45204=DIRECTION('',(1.,1.46081976924362E-16,0.));
#45205=DIRECTION('center_axis',(1.,1.46081976924362E-16,0.));
#45206=DIRECTION('ref_axis',(1.46081976924362E-16,-1.,1.22464679914735E-16));
#45207=DIRECTION('',(1.,1.46081976924362E-16,0.));
#45208=DIRECTION('center_axis',(0.,0.,-1.));
#45209=DIRECTION('ref_axis',(-1.,0.,0.));
#45210=DIRECTION('center_axis',(0.,0.,1.));
#45211=DIRECTION('ref_axis',(1.,0.,0.));
#45212=DIRECTION('',(1.,1.46081976924362E-16,0.));
#45213=DIRECTION('center_axis',(1.,1.46081976924362E-16,0.));
#45214=DIRECTION('ref_axis',(1.46081976924362E-16,-1.,1.22464679914735E-16));
#45215=DIRECTION('',(1.,1.46081976924362E-16,0.));
#45216=DIRECTION('center_axis',(0.,0.,1.));
#45217=DIRECTION('ref_axis',(1.,0.,0.));
#45218=DIRECTION('center_axis',(0.,0.,1.));
#45219=DIRECTION('ref_axis',(1.,0.,0.));
#45220=DIRECTION('',(1.,1.46081976924362E-16,0.));
#45221=DIRECTION('center_axis',(1.,1.46081976924362E-16,0.));
#45222=DIRECTION('ref_axis',(1.46081976924362E-16,-1.,1.22464679914735E-16));
#45223=DIRECTION('',(1.,1.46081976924362E-16,0.));
#45224=DIRECTION('center_axis',(0.,0.,1.));
#45225=DIRECTION('ref_axis',(1.,0.,0.));
#45226=DIRECTION('center_axis',(0.,0.,1.));
#45227=DIRECTION('ref_axis',(1.,0.,0.));
#45228=DIRECTION('',(1.,1.46081976924362E-16,0.));
#45229=DIRECTION('center_axis',(1.,1.46081976924362E-16,0.));
#45230=DIRECTION('ref_axis',(1.46081976924362E-16,-1.,1.22464679914735E-16));
#45231=DIRECTION('',(1.,1.46081976924362E-16,0.));
#45232=DIRECTION('center_axis',(0.,0.,1.));
#45233=DIRECTION('ref_axis',(1.,0.,0.));
#45234=DIRECTION('center_axis',(0.,0.,1.));
#45235=DIRECTION('ref_axis',(1.,0.,0.));
#45236=DIRECTION('',(1.,1.46081976924362E-16,0.));
#45237=DIRECTION('center_axis',(1.,1.46081976924362E-16,0.));
#45238=DIRECTION('ref_axis',(1.46081976924362E-16,-1.,1.22464679914735E-16));
#45239=DIRECTION('',(1.,1.46081976924362E-16,0.));
#45240=DIRECTION('center_axis',(0.,0.,1.));
#45241=DIRECTION('ref_axis',(1.,0.,0.));
#45242=DIRECTION('center_axis',(0.,0.,-1.));
#45243=DIRECTION('ref_axis',(-1.,0.,0.));
#45244=DIRECTION('',(1.,1.46081976924362E-16,0.));
#45245=DIRECTION('center_axis',(1.,1.46081976924362E-16,0.));
#45246=DIRECTION('ref_axis',(1.46081976924362E-16,-1.,1.22464679914735E-16));
#45247=DIRECTION('',(1.,1.46081976924362E-16,0.));
#45248=DIRECTION('center_axis',(0.,0.,-1.));
#45249=DIRECTION('ref_axis',(-1.,0.,0.));
#45250=DIRECTION('center_axis',(0.,0.,-1.));
#45251=DIRECTION('ref_axis',(-1.,0.,0.));
#45252=DIRECTION('',(1.,1.46081976924362E-16,0.));
#45253=DIRECTION('center_axis',(1.,1.46081976924362E-16,0.));
#45254=DIRECTION('ref_axis',(1.46081976924362E-16,-1.,1.22464679914735E-16));
#45255=DIRECTION('',(1.,1.46081976924362E-16,0.));
#45256=DIRECTION('center_axis',(0.,0.,-1.));
#45257=DIRECTION('ref_axis',(-1.,0.,0.));
#45258=DIRECTION('center_axis',(0.,0.,-1.));
#45259=DIRECTION('ref_axis',(-1.,0.,0.));
#45260=DIRECTION('',(1.,1.46081976924362E-16,0.));
#45261=DIRECTION('center_axis',(1.,1.46081976924362E-16,0.));
#45262=DIRECTION('ref_axis',(1.46081976924362E-16,-1.,1.22464679914735E-16));
#45263=DIRECTION('',(1.,1.46081976924362E-16,0.));
#45264=DIRECTION('center_axis',(0.,0.,-1.));
#45265=DIRECTION('ref_axis',(-1.,0.,0.));
#45266=DIRECTION('center_axis',(0.,0.,-1.));
#45267=DIRECTION('ref_axis',(-1.,0.,0.));
#45268=DIRECTION('',(1.,1.46081976924362E-16,0.));
#45269=DIRECTION('center_axis',(1.,1.46081976924362E-16,0.));
#45270=DIRECTION('ref_axis',(1.46081976924362E-16,-1.,1.22464679914735E-16));
#45271=DIRECTION('',(1.,1.46081976924362E-16,0.));
#45272=DIRECTION('center_axis',(0.,0.,-1.));
#45273=DIRECTION('ref_axis',(-1.,0.,0.));
#45274=DIRECTION('center_axis',(0.,0.,-1.));
#45275=DIRECTION('ref_axis',(-1.,0.,0.));
#45276=DIRECTION('',(1.,1.46081976924362E-16,0.));
#45277=DIRECTION('center_axis',(1.,1.46081976924362E-16,0.));
#45278=DIRECTION('ref_axis',(1.46081976924362E-16,-1.,1.22464679914735E-16));
#45279=DIRECTION('',(1.,1.46081976924362E-16,0.));
#45280=DIRECTION('center_axis',(0.,0.,-1.));
#45281=DIRECTION('ref_axis',(-1.,0.,0.));
#45282=DIRECTION('center_axis',(0.,0.,-1.));
#45283=DIRECTION('ref_axis',(-1.,0.,0.));
#45284=DIRECTION('',(1.,1.46081976924362E-16,0.));
#45285=DIRECTION('center_axis',(1.,1.46081976924362E-16,0.));
#45286=DIRECTION('ref_axis',(1.46081976924362E-16,-1.,1.22464679914735E-16));
#45287=DIRECTION('',(1.,1.46081976924362E-16,0.));
#45288=DIRECTION('center_axis',(0.,0.,-1.));
#45289=DIRECTION('ref_axis',(-1.,0.,0.));
#45290=DIRECTION('center_axis',(0.,0.,-1.));
#45291=DIRECTION('ref_axis',(-1.,0.,0.));
#45292=DIRECTION('',(1.,1.46081976924362E-16,0.));
#45293=DIRECTION('center_axis',(1.,1.46081976924362E-16,0.));
#45294=DIRECTION('ref_axis',(1.46081976924362E-16,-1.,1.22464679914735E-16));
#45295=DIRECTION('',(1.,1.46081976924362E-16,0.));
#45296=DIRECTION('center_axis',(0.,0.,-1.));
#45297=DIRECTION('ref_axis',(-1.,0.,0.));
#45298=DIRECTION('center_axis',(0.,0.,1.));
#45299=DIRECTION('ref_axis',(1.,0.,0.));
#45300=DIRECTION('',(1.,1.46081976924362E-16,0.));
#45301=DIRECTION('center_axis',(1.,1.46081976924362E-16,0.));
#45302=DIRECTION('ref_axis',(1.46081976924362E-16,-1.,1.22464679914735E-16));
#45303=DIRECTION('',(1.,1.46081976924362E-16,0.));
#45304=DIRECTION('center_axis',(0.,0.,1.));
#45305=DIRECTION('ref_axis',(1.,0.,0.));
#45306=DIRECTION('center_axis',(0.,0.,1.));
#45307=DIRECTION('ref_axis',(1.,0.,0.));
#45308=DIRECTION('',(1.,1.46081976924362E-16,0.));
#45309=DIRECTION('center_axis',(1.,1.46081976924362E-16,0.));
#45310=DIRECTION('ref_axis',(1.46081976924362E-16,-1.,1.22464679914735E-16));
#45311=DIRECTION('',(1.,1.46081976924362E-16,0.));
#45312=DIRECTION('center_axis',(0.,0.,1.));
#45313=DIRECTION('ref_axis',(1.,0.,0.));
#45314=DIRECTION('center_axis',(0.,0.,1.));
#45315=DIRECTION('ref_axis',(1.,0.,0.));
#45316=DIRECTION('',(1.,1.46081976924362E-16,0.));
#45317=DIRECTION('center_axis',(1.,1.46081976924362E-16,0.));
#45318=DIRECTION('ref_axis',(1.46081976924362E-16,-1.,1.22464679914735E-16));
#45319=DIRECTION('',(1.,1.46081976924362E-16,0.));
#45320=DIRECTION('center_axis',(0.,0.,1.));
#45321=DIRECTION('ref_axis',(1.,0.,0.));
#45322=DIRECTION('center_axis',(0.,0.,1.));
#45323=DIRECTION('ref_axis',(1.,0.,0.));
#45324=DIRECTION('',(1.,1.46081976924362E-16,0.));
#45325=DIRECTION('center_axis',(1.,1.46081976924362E-16,0.));
#45326=DIRECTION('ref_axis',(1.46081976924362E-16,-1.,1.22464679914735E-16));
#45327=DIRECTION('',(1.,1.46081976924362E-16,0.));
#45328=DIRECTION('center_axis',(0.,0.,1.));
#45329=DIRECTION('ref_axis',(1.,0.,0.));
#45330=DIRECTION('center_axis',(0.,0.,1.));
#45331=DIRECTION('ref_axis',(1.,0.,0.));
#45332=DIRECTION('',(1.,1.46081976924362E-16,0.));
#45333=DIRECTION('center_axis',(1.,1.46081976924362E-16,0.));
#45334=DIRECTION('ref_axis',(1.46081976924362E-16,-1.,1.22464679914735E-16));
#45335=DIRECTION('',(1.,1.46081976924362E-16,0.));
#45336=DIRECTION('center_axis',(0.,0.,1.));
#45337=DIRECTION('ref_axis',(1.,0.,0.));
#45338=DIRECTION('center_axis',(0.,0.,-1.));
#45339=DIRECTION('ref_axis',(-1.,0.,0.));
#45340=DIRECTION('',(1.,1.46081976924362E-16,0.));
#45341=DIRECTION('center_axis',(1.,1.46081976924362E-16,0.));
#45342=DIRECTION('ref_axis',(1.46081976924362E-16,-1.,1.22464679914735E-16));
#45343=DIRECTION('',(1.,1.46081976924362E-16,0.));
#45344=DIRECTION('center_axis',(0.,0.,-1.));
#45345=DIRECTION('ref_axis',(-1.,0.,0.));
#45346=DIRECTION('center_axis',(-1.,-2.30915603506606E-31,-3.77113799125394E-15));
#45347=DIRECTION('ref_axis',(-3.77113799125394E-15,0.,1.));
#45348=DIRECTION('',(0.,-1.,6.12323399573677E-17));
#45349=DIRECTION('center_axis',(0.,6.12323399573677E-17,1.));
#45350=DIRECTION('ref_axis',(0.,-1.,6.12323399573677E-17));
#45351=DIRECTION('',(0.,-1.,6.12323399573677E-17));
#45352=DIRECTION('center_axis',(1.,0.,0.));
#45353=DIRECTION('ref_axis',(0.,0.,-1.));
#45354=DIRECTION('',(0.,-1.,0.));
#45355=DIRECTION('center_axis',(-1.,0.,0.));
#45356=DIRECTION('ref_axis',(0.,0.,1.));
#45357=DIRECTION('',(0.,-1.,0.));
#45358=DIRECTION('',(0.,-1.,6.12323399573677E-17));
#45359=DIRECTION('center_axis',(0.,6.12323399573677E-17,1.));
#45360=DIRECTION('ref_axis',(0.,-1.,6.12323399573677E-17));
#45361=DIRECTION('',(0.,-1.,6.12323399573677E-17));
#45362=DIRECTION('center_axis',(1.,0.,0.));
#45363=DIRECTION('ref_axis',(0.,0.,-1.));
#45364=DIRECTION('center_axis',(-1.,0.,0.));
#45365=DIRECTION('ref_axis',(0.,0.,1.));
#45366=DIRECTION('',(0.,0.,1.));
#45367=DIRECTION('center_axis',(-1.,0.,0.));
#45368=DIRECTION('ref_axis',(0.,0.,-1.));
#45369=DIRECTION('center_axis',(-1.,0.,0.));
#45370=DIRECTION('ref_axis',(0.,0.,-1.));
#45371=DIRECTION('center_axis',(-1.,0.,0.));
#45372=DIRECTION('ref_axis',(0.,0.,1.));
#45373=DIRECTION('center_axis',(1.,0.,0.));
#45374=DIRECTION('ref_axis',(0.,0.,-1.));
#45375=DIRECTION('',(0.,0.,1.));
#45376=DIRECTION('center_axis',(1.,0.,0.));
#45377=DIRECTION('ref_axis',(0.,0.,-1.));
#45378=DIRECTION('center_axis',(1.,0.,0.));
#45379=DIRECTION('ref_axis',(0.,0.,1.));
#45380=DIRECTION('center_axis',(1.,0.,0.));
#45381=DIRECTION('ref_axis',(0.,0.,1.));
#45382=DIRECTION('center_axis',(-1.,-1.15648231731787E-15,0.));
#45383=DIRECTION('ref_axis',(1.15648231731787E-15,-1.,0.));
#45384=DIRECTION('',(0.,0.,-1.));
#45385=DIRECTION('center_axis',(1.,0.,0.));
#45386=DIRECTION('ref_axis',(0.,0.,-1.));
#45387=DIRECTION('',(0.,0.,-1.));
#45388=DIRECTION('center_axis',(0.,0.,-1.));
#45389=DIRECTION('ref_axis',(-1.,0.,0.));
#45390=DIRECTION('',(0.,0.,-1.));
#45391=DIRECTION('center_axis',(3.56237856673809E-16,-1.,0.));
#45392=DIRECTION('ref_axis',(1.,3.56237856673809E-16,0.));
#45393=DIRECTION('',(0.,0.,-1.));
#45394=DIRECTION('center_axis',(0.,0.,-1.));
#45395=DIRECTION('ref_axis',(-1.,0.,0.));
#45396=DIRECTION('center_axis',(0.,-1.,0.));
#45397=DIRECTION('ref_axis',(-1.,0.,0.));
#45398=DIRECTION('center_axis',(0.,-1.,0.));
#45399=DIRECTION('ref_axis',(-1.,0.,0.));
#45400=DIRECTION('center_axis',(0.,-1.,0.));
#45401=DIRECTION('ref_axis',(-1.,0.,0.));
#45402=DIRECTION('center_axis',(0.,-1.,0.));
#45403=DIRECTION('ref_axis',(-1.,0.,0.));
#45404=DIRECTION('center_axis',(0.,1.,0.));
#45405=DIRECTION('ref_axis',(-1.,0.,0.));
#45406=DIRECTION('center_axis',(0.,1.,0.));
#45407=DIRECTION('ref_axis',(-1.,0.,0.));
#45408=DIRECTION('center_axis',(0.,-1.,0.));
#45409=DIRECTION('ref_axis',(-1.,0.,0.));
#45410=DIRECTION('center_axis',(0.,-1.,0.));
#45411=DIRECTION('ref_axis',(-1.,0.,0.));
#45412=DIRECTION('',(0.,-1.,0.));
#45413=DIRECTION('center_axis',(0.,1.,0.));
#45414=DIRECTION('ref_axis',(-1.,0.,0.));
#45415=DIRECTION('center_axis',(0.,-1.,0.));
#45416=DIRECTION('ref_axis',(-1.,0.,0.));
#45417=DIRECTION('center_axis',(0.,1.,0.));
#45418=DIRECTION('ref_axis',(-1.,0.,0.));
#45419=DIRECTION('',(0.,1.,0.));
#45420=DIRECTION('center_axis',(0.,-1.,0.));
#45421=DIRECTION('ref_axis',(-1.,0.,0.));
#45422=DIRECTION('center_axis',(0.,1.,0.));
#45423=DIRECTION('ref_axis',(0.,0.,1.));
#45424=DIRECTION('center_axis',(0.,1.,0.));
#45425=DIRECTION('ref_axis',(0.,0.,-1.));
#45426=DIRECTION('',(0.42443387623072,0.,-0.905458935958868));
#45427=DIRECTION('center_axis',(0.,-1.,0.));
#45428=DIRECTION('ref_axis',(0.,0.,-1.));
#45429=DIRECTION('',(1.,0.,0.));
#45430=DIRECTION('center_axis',(0.,-1.,0.));
#45431=DIRECTION('ref_axis',(0.,0.,-1.));
#45432=DIRECTION('',(0.42443387623072,0.,0.905458935958868));
#45433=DIRECTION('center_axis',(0.,1.,0.));
#45434=DIRECTION('ref_axis',(0.,0.,-1.));
#45435=DIRECTION('',(0.42443387623072,0.,0.905458935958868));
#45436=DIRECTION('center_axis',(0.,-1.,0.));
#45437=DIRECTION('ref_axis',(-1.,0.,0.));
#45438=DIRECTION('',(1.,0.,0.));
#45439=DIRECTION('center_axis',(0.,-1.,0.));
#45440=DIRECTION('ref_axis',(-1.,0.,0.));
#45441=DIRECTION('',(0.42443387623072,0.,-0.905458935958868));
#45442=DIRECTION('center_axis',(0.,1.,0.));
#45443=DIRECTION('ref_axis',(0.42443387623072,0.,0.905458935958868));
#45444=DIRECTION('center_axis',(0.,-1.,0.));
#45445=DIRECTION('ref_axis',(0.,0.,-1.));
#45446=DIRECTION('',(0.42443387623072,0.,0.905458935958868));
#45447=DIRECTION('center_axis',(0.,1.,0.));
#45448=DIRECTION('ref_axis',(0.,0.,-1.));
#45449=DIRECTION('',(1.,0.,0.));
#45450=DIRECTION('center_axis',(0.,1.,0.));
#45451=DIRECTION('ref_axis',(0.,0.,-1.));
#45452=DIRECTION('',(0.42443387623072,0.,-0.905458935958868));
#45453=DIRECTION('center_axis',(0.,-1.,0.));
#45454=DIRECTION('ref_axis',(0.,0.,-1.));
#45455=DIRECTION('',(0.42443387623072,0.,-0.905458935958868));
#45456=DIRECTION('center_axis',(0.,1.,0.));
#45457=DIRECTION('ref_axis',(-1.,0.,0.));
#45458=DIRECTION('',(1.,0.,0.));
#45459=DIRECTION('center_axis',(0.,1.,0.));
#45460=DIRECTION('ref_axis',(-1.,0.,0.));
#45461=DIRECTION('',(0.42443387623072,0.,0.905458935958868));
#45462=DIRECTION('center_axis',(0.,-1.,0.));
#45463=DIRECTION('ref_axis',(-1.,0.,0.));
#45464=DIRECTION('',(0.,-1.,0.));
#45465=DIRECTION('',(0.,1.,0.));
#45466=DIRECTION('center_axis',(0.,-1.,0.));
#45467=DIRECTION('ref_axis',(-1.,0.,0.));
#45468=DIRECTION('',(0.,-1.,0.));
#45469=DIRECTION('',(0.,1.,0.));
#45470=DIRECTION('center_axis',(0.905458935958868,0.,-0.42443387623072));
#45471=DIRECTION('ref_axis',(0.42443387623072,0.,0.905458935958868));
#45472=DIRECTION('center_axis',(-0.905458935958868,0.,-0.42443387623072));
#45473=DIRECTION('ref_axis',(0.42443387623072,0.,-0.905458935958868));
#45474=DIRECTION('center_axis',(0.,0.,-1.));
#45475=DIRECTION('ref_axis',(0.,-1.,0.));
#45476=DIRECTION('center_axis',(0.,-1.,0.));
#45477=DIRECTION('ref_axis',(-1.,0.,0.));
#45478=DIRECTION('',(0.,1.,0.));
#45479=DIRECTION('',(0.,-1.,0.));
#45480=DIRECTION('center_axis',(0.,-1.,0.));
#45481=DIRECTION('ref_axis',(-1.,0.,0.));
#45482=DIRECTION('',(0.,1.,0.));
#45483=DIRECTION('',(0.,-1.,0.));
#45484=DIRECTION('center_axis',(0.,-1.,0.));
#45485=DIRECTION('ref_axis',(-1.,0.,0.));
#45486=DIRECTION('',(0.,1.,0.));
#45487=DIRECTION('center_axis',(0.,-1.,0.));
#45488=DIRECTION('ref_axis',(-1.,0.,0.));
#45489=DIRECTION('',(0.,-1.,0.));
#45490=DIRECTION('center_axis',(0.905458935958868,0.,-0.42443387623072));
#45491=DIRECTION('ref_axis',(0.42443387623072,0.,0.905458935958868));
#45492=DIRECTION('center_axis',(-0.905458935958868,0.,-0.42443387623072));
#45493=DIRECTION('ref_axis',(0.42443387623072,0.,-0.905458935958868));
#45494=DIRECTION('center_axis',(0.,0.,-1.));
#45495=DIRECTION('ref_axis',(0.,-1.,0.));
#45496=DIRECTION('center_axis',(5.8432790769745E-16,-1.,0.));
#45497=DIRECTION('ref_axis',(1.,5.8432790769745E-16,0.));
#45498=DIRECTION('center_axis',(-5.8432790769745E-16,1.,0.));
#45499=DIRECTION('ref_axis',(1.,5.8432790769745E-16,0.));
#45500=DIRECTION('center_axis',(-5.8432790769745E-16,1.,0.));
#45501=DIRECTION('ref_axis',(1.,5.8432790769745E-16,0.));
#45502=DIRECTION('center_axis',(5.8432790769745E-16,-1.,0.));
#45503=DIRECTION('ref_axis',(1.,5.8432790769745E-16,0.));
#45504=DIRECTION('center_axis',(5.8432790769745E-16,-1.,0.));
#45505=DIRECTION('ref_axis',(1.,5.8432790769745E-16,0.));
#45506=DIRECTION('center_axis',(5.8432790769745E-16,-1.,0.));
#45507=DIRECTION('ref_axis',(1.,5.8432790769745E-16,0.));
#45508=DIRECTION('center_axis',(5.8432790769745E-16,-1.,0.));
#45509=DIRECTION('ref_axis',(1.,5.8432790769745E-16,0.));
#45510=DIRECTION('center_axis',(5.8432790769745E-16,-1.,0.));
#45511=DIRECTION('ref_axis',(1.,5.8432790769745E-16,-6.93889390390722E-15));
#45512=DIRECTION('',(5.8432790769745E-16,-1.,0.));
#45513=DIRECTION('center_axis',(-5.8432790769745E-16,1.,0.));
#45514=DIRECTION('ref_axis',(1.,5.8432790769745E-16,0.));
#45515=DIRECTION('center_axis',(5.8432790769745E-16,-1.,0.));
#45516=DIRECTION('ref_axis',(1.,5.8432790769745E-16,0.));
#45517=DIRECTION('center_axis',(-5.8432790769745E-16,1.,0.));
#45518=DIRECTION('ref_axis',(1.,5.8432790769745E-16,0.));
#45519=DIRECTION('',(-5.8432790769745E-16,1.,0.));
#45520=DIRECTION('center_axis',(5.8432790769745E-16,-1.,0.));
#45521=DIRECTION('ref_axis',(1.,5.8432790769745E-16,0.));
#45522=DIRECTION('center_axis',(5.8432790769745E-16,-1.,0.));
#45523=DIRECTION('ref_axis',(1.,5.8432790769745E-16,0.));
#45524=DIRECTION('center_axis',(5.8432790769745E-16,-1.,0.));
#45525=DIRECTION('ref_axis',(1.,5.8432790769745E-16,0.));
#45526=DIRECTION('',(-0.42443387623072,-2.48008558853815E-16,0.905458935958868));
#45527=DIRECTION('center_axis',(-5.8432790769745E-16,1.,0.));
#45528=DIRECTION('ref_axis',(1.,5.8432790769745E-16,0.));
#45529=DIRECTION('',(-1.,-5.8432790769745E-16,0.));
#45530=DIRECTION('center_axis',(-5.8432790769745E-16,1.,0.));
#45531=DIRECTION('ref_axis',(1.,5.8432790769745E-16,0.));
#45532=DIRECTION('',(-0.42443387623072,-2.48008558853815E-16,-0.905458935958868));
#45533=DIRECTION('center_axis',(5.8432790769745E-16,-1.,0.));
#45534=DIRECTION('ref_axis',(1.,5.8432790769745E-16,0.));
#45535=DIRECTION('',(-0.42443387623072,-2.48008558853815E-16,-0.905458935958868));
#45536=DIRECTION('center_axis',(-5.8432790769745E-16,1.,0.));
#45537=DIRECTION('ref_axis',(1.,5.8432790769745E-16,0.));
#45538=DIRECTION('',(-1.,-5.8432790769745E-16,0.));
#45539=DIRECTION('center_axis',(-5.8432790769745E-16,1.,0.));
#45540=DIRECTION('ref_axis',(1.,5.8432790769745E-16,0.));
#45541=DIRECTION('',(-0.42443387623072,-2.48008558853815E-16,0.905458935958868));
#45542=DIRECTION('center_axis',(5.8432790769745E-16,-1.,0.));
#45543=DIRECTION('ref_axis',(-1.,-5.8432790769745E-16,0.));
#45544=DIRECTION('center_axis',(-5.8432790769745E-16,1.,0.));
#45545=DIRECTION('ref_axis',(1.,5.8432790769745E-16,0.));
#45546=DIRECTION('',(-0.42443387623072,-2.48008558853815E-16,-0.905458935958868));
#45547=DIRECTION('center_axis',(5.8432790769745E-16,-1.,0.));
#45548=DIRECTION('ref_axis',(1.,5.8432790769745E-16,0.));
#45549=DIRECTION('',(-1.,-5.8432790769745E-16,0.));
#45550=DIRECTION('center_axis',(5.8432790769745E-16,-1.,0.));
#45551=DIRECTION('ref_axis',(1.,5.8432790769745E-16,0.));
#45552=DIRECTION('',(-0.42443387623072,-2.48008558853815E-16,0.905458935958868));
#45553=DIRECTION('center_axis',(-5.8432790769745E-16,1.,0.));
#45554=DIRECTION('ref_axis',(1.,5.8432790769745E-16,0.));
#45555=DIRECTION('',(-0.42443387623072,-2.48008558853815E-16,0.905458935958868));
#45556=DIRECTION('center_axis',(5.8432790769745E-16,-1.,0.));
#45557=DIRECTION('ref_axis',(1.,5.8432790769745E-16,0.));
#45558=DIRECTION('',(-1.,-5.8432790769745E-16,0.));
#45559=DIRECTION('center_axis',(5.8432790769745E-16,-1.,0.));
#45560=DIRECTION('ref_axis',(1.,5.8432790769745E-16,0.));
#45561=DIRECTION('',(-0.42443387623072,-2.48008558853815E-16,-0.905458935958868));
#45562=DIRECTION('center_axis',(5.8432790769745E-16,-1.,0.));
#45563=DIRECTION('ref_axis',(1.,5.8432790769745E-16,0.));
#45564=DIRECTION('',(-5.8432790769745E-16,1.,0.));
#45565=DIRECTION('',(5.8432790769745E-16,-1.,0.));
#45566=DIRECTION('center_axis',(5.8432790769745E-16,-1.,0.));
#45567=DIRECTION('ref_axis',(1.,5.8432790769745E-16,0.));
#45568=DIRECTION('',(-5.8432790769745E-16,1.,0.));
#45569=DIRECTION('',(5.8432790769745E-16,-1.,0.));
#45570=DIRECTION('center_axis',(-0.905458935958868,-5.29084925554805E-16,
-0.42443387623072));
#45571=DIRECTION('ref_axis',(-0.42443387623072,-2.48008558853815E-16,0.905458935958868));
#45572=DIRECTION('center_axis',(0.905458935958868,5.29084925554805E-16,
-0.42443387623072));
#45573=DIRECTION('ref_axis',(-0.42443387623072,-2.48008558853815E-16,-0.905458935958868));
#45574=DIRECTION('center_axis',(0.,0.,-1.));
#45575=DIRECTION('ref_axis',(5.8432790769745E-16,-1.,0.));
#45576=DIRECTION('center_axis',(5.8432790769745E-16,-1.,0.));
#45577=DIRECTION('ref_axis',(1.,5.8432790769745E-16,0.));
#45578=DIRECTION('',(5.8432790769745E-16,-1.,0.));
#45579=DIRECTION('',(-5.8432790769745E-16,1.,0.));
#45580=DIRECTION('center_axis',(5.8432790769745E-16,-1.,0.));
#45581=DIRECTION('ref_axis',(1.,5.8432790769745E-16,0.));
#45582=DIRECTION('',(5.8432790769745E-16,-1.,0.));
#45583=DIRECTION('',(-5.8432790769745E-16,1.,0.));
#45584=DIRECTION('center_axis',(5.8432790769745E-16,-1.,0.));
#45585=DIRECTION('ref_axis',(1.,5.8432790769745E-16,0.));
#45586=DIRECTION('',(-5.8432790769745E-16,1.,0.));
#45587=DIRECTION('center_axis',(5.8432790769745E-16,-1.,0.));
#45588=DIRECTION('ref_axis',(1.,5.8432790769745E-16,0.));
#45589=DIRECTION('',(5.8432790769745E-16,-1.,0.));
#45590=DIRECTION('center_axis',(-0.905458935958868,-5.29084925554805E-16,
-0.42443387623072));
#45591=DIRECTION('ref_axis',(-0.42443387623072,-2.48008558853815E-16,0.905458935958868));
#45592=DIRECTION('center_axis',(0.905458935958868,5.29084925554805E-16,
-0.42443387623072));
#45593=DIRECTION('ref_axis',(-0.42443387623072,-2.48008558853815E-16,-0.905458935958868));
#45594=DIRECTION('center_axis',(0.,0.,-1.));
#45595=DIRECTION('ref_axis',(5.8432790769745E-16,-1.,0.));
#45596=DIRECTION('center_axis',(1.,0.,0.));
#45597=DIRECTION('ref_axis',(0.,0.,-1.));
#45598=DIRECTION('',(0.,-1.,6.12323399573677E-17));
#45599=DIRECTION('center_axis',(0.,-6.12323399573677E-17,-1.));
#45600=DIRECTION('ref_axis',(0.,1.,-6.12323399573677E-17));
#45601=DIRECTION('',(0.,-1.,6.12323399573677E-17));
#45602=DIRECTION('center_axis',(-1.,0.,0.));
#45603=DIRECTION('ref_axis',(0.,0.,1.));
#45604=DIRECTION('',(0.,-1.,0.));
#45605=DIRECTION('center_axis',(1.,0.,0.));
#45606=DIRECTION('ref_axis',(0.,0.,-1.));
#45607=DIRECTION('',(0.,-1.,0.));
#45608=DIRECTION('',(0.,-1.,6.12323399573677E-17));
#45609=DIRECTION('center_axis',(0.,-6.12323399573677E-17,-1.));
#45610=DIRECTION('ref_axis',(0.,1.,-6.12323399573677E-17));
#45611=DIRECTION('',(0.,-1.,6.12323399573677E-17));
#45612=DIRECTION('center_axis',(-1.,2.30915603506606E-31,3.77113799125394E-15));
#45613=DIRECTION('ref_axis',(3.77113799125394E-15,0.,1.));
#45614=DIRECTION('center_axis',(1.,0.,0.));
#45615=DIRECTION('ref_axis',(0.,0.,-1.));
#45616=DIRECTION('',(-8.07567285923481E-30,6.98296267768627E-15,-1.));
#45617=DIRECTION('center_axis',(1.,0.,0.));
#45618=DIRECTION('ref_axis',(0.,0.,1.));
#45619=DIRECTION('center_axis',(1.,0.,0.));
#45620=DIRECTION('ref_axis',(0.,0.,1.));
#45621=DIRECTION('center_axis',(1.,0.,0.));
#45622=DIRECTION('ref_axis',(0.,0.,-1.));
#45623=DIRECTION('center_axis',(-1.,0.,0.));
#45624=DIRECTION('ref_axis',(0.,0.,1.));
#45625=DIRECTION('',(0.,6.98296267768627E-15,-1.));
#45626=DIRECTION('center_axis',(-1.,0.,0.));
#45627=DIRECTION('ref_axis',(0.,0.,1.));
#45628=DIRECTION('center_axis',(-1.,0.,0.));
#45629=DIRECTION('ref_axis',(0.,0.,-1.));
#45630=DIRECTION('',(1.,-8.07567285923482E-31,0.));
#45631=DIRECTION('center_axis',(-1.,0.,0.));
#45632=DIRECTION('ref_axis',(0.,0.,-1.));
#45633=DIRECTION('',(-1.,8.07567285923482E-31,0.));
#45634=DIRECTION('center_axis',(1.,1.15648231731787E-15,0.));
#45635=DIRECTION('ref_axis',(-1.15648231731787E-15,1.,0.));
#45636=DIRECTION('',(-1.15648231731787E-15,1.,0.));
#45637=DIRECTION('',(-1.15648231731787E-15,1.,0.));
#45638=DIRECTION('',(0.,0.,1.));
#45639=DIRECTION('center_axis',(-1.,0.,0.));
#45640=DIRECTION('ref_axis',(0.,0.,1.));
#45641=DIRECTION('',(0.,-1.,0.));
#45642=DIRECTION('',(0.,-1.,0.));
#45643=DIRECTION('',(0.,0.,1.));
#45644=DIRECTION('center_axis',(0.,0.,1.));
#45645=DIRECTION('ref_axis',(-1.,0.,0.));
#45646=DIRECTION('center_axis',(0.,0.,1.));
#45647=DIRECTION('ref_axis',(1.,0.,0.));
#45648=DIRECTION('',(-1.,-3.56237856673809E-16,0.));
#45649=DIRECTION('center_axis',(0.,0.,1.));
#45650=DIRECTION('ref_axis',(1.,0.,0.));
#45651=DIRECTION('center_axis',(0.,0.,1.));
#45652=DIRECTION('ref_axis',(-1.,0.,0.));
#45653=DIRECTION('center_axis',(0.,0.,1.));
#45654=DIRECTION('ref_axis',(1.,0.,0.));
#45655=DIRECTION('',(-1.,-3.56237856673809E-16,0.));
#45656=DIRECTION('center_axis',(0.,0.,1.));
#45657=DIRECTION('ref_axis',(1.,0.,0.));
#45658=DIRECTION('center_axis',(0.,0.,1.));
#45659=DIRECTION('ref_axis',(1.,0.,0.));
#45660=DIRECTION('',(0.,0.,1.));
#45661=DIRECTION('center_axis',(-3.56237856673809E-16,1.,0.));
#45662=DIRECTION('ref_axis',(-1.,-3.56237856673809E-16,0.));
#45663=DIRECTION('',(0.,0.,1.));
#45664=DIRECTION('center_axis',(0.,0.,1.));
#45665=DIRECTION('ref_axis',(1.,0.,0.));
#45666=DIRECTION('axis',(0.,0.,1.));
#45667=DIRECTION('refdir',(1.,0.,0.));
#45668=DIRECTION('center_axis',(1.,0.,0.));
#45669=DIRECTION('ref_axis',(0.,0.,-1.));
#45670=DIRECTION('center_axis',(1.,0.,0.));
#45671=DIRECTION('ref_axis',(0.,0.,-1.));
#45672=DIRECTION('',(1.,0.,0.));
#45673=DIRECTION('center_axis',(1.,0.,0.));
#45674=DIRECTION('ref_axis',(0.,0.,-1.));
#45675=DIRECTION('center_axis',(1.,0.,0.));
#45676=DIRECTION('ref_axis',(0.,0.,-1.));
#45677=DIRECTION('center_axis',(-1.,0.,0.));
#45678=DIRECTION('ref_axis',(0.,0.,1.));
#45679=DIRECTION('',(1.,0.,0.));
#45680=DIRECTION('center_axis',(1.,0.,0.));
#45681=DIRECTION('ref_axis',(0.,0.,-1.));
#45682=DIRECTION('center_axis',(1.,0.,0.));
#45683=DIRECTION('ref_axis',(0.,0.,-1.));
#45684=DIRECTION('center_axis',(-1.,2.06958181338202E-16,0.));
#45685=DIRECTION('ref_axis',(2.06958181338202E-16,1.,0.));
#45686=DIRECTION('',(1.,0.,0.));
#45687=DIRECTION('center_axis',(-1.,-1.29348863336376E-16,0.));
#45688=DIRECTION('ref_axis',(-1.29348863336376E-16,1.,0.));
#45689=DIRECTION('center_axis',(0.,0.,1.));
#45690=DIRECTION('ref_axis',(1.,0.,0.));
#45691=DIRECTION('center_axis',(0.,0.,1.));
#45692=DIRECTION('ref_axis',(-1.,0.,0.));
#45693=DIRECTION('center_axis',(0.,0.,1.));
#45694=DIRECTION('ref_axis',(-1.,0.,0.));
#45695=DIRECTION('',(-0.656059028990511,-8.0344058990495E-17,0.754709580222769));
#45696=DIRECTION('center_axis',(0.,0.,-1.));
#45697=DIRECTION('ref_axis',(-1.,0.,0.));
#45698=DIRECTION('center_axis',(0.,0.,1.));
#45699=DIRECTION('ref_axis',(1.,0.,0.));
#45700=DIRECTION('center_axis',(0.,0.,1.));
#45701=DIRECTION('ref_axis',(-1.,0.,0.));
#45702=DIRECTION('center_axis',(0.,0.,1.));
#45703=DIRECTION('ref_axis',(-1.,0.,0.));
#45704=DIRECTION('',(-0.656059028990511,-8.0344058990495E-17,0.754709580222769));
#45705=DIRECTION('center_axis',(0.,0.,-1.));
#45706=DIRECTION('ref_axis',(-1.,0.,0.));
#45707=DIRECTION('center_axis',(0.,0.,-1.));
#45708=DIRECTION('ref_axis',(-1.,0.,0.));
#45709=DIRECTION('',(0.,0.,-1.));
#45710=DIRECTION('center_axis',(0.,0.,-1.));
#45711=DIRECTION('ref_axis',(-1.,0.,0.));
#45712=DIRECTION('center_axis',(0.,0.,-1.));
#45713=DIRECTION('ref_axis',(-1.,0.,0.));
#45714=DIRECTION('center_axis',(0.,0.,1.));
#45715=DIRECTION('ref_axis',(1.,0.,0.));
#45716=DIRECTION('',(0.,0.,-1.));
#45717=DIRECTION('center_axis',(0.,0.,1.));
#45718=DIRECTION('ref_axis',(1.,0.,0.));
#45719=DIRECTION('',(0.,0.,-1.));
#45720=DIRECTION('center_axis',(0.,0.,-1.));
#45721=DIRECTION('ref_axis',(-1.,0.,0.));
#45722=DIRECTION('',(0.,0.,-1.));
#45723=DIRECTION('center_axis',(0.,0.,-1.));
#45724=DIRECTION('ref_axis',(-1.,0.,0.));
#45725=DIRECTION('center_axis',(0.,0.,-1.));
#45726=DIRECTION('ref_axis',(-1.,0.,0.));
#45727=DIRECTION('center_axis',(0.,0.,-1.));
#45728=DIRECTION('ref_axis',(-1.,0.,0.));
#45729=DIRECTION('',(1.,0.,0.));
#45730=DIRECTION('center_axis',(0.,0.,1.));
#45731=DIRECTION('ref_axis',(1.,0.,0.));
#45732=DIRECTION('',(-2.33197918015441E-16,1.,0.));
#45733=DIRECTION('center_axis',(0.,0.,-1.));
#45734=DIRECTION('ref_axis',(-1.,0.,0.));
#45735=DIRECTION('',(-0.707106781186543,-0.707106781186552,0.));
#45736=DIRECTION('center_axis',(0.,0.,1.));
#45737=DIRECTION('ref_axis',(1.,0.,0.));
#45738=DIRECTION('',(-1.,3.20838317005448E-16,0.));
#45739=DIRECTION('center_axis',(0.,0.,-1.));
#45740=DIRECTION('ref_axis',(-1.,0.,0.));
#45741=DIRECTION('',(0.707106781186544,-0.707106781186551,0.));
#45742=DIRECTION('center_axis',(0.,0.,1.));
#45743=DIRECTION('ref_axis',(1.,0.,0.));
#45744=DIRECTION('',(2.33197918015441E-16,-1.,0.));
#45745=DIRECTION('',(6.96899998383741E-17,1.,0.));
#45746=DIRECTION('',(1.,0.,0.));
#45747=DIRECTION('',(1.39379999676748E-16,-1.,0.));
#45748=DIRECTION('',(-1.,0.,0.));
#45749=DIRECTION('',(-1.39379999676748E-16,1.,0.));
#45750=DIRECTION('',(1.,6.44303772090628E-16,0.));
#45751=DIRECTION('',(5.57519998706993E-16,-1.,0.));
#45752=DIRECTION('',(-1.,0.,0.));
#45753=DIRECTION('',(1.,0.,0.));
#45754=DIRECTION('',(-2.78759999353496E-16,-1.,0.));
#45755=DIRECTION('',(-1.,-6.44303772090628E-16,0.));
#45756=DIRECTION('',(2.78759999353496E-16,1.,0.));
#45757=DIRECTION('center_axis',(1.,1.55218636003651E-16,0.));
#45758=DIRECTION('ref_axis',(-1.55218636003651E-16,1.,0.));
#45759=DIRECTION('',(1.55218636003651E-16,-1.,4.48409752679708E-16));
#45760=DIRECTION('',(0.,0.,-1.));
#45761=DIRECTION('',(1.55218636003651E-16,-1.,0.));
#45762=DIRECTION('',(0.,0.,-1.));
#45763=DIRECTION('center_axis',(0.,-1.,0.));
#45764=DIRECTION('ref_axis',(0.,0.,-1.));
#45765=DIRECTION('',(0.327110329510081,0.,-0.94498615456937));
#45766=DIRECTION('',(-1.,0.,0.));
#45767=DIRECTION('',(-0.327110329510081,0.,-0.94498615456937));
#45768=DIRECTION('',(-1.,0.,0.));
#45769=DIRECTION('',(0.,0.,-1.));
#45770=DIRECTION('center_axis',(0.,1.,0.));
#45771=DIRECTION('ref_axis',(0.,0.,1.));
#45772=DIRECTION('',(0.327110329510081,0.,-0.94498615456937));
#45773=DIRECTION('',(0.,0.,-1.));
#45774=DIRECTION('',(1.,0.,0.));
#45775=DIRECTION('',(-0.327110329510081,0.,-0.94498615456937));
#45776=DIRECTION('',(1.,0.,0.));
#45777=DIRECTION('center_axis',(0.,0.,-1.));
#45778=DIRECTION('ref_axis',(-1.,0.,0.));
#45779=DIRECTION('',(0.,1.,0.));
#45780=DIRECTION('',(0.,1.,0.));
#45781=DIRECTION('center_axis',(0.,-1.,0.));
#45782=DIRECTION('ref_axis',(0.,0.,-1.));
#45783=DIRECTION('',(-0.216439613938104,0.,-0.976296007119933));
#45784=DIRECTION('',(-1.,0.,0.));
#45785=DIRECTION('',(0.216439613938104,0.,-0.976296007119933));
#45786=DIRECTION('',(0.,0.,-1.));
#45787=DIRECTION('',(-1.,0.,0.));
#45788=DIRECTION('',(0.,0.,-1.));
#45789=DIRECTION('center_axis',(-1.,2.06958181338202E-16,0.));
#45790=DIRECTION('ref_axis',(-2.06958181338202E-16,-1.,0.));
#45791=DIRECTION('',(0.,0.,-1.));
#45792=DIRECTION('',(2.06958181338202E-16,1.,9.33528028464658E-16));
#45793=DIRECTION('',(2.06958181338202E-16,1.,0.));
#45794=DIRECTION('center_axis',(0.,1.,0.));
#45795=DIRECTION('ref_axis',(0.,0.,1.));
#45796=DIRECTION('',(-0.216439613938104,0.,-0.976296007119933));
#45797=DIRECTION('',(1.,0.,0.));
#45798=DIRECTION('',(0.,0.,-1.));
#45799=DIRECTION('',(0.216439613938104,0.,-0.976296007119933));
#45800=DIRECTION('',(1.,0.,0.));
#45801=DIRECTION('center_axis',(0.,0.,1.));
#45802=DIRECTION('ref_axis',(1.,0.,0.));
#45803=DIRECTION('',(0.,-1.,0.));
#45804=DIRECTION('',(0.,-1.,0.));
#45805=DIRECTION('center_axis',(1.,6.20874544014605E-16,0.));
#45806=DIRECTION('ref_axis',(-6.20874544014605E-16,1.,0.));
#45807=DIRECTION('',(6.20874544014605E-16,-1.,2.80058408539398E-15));
#45808=DIRECTION('',(0.,0.,-1.));
#45809=DIRECTION('',(6.20874544014605E-16,-1.,0.));
#45810=DIRECTION('',(0.,0.,-1.));
#45811=DIRECTION('center_axis',(0.,-1.,0.));
#45812=DIRECTION('ref_axis',(0.,0.,-1.));
#45813=DIRECTION('',(-1.,0.,0.));
#45814=DIRECTION('',(-0.216439613938103,0.,-0.976296007119933));
#45815=DIRECTION('',(-1.,0.,0.));
#45816=DIRECTION('',(0.,0.,-1.));
#45817=DIRECTION('',(0.216439613938103,0.,-0.976296007119933));
#45818=DIRECTION('center_axis',(0.,1.,0.));
#45819=DIRECTION('ref_axis',(0.,0.,1.));
#45820=DIRECTION('',(0.216439613938103,0.,0.976296007119933));
#45821=DIRECTION('',(1.,0.,0.));
#45822=DIRECTION('',(-0.216439613938103,0.,0.976296007119933));
#45823=DIRECTION('',(0.,0.,-1.));
#45824=DIRECTION('',(1.,0.,0.));
#45825=DIRECTION('center_axis',(0.,0.,-1.));
#45826=DIRECTION('ref_axis',(-1.,0.,0.));
#45827=DIRECTION('',(0.,1.,0.));
#45828=DIRECTION('',(0.,1.,0.));
#45829=DIRECTION('center_axis',(0.,0.,-1.));
#45830=DIRECTION('ref_axis',(-1.,0.,0.));
#45831=DIRECTION('center_axis',(0.,0.,-1.));
#45832=DIRECTION('ref_axis',(-1.,0.,0.));
#45833=DIRECTION('',(-1.,0.,0.));
#45834=DIRECTION('center_axis',(0.,0.,1.));
#45835=DIRECTION('ref_axis',(1.,0.,0.));
#45836=DIRECTION('',(-0.707106781186544,-0.707106781186551,0.));
#45837=DIRECTION('center_axis',(0.,0.,-1.));
#45838=DIRECTION('ref_axis',(-1.,0.,0.));
#45839=DIRECTION('',(0.,1.,0.));
#45840=DIRECTION('center_axis',(0.,0.,1.));
#45841=DIRECTION('ref_axis',(1.,0.,0.));
#45842=DIRECTION('',(1.,0.,0.));
#45843=DIRECTION('center_axis',(0.,0.,-1.));
#45844=DIRECTION('ref_axis',(-1.,0.,0.));
#45845=DIRECTION('',(0.,-1.,0.));
#45846=DIRECTION('center_axis',(0.,0.,1.));
#45847=DIRECTION('ref_axis',(1.,0.,0.));
#45848=DIRECTION('',(0.707106781186544,-0.707106781186551,0.));
#45849=DIRECTION('',(-2.06958181338202E-16,1.,0.));
#45850=DIRECTION('',(-6.20874544014605E-16,-1.,0.));
#45851=DIRECTION('',(0.,1.,0.));
#45852=DIRECTION('center_axis',(0.,0.,-1.));
#45853=DIRECTION('ref_axis',(-1.,0.,0.));
#45854=DIRECTION('',(0.,-1.,0.));
#45855=DIRECTION('center_axis',(0.,0.,1.));
#45856=DIRECTION('ref_axis',(-1.,0.,0.));
#45857=DIRECTION('',(1.,-1.52617206349959E-16,0.));
#45858=DIRECTION('center_axis',(0.,0.,1.));
#45859=DIRECTION('ref_axis',(-1.,0.,0.));
#45860=DIRECTION('',(0.,1.,0.));
#45861=DIRECTION('center_axis',(0.,0.,1.));
#45862=DIRECTION('ref_axis',(-1.,1.89711666226685E-15,0.));
#45863=DIRECTION('',(-1.,0.,0.));
#45864=DIRECTION('center_axis',(0.,0.,1.));
#45865=DIRECTION('ref_axis',(-1.,2.38494666113547E-14,0.));
#45866=DIRECTION('center_axis',(0.,0.,-1.));
#45867=DIRECTION('ref_axis',(-1.,0.,0.));
#45868=DIRECTION('',(0.707106781186544,-0.707106781186551,0.));
#45869=DIRECTION('center_axis',(0.,0.,1.));
#45870=DIRECTION('ref_axis',(1.,0.,0.));
#45871=DIRECTION('',(0.,-1.,0.));
#45872=DIRECTION('center_axis',(0.,0.,-1.));
#45873=DIRECTION('ref_axis',(-1.,0.,0.));
#45874=DIRECTION('',(1.,0.,0.));
#45875=DIRECTION('center_axis',(0.,0.,1.));
#45876=DIRECTION('ref_axis',(1.,0.,0.));
#45877=DIRECTION('',(0.,1.,0.));
#45878=DIRECTION('center_axis',(0.,0.,-1.));
#45879=DIRECTION('ref_axis',(-1.,0.,0.));
#45880=DIRECTION('',(-0.707106781186544,-0.707106781186551,0.));
#45881=DIRECTION('center_axis',(0.,0.,1.));
#45882=DIRECTION('ref_axis',(1.,0.,0.));
#45883=DIRECTION('',(-1.,0.,0.));
#45884=DIRECTION('center_axis',(0.,0.,-1.));
#45885=DIRECTION('ref_axis',(-1.,0.,0.));
#45886=DIRECTION('',(-0.826053778523829,-0.563591301375832,0.));
#45887=DIRECTION('center_axis',(0.,0.,-1.));
#45888=DIRECTION('ref_axis',(-1.,0.,0.));
#45889=DIRECTION('',(1.,0.,0.));
#45890=DIRECTION('center_axis',(0.,0.,1.));
#45891=DIRECTION('ref_axis',(1.,0.,0.));
#45892=DIRECTION('',(0.826053778523829,-0.563591301375832,0.));
#45893=DIRECTION('center_axis',(0.,0.,-1.));
#45894=DIRECTION('ref_axis',(-1.,0.,0.));
#45895=DIRECTION('',(-0.82605377852383,-0.563591301375832,0.));
#45896=DIRECTION('center_axis',(0.,0.,-1.));
#45897=DIRECTION('ref_axis',(-1.,0.,0.));
#45898=DIRECTION('',(-1.,1.52617206349959E-16,0.));
#45899=DIRECTION('center_axis',(0.,0.,-1.));
#45900=DIRECTION('ref_axis',(-1.,0.,0.));
#45901=DIRECTION('',(0.82605377852383,-0.563591301375832,0.));
#45902=DIRECTION('',(1.,0.,0.));
#45903=DIRECTION('center_axis',(0.,0.,-1.));
#45904=DIRECTION('ref_axis',(-1.,0.,0.));
#45905=DIRECTION('',(2.33197918015441E-16,-1.,0.));
#45906=DIRECTION('center_axis',(0.,0.,1.));
#45907=DIRECTION('ref_axis',(1.,0.,0.));
#45908=DIRECTION('',(0.707106781186544,-0.707106781186551,0.));
#45909=DIRECTION('center_axis',(0.,0.,-1.));
#45910=DIRECTION('ref_axis',(-1.,0.,0.));
#45911=DIRECTION('',(-1.,3.20838317005448E-16,0.));
#45912=DIRECTION('center_axis',(0.,0.,1.));
#45913=DIRECTION('ref_axis',(1.,0.,0.));
#45914=DIRECTION('',(-0.707106781186543,-0.707106781186552,0.));
#45915=DIRECTION('center_axis',(0.,0.,-1.));
#45916=DIRECTION('ref_axis',(-1.,0.,0.));
#45917=DIRECTION('',(-2.33197918015441E-16,1.,0.));
#45918=DIRECTION('center_axis',(0.,0.,1.));
#45919=DIRECTION('ref_axis',(1.,0.,0.));
#45920=DIRECTION('center_axis',(0.,0.,-1.));
#45921=DIRECTION('ref_axis',(-1.,0.,0.));
#45922=DIRECTION('',(0.,0.,-1.));
#45923=DIRECTION('center_axis',(0.,0.,-1.));
#45924=DIRECTION('ref_axis',(-1.,0.,0.));
#45925=DIRECTION('',(0.,0.,-1.));
#45926=DIRECTION('',(0.,0.,-1.));
#45927=DIRECTION('center_axis',(0.,0.,-1.));
#45928=DIRECTION('ref_axis',(-1.,0.,0.));
#45929=DIRECTION('center_axis',(1.,0.,0.));
#45930=DIRECTION('ref_axis',(0.,0.,-1.));
#45931=DIRECTION('',(0.,0.,-1.));
#45932=DIRECTION('',(0.,1.,0.));
#45933=DIRECTION('',(0.,-1.,0.));
#45934=DIRECTION('center_axis',(0.,0.,-1.));
#45935=DIRECTION('ref_axis',(-1.,0.,0.));
#45936=DIRECTION('',(0.,0.,-1.));
#45937=DIRECTION('center_axis',(0.,0.,-1.));
#45938=DIRECTION('ref_axis',(-1.,0.,0.));
#45939=DIRECTION('',(0.,0.,-1.));
#45940=DIRECTION('',(0.,0.,-1.));
#45941=DIRECTION('center_axis',(0.,0.,-1.));
#45942=DIRECTION('ref_axis',(-1.,0.,0.));
#45943=DIRECTION('center_axis',(-1.,0.,0.));
#45944=DIRECTION('ref_axis',(0.,0.,1.));
#45945=DIRECTION('',(0.,0.,-1.));
#45946=DIRECTION('',(0.,-1.,0.));
#45947=DIRECTION('',(0.,1.,0.));
#45948=DIRECTION('center_axis',(0.,0.,-1.));
#45949=DIRECTION('ref_axis',(-1.,0.,0.));
#45950=DIRECTION('',(0.,0.,-1.));
#45951=DIRECTION('center_axis',(0.,0.,-1.));
#45952=DIRECTION('ref_axis',(-1.,0.,0.));
#45953=DIRECTION('center_axis',(0.,0.,-1.));
#45954=DIRECTION('ref_axis',(-1.,0.,0.));
#45955=DIRECTION('',(0.,0.,-1.));
#45956=DIRECTION('center_axis',(0.,1.,0.));
#45957=DIRECTION('ref_axis',(0.,0.,1.));
#45958=DIRECTION('',(1.,0.,0.));
#45959=DIRECTION('center_axis',(0.,0.,-1.));
#45960=DIRECTION('ref_axis',(-1.,0.,0.));
#45961=DIRECTION('',(0.,0.,-1.));
#45962=DIRECTION('center_axis',(0.,0.,-1.));
#45963=DIRECTION('ref_axis',(-1.,0.,0.));
#45964=DIRECTION('center_axis',(0.,0.,-1.));
#45965=DIRECTION('ref_axis',(-1.,0.,0.));
#45966=DIRECTION('',(0.,0.,-1.));
#45967=DIRECTION('center_axis',(-1.52617206349959E-16,-1.,0.));
#45968=DIRECTION('ref_axis',(1.,-1.52617206349959E-16,0.));
#45969=DIRECTION('',(-1.,1.52617206349959E-16,0.));
#45970=DIRECTION('center_axis',(0.563591301375832,-0.82605377852383,0.));
#45971=DIRECTION('ref_axis',(0.82605377852383,0.563591301375832,0.));
#45972=DIRECTION('',(0.,0.,-1.));
#45973=DIRECTION('',(-0.82605377852383,-0.563591301375832,0.));
#45974=DIRECTION('center_axis',(0.,0.,-1.));
#45975=DIRECTION('ref_axis',(1.,-3.21624529935327E-16,0.));
#45976=DIRECTION('',(0.,0.,-1.));
#45977=DIRECTION('center_axis',(0.,0.,-1.));
#45978=DIRECTION('ref_axis',(-1.,0.,0.));
#45979=DIRECTION('center_axis',(0.563591301375832,0.826053778523829,0.));
#45980=DIRECTION('ref_axis',(-0.82605377852383,0.563591301375832,0.));
#45981=DIRECTION('',(0.826053778523829,-0.563591301375832,0.));
#45982=DIRECTION('center_axis',(0.,0.,-1.));
#45983=DIRECTION('ref_axis',(-1.,0.,0.));
#45984=DIRECTION('center_axis',(0.563591301375832,-0.826053778523829,0.));
#45985=DIRECTION('ref_axis',(0.82605377852383,0.563591301375832,0.));
#45986=DIRECTION('',(-0.826053778523829,-0.563591301375832,0.));
#45987=DIRECTION('center_axis',(0.563591301375832,0.82605377852383,0.));
#45988=DIRECTION('ref_axis',(-0.82605377852383,0.563591301375832,0.));
#45989=DIRECTION('',(0.82605377852383,-0.563591301375832,0.));
#45990=DIRECTION('center_axis',(0.,0.,-1.));
#45991=DIRECTION('ref_axis',(-1.,0.,0.));
#45992=DIRECTION('center_axis',(0.,0.,-1.));
#45993=DIRECTION('ref_axis',(-1.,0.,0.));
#45994=DIRECTION('center_axis',(-1.,0.,0.));
#45995=DIRECTION('ref_axis',(0.,0.,1.));
#45996=DIRECTION('center_axis',(-6.82961998416064E-15,-1.,-6.82961998416066E-15));
#45997=DIRECTION('ref_axis',(-3.33169350914619E-30,6.82961998416066E-15,
-1.));
#45998=DIRECTION('center_axis',(0.,1.,0.));
#45999=DIRECTION('ref_axis',(0.,0.,1.));
#46000=DIRECTION('center_axis',(0.,-1.,-6.82961998416066E-15));
#46001=DIRECTION('ref_axis',(0.,6.82961998416066E-15,-1.));
#46002=DIRECTION('center_axis',(-1.,0.,0.));
#46003=DIRECTION('ref_axis',(0.,0.,1.));
#46004=DIRECTION('center_axis',(-1.,6.82961998416066E-15,0.));
#46005=DIRECTION('ref_axis',(-6.82961998416066E-15,-1.,0.));
#46006=DIRECTION('center_axis',(0.,0.,-1.));
#46007=DIRECTION('ref_axis',(-1.,0.,0.));
#46008=DIRECTION('center_axis',(-1.,6.82961998416066E-15,-6.82961998416066E-15));
#46009=DIRECTION('ref_axis',(-6.82961998416066E-15,1.33267740365848E-29,
1.));
#46010=DIRECTION('center_axis',(0.,0.,-1.));
#46011=DIRECTION('ref_axis',(-1.,0.,0.));
#46012=DIRECTION('center_axis',(0.,-1.,0.));
#46013=DIRECTION('ref_axis',(0.,0.,-1.));
#46014=DIRECTION('center_axis',(1.,-1.52617206349959E-16,0.));
#46015=DIRECTION('ref_axis',(1.52617206349959E-16,1.,0.));
#46016=DIRECTION('center_axis',(-1.,0.,-6.82961998416066E-15));
#46017=DIRECTION('ref_axis',(-6.82961998416066E-15,0.,1.));
#46018=DIRECTION('center_axis',(0.,-1.,0.));
#46019=DIRECTION('ref_axis',(0.,0.,-1.));
#46020=DIRECTION('center_axis',(-6.82961998416064E-15,-1.,0.));
#46021=DIRECTION('ref_axis',(1.,-6.82961998416064E-15,0.));
#46022=DIRECTION('center_axis',(0.,0.,-1.));
#46023=DIRECTION('ref_axis',(-1.,0.,0.));
#46024=DIRECTION('center_axis',(0.,0.,1.));
#46025=DIRECTION('ref_axis',(1.,0.,0.));
#46026=DIRECTION('',(0.,0.,1.));
#46027=DIRECTION('',(0.,0.,1.));
#46028=DIRECTION('center_axis',(0.,-1.,0.));
#46029=DIRECTION('ref_axis',(0.,0.,-1.));
#46030=DIRECTION('',(0.,0.,1.));
#46031=DIRECTION('center_axis',(0.,0.,1.));
#46032=DIRECTION('ref_axis',(1.,0.,0.));
#46033=DIRECTION('',(0.,0.,1.));
#46034=DIRECTION('center_axis',(1.,2.33197918015441E-16,0.));
#46035=DIRECTION('ref_axis',(-2.33197918015441E-16,1.,0.));
#46036=DIRECTION('',(0.,0.,1.));
#46037=DIRECTION('center_axis',(0.,0.,1.));
#46038=DIRECTION('ref_axis',(1.,0.,0.));
#46039=DIRECTION('',(0.,0.,1.));
#46040=DIRECTION('center_axis',(-0.707106781186552,0.707106781186543,0.));
#46041=DIRECTION('ref_axis',(-0.707106781186543,-0.707106781186552,0.));
#46042=DIRECTION('',(0.,0.,1.));
#46043=DIRECTION('center_axis',(0.,0.,1.));
#46044=DIRECTION('ref_axis',(1.,0.,0.));
#46045=DIRECTION('',(0.,0.,1.));
#46046=DIRECTION('center_axis',(3.20838317005448E-16,1.,0.));
#46047=DIRECTION('ref_axis',(-1.,3.20838317005448E-16,0.));
#46048=DIRECTION('',(0.,0.,1.));
#46049=DIRECTION('center_axis',(0.,0.,1.));
#46050=DIRECTION('ref_axis',(1.,0.,0.));
#46051=DIRECTION('',(0.,0.,1.));
#46052=DIRECTION('center_axis',(-0.707106781186551,-0.707106781186544,0.));
#46053=DIRECTION('ref_axis',(0.707106781186544,-0.707106781186551,0.));
#46054=DIRECTION('',(0.,0.,1.));
#46055=DIRECTION('center_axis',(0.,0.,1.));
#46056=DIRECTION('ref_axis',(1.,0.,0.));
#46057=DIRECTION('',(0.,0.,1.));
#46058=DIRECTION('center_axis',(-1.,-2.33197918015441E-16,0.));
#46059=DIRECTION('ref_axis',(2.33197918015441E-16,-1.,0.));
#46060=DIRECTION('center_axis',(0.,0.,1.));
#46061=DIRECTION('ref_axis',(1.,0.,0.));
#46062=DIRECTION('',(0.,0.,1.));
#46063=DIRECTION('',(0.,0.,1.));
#46064=DIRECTION('center_axis',(-0.707106781186551,-0.707106781186544,0.));
#46065=DIRECTION('ref_axis',(0.707106781186544,-0.707106781186551,0.));
#46066=DIRECTION('',(0.,0.,1.));
#46067=DIRECTION('center_axis',(0.,0.,1.));
#46068=DIRECTION('ref_axis',(1.,0.,0.));
#46069=DIRECTION('',(0.,0.,1.));
#46070=DIRECTION('center_axis',(-1.,0.,0.));
#46071=DIRECTION('ref_axis',(0.,0.,1.));
#46072=DIRECTION('',(0.,0.,1.));
#46073=DIRECTION('center_axis',(0.,0.,1.));
#46074=DIRECTION('ref_axis',(1.,0.,0.));
#46075=DIRECTION('',(0.,0.,1.));
#46076=DIRECTION('center_axis',(0.,-1.,0.));
#46077=DIRECTION('ref_axis',(0.,0.,-1.));
#46078=DIRECTION('',(0.,0.,1.));
#46079=DIRECTION('center_axis',(0.,0.,1.));
#46080=DIRECTION('ref_axis',(1.,0.,0.));
#46081=DIRECTION('',(0.,0.,1.));
#46082=DIRECTION('center_axis',(1.,0.,0.));
#46083=DIRECTION('ref_axis',(0.,0.,-1.));
#46084=DIRECTION('',(0.,0.,1.));
#46085=DIRECTION('center_axis',(0.,0.,1.));
#46086=DIRECTION('ref_axis',(1.,0.,0.));
#46087=DIRECTION('',(0.,0.,1.));
#46088=DIRECTION('center_axis',(-0.707106781186551,0.707106781186544,0.));
#46089=DIRECTION('ref_axis',(-0.707106781186544,-0.707106781186551,0.));
#46090=DIRECTION('',(0.,0.,1.));
#46091=DIRECTION('center_axis',(0.,0.,1.));
#46092=DIRECTION('ref_axis',(1.,0.,0.));
#46093=DIRECTION('',(0.,0.,1.));
#46094=DIRECTION('center_axis',(0.,1.,0.));
#46095=DIRECTION('ref_axis',(0.,0.,1.));
#46096=DIRECTION('center_axis',(-1.,0.,0.));
#46097=DIRECTION('ref_axis',(0.,0.,1.));
#46098=DIRECTION('',(0.,-1.,0.));
#46099=DIRECTION('center_axis',(-1.,-2.06958181338202E-16,0.));
#46100=DIRECTION('ref_axis',(2.06958181338202E-16,-1.,0.));
#46101=DIRECTION('',(2.06958181338202E-16,-1.,-9.33528028464659E-16));
#46102=DIRECTION('center_axis',(1.,-6.20874544014605E-16,0.));
#46103=DIRECTION('ref_axis',(6.20874544014605E-16,1.,0.));
#46104=DIRECTION('',(6.20874544014605E-16,1.,-2.80058408539397E-15));
#46105=DIRECTION('center_axis',(-0.976296007119933,0.,-0.216439613938103));
#46106=DIRECTION('ref_axis',(-0.216439613938103,0.,0.976296007119933));
#46107=DIRECTION('center_axis',(-0.976296007119933,0.,0.216439613938103));
#46108=DIRECTION('ref_axis',(0.216439613938103,0.,0.976296007119933));
#46109=DIRECTION('center_axis',(-0.976296007119933,0.,-0.216439613938104));
#46110=DIRECTION('ref_axis',(-0.216439613938104,0.,0.976296007119933));
#46111=DIRECTION('center_axis',(-0.976296007119933,0.,0.216439613938104));
#46112=DIRECTION('ref_axis',(0.216439613938104,0.,0.976296007119933));
#46113=DIRECTION('center_axis',(-0.94498615456937,0.,0.327110329510081));
#46114=DIRECTION('ref_axis',(0.327110329510081,0.,0.944986154569371));
#46115=DIRECTION('center_axis',(-0.94498615456937,0.,-0.327110329510081));
#46116=DIRECTION('ref_axis',(-0.327110329510081,0.,0.944986154569371));
#46117=DIRECTION('center_axis',(0.,0.,1.));
#46118=DIRECTION('ref_axis',(1.,0.,0.));
#46119=DIRECTION('',(1.,0.,0.));
#46120=DIRECTION('',(6.96899998383741E-17,1.,0.));
#46121=DIRECTION('',(-1.,0.,0.));
#46122=DIRECTION('',(1.39379999676748E-16,-1.,0.));
#46123=DIRECTION('',(-1.,-6.72614310123308E-16,0.));
#46124=DIRECTION('',(-2.06958181338202E-16,-1.,0.));
#46125=DIRECTION('',(1.,0.,0.));
#46126=DIRECTION('',(1.29348863336376E-16,-1.,0.));
#46127=DIRECTION('center_axis',(0.,-1.,0.));
#46128=DIRECTION('ref_axis',(0.,0.,-1.));
#46129=DIRECTION('',(0.,0.,1.));
#46130=DIRECTION('',(0.,0.,1.));
#46131=DIRECTION('center_axis',(1.,-6.96899998383741E-17,0.));
#46132=DIRECTION('ref_axis',(6.96899998383741E-17,1.,0.));
#46133=DIRECTION('',(0.,0.,1.));
#46134=DIRECTION('center_axis',(0.,1.,0.));
#46135=DIRECTION('ref_axis',(0.,0.,1.));
#46136=DIRECTION('',(0.,0.,1.));
#46137=DIRECTION('center_axis',(-1.,-1.39379999676748E-16,0.));
#46138=DIRECTION('ref_axis',(1.39379999676748E-16,-1.,0.));
#46139=DIRECTION('center_axis',(0.,0.707106781186548,-0.707106781186547));
#46140=DIRECTION('ref_axis',(0.,0.707106781186547,0.707106781186548));
#46141=DIRECTION('',(1.46341533446278E-16,0.707106781186547,0.707106781186548));
#46142=DIRECTION('',(1.,6.72614310123308E-16,6.7261431012331E-16));
#46143=DIRECTION('',(-9.14634584039234E-17,0.707106781186547,0.707106781186548));
#46144=DIRECTION('',(-1.,0.,0.));
#46145=DIRECTION('center_axis',(0.,0.,1.));
#46146=DIRECTION('ref_axis',(1.,0.,0.));
#46147=DIRECTION('',(-1.29348863336376E-16,1.,0.));
#46148=DIRECTION('',(-1.,0.,0.));
#46149=DIRECTION('',(2.06958181338202E-16,1.,0.));
#46150=DIRECTION('center_axis',(0.,0.707106781186547,0.707106781186548));
#46151=DIRECTION('ref_axis',(0.,-0.707106781186548,0.707106781186547));
#46152=DIRECTION('',(-1.46341533446278E-16,-0.707106781186548,0.707106781186547));
#46153=DIRECTION('',(9.14634584039236E-17,-0.707106781186548,0.707106781186547));
#46154=DIRECTION('',(1.,0.,0.));
#46155=DIRECTION('center_axis',(0.,1.,0.));
#46156=DIRECTION('ref_axis',(0.,0.,1.));
#46157=DIRECTION('',(0.,0.,1.));
#46158=DIRECTION('',(0.,0.,1.));
#46159=DIRECTION('center_axis',(1.,1.29348863336376E-16,0.));
#46160=DIRECTION('ref_axis',(-1.29348863336376E-16,1.,0.));
#46161=DIRECTION('',(0.,0.,1.));
#46162=DIRECTION('center_axis',(6.72614310123308E-16,-1.,0.));
#46163=DIRECTION('ref_axis',(1.,6.72614310123308E-16,0.));
#46164=DIRECTION('',(0.,0.,1.));
#46165=DIRECTION('center_axis',(1.,-2.06958181338202E-16,0.));
#46166=DIRECTION('ref_axis',(2.06958181338202E-16,1.,0.));
#46167=DIRECTION('center_axis',(0.,-1.,0.));
#46168=DIRECTION('ref_axis',(0.,0.,-1.));
#46169=DIRECTION('',(0.,0.,1.));
#46170=DIRECTION('',(1.,0.,0.));
#46171=DIRECTION('',(0.,0.,1.));
#46172=DIRECTION('center_axis',(1.,-2.78759999353496E-16,0.));
#46173=DIRECTION('ref_axis',(2.78759999353496E-16,1.,0.));
#46174=DIRECTION('',(0.,0.,1.));
#46175=DIRECTION('',(2.78759999353496E-16,1.,0.));
#46176=DIRECTION('center_axis',(-6.44303772090628E-16,1.,0.));
#46177=DIRECTION('ref_axis',(-1.,-6.44303772090628E-16,0.));
#46178=DIRECTION('',(0.,0.,1.));
#46179=DIRECTION('',(-1.,-6.44303772090628E-16,0.));
#46180=DIRECTION('center_axis',(-1.,2.78759999353496E-16,0.));
#46181=DIRECTION('ref_axis',(-2.78759999353496E-16,-1.,0.));
#46182=DIRECTION('',(-2.78759999353496E-16,-1.,0.));
#46183=DIRECTION('center_axis',(0.,0.,-1.));
#46184=DIRECTION('ref_axis',(-1.,0.,0.));
#46185=DIRECTION('',(0.,-1.,0.));
#46186=DIRECTION('',(-1.,0.,0.));
#46187=DIRECTION('',(0.,-1.,0.));
#46188=DIRECTION('',(1.,0.,0.));
#46189=DIRECTION('center_axis',(0.,0.,1.));
#46190=DIRECTION('ref_axis',(1.,0.,0.));
#46191=DIRECTION('',(0.,-1.,0.));
#46192=DIRECTION('',(-1.,0.,0.));
#46193=DIRECTION('',(0.,-1.,0.));
#46194=DIRECTION('',(-1.,0.,0.));
#46195=DIRECTION('center_axis',(0.,0.707106781186547,-0.707106781186548));
#46196=DIRECTION('ref_axis',(0.,0.707106781186548,0.707106781186547));
#46197=DIRECTION('',(0.,0.707106781186548,0.707106781186547));
#46198=DIRECTION('',(0.,-0.707106781186548,-0.707106781186547));
#46199=DIRECTION('',(-1.,0.,0.));
#46200=DIRECTION('center_axis',(0.,0.707106781186548,0.707106781186547));
#46201=DIRECTION('ref_axis',(0.,-0.707106781186547,0.707106781186548));
#46202=DIRECTION('',(-1.,0.,0.));
#46203=DIRECTION('',(0.,0.707106781186547,-0.707106781186548));
#46204=DIRECTION('',(0.,-0.707106781186547,0.707106781186548));
#46205=DIRECTION('center_axis',(0.,-1.,0.));
#46206=DIRECTION('ref_axis',(0.,0.,-1.));
#46207=DIRECTION('',(0.,0.,1.));
#46208=DIRECTION('',(0.,0.,1.));
#46209=DIRECTION('center_axis',(0.,1.,0.));
#46210=DIRECTION('ref_axis',(0.,0.,1.));
#46211=DIRECTION('',(0.,0.,1.));
#46212=DIRECTION('',(0.,0.,1.));
#46213=DIRECTION('center_axis',(-1.,0.,0.));
#46214=DIRECTION('ref_axis',(0.,0.,1.));
#46215=DIRECTION('center_axis',(-1.,0.,0.));
#46216=DIRECTION('ref_axis',(0.,0.,1.));
#46217=DIRECTION('center_axis',(0.,0.,1.));
#46218=DIRECTION('ref_axis',(1.,0.,0.));
#46219=DIRECTION('',(-1.39379999676748E-16,1.,0.));
#46220=DIRECTION('',(-1.,0.,0.));
#46221=DIRECTION('',(5.57519998706993E-16,-1.,0.));
#46222=DIRECTION('',(1.,6.44303772090628E-16,0.));
#46223=DIRECTION('',(0.,-1.,0.));
#46224=DIRECTION('',(-1.,0.,0.));
#46225=DIRECTION('',(0.,-1.,0.));
#46226=DIRECTION('',(1.,0.,0.));
#46227=DIRECTION('center_axis',(1.,1.39379999676748E-16,0.));
#46228=DIRECTION('ref_axis',(-1.39379999676748E-16,1.,0.));
#46229=DIRECTION('',(0.,0.,1.));
#46230=DIRECTION('',(0.,0.,1.));
#46231=DIRECTION('center_axis',(0.,1.,0.));
#46232=DIRECTION('ref_axis',(0.,0.,1.));
#46233=DIRECTION('',(0.,0.,1.));
#46234=DIRECTION('center_axis',(-1.,-5.57519998706993E-16,0.));
#46235=DIRECTION('ref_axis',(5.57519998706993E-16,-1.,0.));
#46236=DIRECTION('',(0.,0.,1.));
#46237=DIRECTION('center_axis',(6.44303772090628E-16,-1.,0.));
#46238=DIRECTION('ref_axis',(1.,6.44303772090628E-16,0.));
#46239=DIRECTION('center_axis',(0.,0.,-1.));
#46240=DIRECTION('ref_axis',(-1.,0.,0.));
#46241=DIRECTION('',(1.,0.,0.));
#46242=DIRECTION('',(0.,1.,0.));
#46243=DIRECTION('',(1.,0.,0.));
#46244=DIRECTION('',(0.,1.,0.));
#46245=DIRECTION('center_axis',(0.,0.707106781186547,-0.707106781186548));
#46246=DIRECTION('ref_axis',(0.,0.707106781186548,0.707106781186547));
#46247=DIRECTION('',(1.,0.,0.));
#46248=DIRECTION('',(0.,0.707106781186548,0.707106781186547));
#46249=DIRECTION('',(0.,0.707106781186548,0.707106781186547));
#46250=DIRECTION('center_axis',(0.,0.707106781186548,0.707106781186547));
#46251=DIRECTION('ref_axis',(0.,-0.707106781186547,0.707106781186548));
#46252=DIRECTION('',(0.,-0.707106781186547,0.707106781186548));
#46253=DIRECTION('',(1.,0.,0.));
#46254=DIRECTION('',(0.,-0.707106781186547,0.707106781186548));
#46255=DIRECTION('center_axis',(0.,1.,0.));
#46256=DIRECTION('ref_axis',(0.,0.,1.));
#46257=DIRECTION('',(0.,0.,1.));
#46258=DIRECTION('',(0.,0.,1.));
#46259=DIRECTION('center_axis',(0.,-1.,0.));
#46260=DIRECTION('ref_axis',(0.,0.,-1.));
#46261=DIRECTION('',(0.,0.,1.));
#46262=DIRECTION('',(0.,0.,1.));
#46263=DIRECTION('center_axis',(1.,0.,0.));
#46264=DIRECTION('ref_axis',(0.,0.,-1.));
#46265=DIRECTION('center_axis',(1.,0.,0.));
#46266=DIRECTION('ref_axis',(0.,0.,-1.));
#46267=DIRECTION('axis',(0.,0.,1.));
#46268=DIRECTION('refdir',(1.,0.,0.));
#46269=DIRECTION('center_axis',(0.,0.,1.));
#46270=DIRECTION('ref_axis',(1.,0.,0.));
#46271=DIRECTION('',(0.,-1.,0.));
#46272=DIRECTION('',(-1.,0.,0.));
#46273=DIRECTION('',(0.,1.,0.));
#46274=DIRECTION('',(1.,0.,0.));
#46275=DIRECTION('center_axis',(0.,0.,-1.));
#46276=DIRECTION('ref_axis',(-1.,0.,0.));
#46277=DIRECTION('',(1.,-6.42490176287706E-17,0.));
#46278=DIRECTION('',(0.,1.,0.));
#46279=DIRECTION('',(-1.,0.,0.));
#46280=DIRECTION('',(0.,-1.,0.));
#46281=DIRECTION('center_axis',(-6.42490176287706E-17,-1.,0.));
#46282=DIRECTION('ref_axis',(1.,-6.42490176287706E-17,0.));
#46283=DIRECTION('',(0.,0.,1.));
#46284=DIRECTION('',(0.,0.,1.));
#46285=DIRECTION('center_axis',(-1.,0.,0.));
#46286=DIRECTION('ref_axis',(0.,0.,1.));
#46287=DIRECTION('',(0.,0.,1.));
#46288=DIRECTION('center_axis',(0.,1.,0.));
#46289=DIRECTION('ref_axis',(0.,0.,1.));
#46290=DIRECTION('',(0.,0.,1.));
#46291=DIRECTION('center_axis',(1.,0.,0.));
#46292=DIRECTION('ref_axis',(0.,0.,-1.));
#46293=DIRECTION('center_axis',(1.,-3.61400724161835E-16,0.));
#46294=DIRECTION('ref_axis',(3.61400724161835E-16,1.,0.));
#46295=DIRECTION('center_axis',(1.,-4.33680868994202E-17,0.));
#46296=DIRECTION('ref_axis',(4.33680868994202E-17,1.,0.));
#46297=DIRECTION('',(1.,-3.61400724161835E-16,0.));
#46298=DIRECTION('center_axis',(1.,-3.61400724161835E-16,0.));
#46299=DIRECTION('ref_axis',(3.61400724161835E-16,1.,0.));
#46300=DIRECTION('center_axis',(1.,-3.61400724161835E-16,0.));
#46301=DIRECTION('ref_axis',(3.61400724161835E-16,1.,0.));
#46302=DIRECTION('center_axis',(1.,0.,0.));
#46303=DIRECTION('ref_axis',(0.,0.,-1.));
#46304=DIRECTION('',(1.,-3.61400724161835E-16,0.));
#46305=DIRECTION('center_axis',(1.,-3.46944695195361E-16,0.));
#46306=DIRECTION('ref_axis',(3.46944695195361E-16,1.,0.));
#46307=DIRECTION('center_axis',(0.,-1.,0.));
#46308=DIRECTION('ref_axis',(0.,0.,-1.));
#46309=DIRECTION('center_axis',(0.,-1.,0.));
#46310=DIRECTION('ref_axis',(0.,0.,-1.));
#46311=DIRECTION('',(0.,-1.,0.));
#46312=DIRECTION('center_axis',(0.,-1.,0.));
#46313=DIRECTION('ref_axis',(0.,0.,-1.));
#46314=DIRECTION('',(0.,1.,0.));
#46315=DIRECTION('center_axis',(0.,1.,0.));
#46316=DIRECTION('ref_axis',(0.,0.,1.));
#46317=DIRECTION('',(0.,0.,1.));
#46318=DIRECTION('',(-1.,0.,0.));
#46319=DIRECTION('',(0.,0.,1.));
#46320=DIRECTION('',(-1.,0.,0.));
#46321=DIRECTION('center_axis',(0.,1.,0.));
#46322=DIRECTION('ref_axis',(0.,0.,1.));
#46323=DIRECTION('',(-1.,0.,0.));
#46324=DIRECTION('',(0.,0.,1.));
#46325=DIRECTION('',(-1.,0.,0.));
#46326=DIRECTION('',(0.,0.,1.));
#46327=DIRECTION('center_axis',(0.,1.,0.));
#46328=DIRECTION('ref_axis',(0.,0.,1.));
#46329=DIRECTION('',(0.,0.,1.));
#46330=DIRECTION('',(-1.,0.,0.));
#46331=DIRECTION('',(4.33680868994201E-16,0.,1.));
#46332=DIRECTION('',(0.,0.,1.));
#46333=DIRECTION('',(-1.,0.,0.));
#46334=DIRECTION('center_axis',(0.,1.,0.));
#46335=DIRECTION('ref_axis',(0.,0.,1.));
#46336=DIRECTION('',(0.,0.,1.));
#46337=DIRECTION('',(-1.,0.,0.));
#46338=DIRECTION('',(0.,0.,1.));
#46339=DIRECTION('',(4.33680868994201E-16,0.,1.));
#46340=DIRECTION('',(-1.,0.,0.));
#46341=DIRECTION('center_axis',(0.,1.,0.));
#46342=DIRECTION('ref_axis',(0.,0.,1.));
#46343=DIRECTION('',(-1.,0.,0.));
#46344=DIRECTION('',(0.,0.,1.));
#46345=DIRECTION('',(-1.,0.,0.));
#46346=DIRECTION('',(0.,0.,1.));
#46347=DIRECTION('center_axis',(0.,1.,0.));
#46348=DIRECTION('ref_axis',(0.,0.,1.));
#46349=DIRECTION('',(0.,0.,1.));
#46350=DIRECTION('',(-1.,0.,0.));
#46351=DIRECTION('',(0.,0.,1.));
#46352=DIRECTION('',(-1.,0.,0.));
#46353=DIRECTION('center_axis',(0.,1.,0.));
#46354=DIRECTION('ref_axis',(0.,0.,1.));
#46355=DIRECTION('',(0.,0.,1.));
#46356=DIRECTION('',(-1.,0.,0.));
#46357=DIRECTION('',(0.,0.,1.));
#46358=DIRECTION('',(0.,0.,1.));
#46359=DIRECTION('',(-1.,0.,0.));
#46360=DIRECTION('center_axis',(0.,1.,0.));
#46361=DIRECTION('ref_axis',(0.,0.,1.));
#46362=DIRECTION('',(0.,0.,1.));
#46363=DIRECTION('',(-1.,0.,0.));
#46364=DIRECTION('',(0.,0.,1.));
#46365=DIRECTION('',(0.,0.,1.));
#46366=DIRECTION('',(-1.,0.,0.));
#46367=DIRECTION('center_axis',(0.,0.,-1.));
#46368=DIRECTION('ref_axis',(-1.,0.,0.));
#46369=DIRECTION('',(-1.,6.08674903851511E-17,0.));
#46370=DIRECTION('',(0.,1.,0.));
#46371=DIRECTION('',(1.,0.,0.));
#46372=DIRECTION('',(0.,-1.,0.));
#46373=DIRECTION('',(0.,1.,0.));
#46374=DIRECTION('',(-1.,0.,0.));
#46375=DIRECTION('',(0.,1.,0.));
#46376=DIRECTION('',(-1.,0.,0.));
#46377=DIRECTION('',(0.,1.,0.));
#46378=DIRECTION('',(-1.,0.,0.));
#46379=DIRECTION('',(0.,1.,0.));
#46380=DIRECTION('',(-1.,0.,0.));
#46381=DIRECTION('center_axis',(0.,0.,1.));
#46382=DIRECTION('ref_axis',(1.,0.,0.));
#46383=DIRECTION('',(1.,5.9818050895752E-17,0.));
#46384=DIRECTION('',(8.46206573647223E-17,1.,0.));
#46385=DIRECTION('',(1.,0.,0.));
#46386=DIRECTION('',(0.,1.,0.));
#46387=DIRECTION('',(6.19544098563145E-17,-1.,0.));
#46388=DIRECTION('',(1.,4.33680868994203E-15,0.));
#46389=DIRECTION('',(1.,0.,0.));
#46390=DIRECTION('',(1.,0.,0.));
#46391=DIRECTION('',(-1.,4.33680868994203E-15,0.));
#46392=DIRECTION('',(-6.19544098563145E-17,-1.,0.));
#46393=DIRECTION('',(-1.,4.33680868994203E-15,0.));
#46394=DIRECTION('',(-1.,6.08674903851511E-17,0.));
#46395=DIRECTION('',(-1.,6.08674903851511E-17,0.));
#46396=DIRECTION('',(1.,4.33680868994203E-15,0.));
#46397=DIRECTION('center_axis',(0.,1.,0.));
#46398=DIRECTION('ref_axis',(0.,0.,1.));
#46399=DIRECTION('',(0.,0.,-1.));
#46400=DIRECTION('',(1.,0.,0.));
#46401=DIRECTION('',(0.,0.,-1.));
#46402=DIRECTION('center_axis',(-1.,8.46206573647223E-17,0.));
#46403=DIRECTION('ref_axis',(-8.46206573647223E-17,-1.,0.));
#46404=DIRECTION('',(0.,0.,-1.));
#46405=DIRECTION('',(8.46206573647223E-17,1.,0.));
#46406=DIRECTION('center_axis',(-5.9818050895752E-17,1.,0.));
#46407=DIRECTION('ref_axis',(-1.,-5.9818050895752E-17,0.));
#46408=DIRECTION('',(0.,0.,-1.));
#46409=DIRECTION('',(1.,5.9818050895752E-17,0.));
#46410=DIRECTION('center_axis',(-1.,0.,0.));
#46411=DIRECTION('ref_axis',(0.,0.,1.));
#46412=DIRECTION('',(0.,1.,0.));
#46413=DIRECTION('center_axis',(0.,0.,1.));
#46414=DIRECTION('ref_axis',(1.,0.,0.));
#46415=DIRECTION('',(0.,1.,0.));
#46416=DIRECTION('',(1.,-6.42490176287706E-17,0.));
#46417=DIRECTION('',(0.,-1.,0.));
#46418=DIRECTION('',(-1.,0.,0.));
#46419=DIRECTION('center_axis',(6.08674903851511E-17,1.,0.));
#46420=DIRECTION('ref_axis',(-1.,6.08674903851511E-17,0.));
#46421=DIRECTION('center_axis',(-6.08674903851511E-17,-1.,0.));
#46422=DIRECTION('ref_axis',(-1.,6.08674903851511E-17,0.));
#46423=DIRECTION('center_axis',(-6.08674903851511E-17,-1.,0.));
#46424=DIRECTION('ref_axis',(-1.,6.08674903851511E-17,0.));
#46425=DIRECTION('',(2.31296463463574E-16,-1.40784352659886E-32,-1.));
#46426=DIRECTION('',(-0.0817503058163819,2.70504095639686E-16,0.99665284201618));
#46427=DIRECTION('',(0.427528579403957,-1.41465197685674E-15,0.904001832848161));
#46428=DIRECTION('',(-0.427528579403968,0.,-0.904001832848156));
#46429=DIRECTION('',(0.0817503058163822,0.,-0.99665284201618));
#46430=DIRECTION('',(0.,0.,1.));
#46431=DIRECTION('',(0.,0.,1.));
#46432=DIRECTION('',(-0.0817503058163822,0.,-0.99665284201618));
#46433=DIRECTION('',(0.427528579403968,0.,-0.904001832848156));
#46434=DIRECTION('',(-0.427528579403957,-1.41465197685674E-15,0.904001832848161));
#46435=DIRECTION('',(0.0817503058163819,2.70504095639686E-16,0.99665284201618));
#46436=DIRECTION('',(-2.31296463463574E-16,1.40784352659886E-32,1.));
#46437=DIRECTION('center_axis',(1.,0.,0.));
#46438=DIRECTION('ref_axis',(0.,0.,-1.));
#46439=DIRECTION('',(-6.19544098563145E-17,-1.,0.));
#46440=DIRECTION('',(0.,0.,1.));
#46441=DIRECTION('center_axis',(0.,-1.,0.));
#46442=DIRECTION('ref_axis',(0.,0.,-1.));
#46443=DIRECTION('center_axis',(0.,1.,0.));
#46444=DIRECTION('ref_axis',(0.,0.,-1.));
#46445=DIRECTION('center_axis',(0.,1.,0.));
#46446=DIRECTION('ref_axis',(0.,0.,-1.));
#46447=DIRECTION('',(2.31296463463574E-16,0.,-1.));
#46448=DIRECTION('',(0.0817503058163819,2.70504095639686E-16,0.99665284201618));
#46449=DIRECTION('',(-0.427528579403957,-1.41465197685674E-15,0.904001832848161));
#46450=DIRECTION('',(0.427528579403968,0.,-0.904001832848156));
#46451=DIRECTION('',(-0.0817503058163822,0.,-0.99665284201618));
#46452=DIRECTION('',(0.,0.,1.));
#46453=DIRECTION('',(0.0817503058163822,0.,-0.99665284201618));
#46454=DIRECTION('',(-0.427528579403968,0.,-0.904001832848156));
#46455=DIRECTION('',(0.427528579403957,-1.41465197685674E-15,0.904001832848161));
#46456=DIRECTION('',(-0.0817503058163819,2.70504095639686E-16,0.99665284201618));
#46457=DIRECTION('',(-2.31296463463574E-16,0.,1.));
#46458=DIRECTION('center_axis',(-1.,0.,0.));
#46459=DIRECTION('ref_axis',(0.,0.,1.));
#46460=DIRECTION('',(0.,-1.,0.));
#46461=DIRECTION('center_axis',(1.,0.,0.));
#46462=DIRECTION('ref_axis',(0.,0.,-1.));
#46463=DIRECTION('',(0.,1.,0.));
#46464=DIRECTION('center_axis',(0.,1.,0.));
#46465=DIRECTION('ref_axis',(0.,0.,1.));
#46466=DIRECTION('',(-1.,0.,0.));
#46467=DIRECTION('',(0.,0.,1.));
#46468=DIRECTION('center_axis',(0.,1.,0.));
#46469=DIRECTION('ref_axis',(0.,0.,1.));
#46470=DIRECTION('',(-1.,0.,0.));
#46471=DIRECTION('',(0.,0.,1.));
#46472=DIRECTION('center_axis',(0.,0.,1.));
#46473=DIRECTION('ref_axis',(1.,0.,0.));
#46474=DIRECTION('',(3.61400724161835E-16,1.,0.));
#46475=DIRECTION('',(1.,-3.61400724161835E-16,0.));
#46476=DIRECTION('',(4.33680868994202E-17,1.,0.));
#46477=DIRECTION('',(0.,1.,0.));
#46478=DIRECTION('',(4.33680868994202E-17,1.,0.));
#46479=DIRECTION('',(1.,-3.61400724161835E-16,0.));
#46480=DIRECTION('',(3.61400724161835E-16,1.,0.));
#46481=DIRECTION('center_axis',(1.,0.,0.));
#46482=DIRECTION('ref_axis',(0.,0.,-1.));
#46483=DIRECTION('center_axis',(1.,0.,0.));
#46484=DIRECTION('ref_axis',(0.,0.,-1.));
#46485=DIRECTION('',(0.,1.,0.));
#46486=DIRECTION('center_axis',(0.,1.,0.));
#46487=DIRECTION('ref_axis',(0.,0.,1.));
#46488=DIRECTION('',(-1.,0.,0.));
#46489=DIRECTION('',(0.,0.,1.));
#46490=DIRECTION('center_axis',(0.,1.,0.));
#46491=DIRECTION('ref_axis',(0.,0.,1.));
#46492=DIRECTION('',(-1.,0.,0.));
#46493=DIRECTION('',(0.,0.,1.));
#46494=DIRECTION('center_axis',(0.,0.,1.));
#46495=DIRECTION('ref_axis',(1.,0.,0.));
#46496=DIRECTION('',(3.46944695195361E-16,1.,0.));
#46497=DIRECTION('',(1.,-3.61400724161835E-16,0.));
#46498=DIRECTION('',(0.,1.,0.));
#46499=DIRECTION('',(0.,1.,0.));
#46500=DIRECTION('',(0.,1.,0.));
#46501=DIRECTION('',(1.,-3.61400724161835E-16,0.));
#46502=DIRECTION('',(3.46944695195361E-16,1.,0.));
#46503=DIRECTION('center_axis',(1.,0.,0.));
#46504=DIRECTION('ref_axis',(0.,0.,-1.));
#46505=DIRECTION('center_axis',(1.,-3.61400724161835E-16,0.));
#46506=DIRECTION('ref_axis',(3.61400724161835E-16,1.,0.));
#46507=DIRECTION('center_axis',(1.,-3.61400724161835E-16,0.));
#46508=DIRECTION('ref_axis',(-3.61400724161835E-16,-1.,0.));
#46509=DIRECTION('',(-1.61623317268703E-16,-0.44721359549996,0.894427190999915));
#46510=DIRECTION('',(3.61400724161835E-16,1.,0.));
#46511=DIRECTION('',(-1.61623317268703E-16,-0.447213595499958,-0.894427190999916));
#46512=DIRECTION('center_axis',(1.,-4.33680868994202E-17,0.));
#46513=DIRECTION('ref_axis',(4.33680868994202E-17,1.,0.));
#46514=DIRECTION('center_axis',(1.,-4.33680868994202E-17,0.));
#46515=DIRECTION('ref_axis',(4.33680868994202E-17,1.,0.));
#46516=DIRECTION('',(-1.93947980722443E-17,-0.447213595499958,-0.894427190999916));
#46517=DIRECTION('',(4.33680868994202E-17,1.,0.));
#46518=DIRECTION('',(-1.93947980722444E-17,-0.44721359549996,0.894427190999915));
#46519=DIRECTION('center_axis',(0.,0.,-1.));
#46520=DIRECTION('ref_axis',(-1.,0.,0.));
#46521=DIRECTION('',(-1.,0.,0.));
#46522=DIRECTION('',(-1.,0.,0.));
#46523=DIRECTION('center_axis',(1.,-3.46944695195361E-16,0.));
#46524=DIRECTION('ref_axis',(3.46944695195361E-16,1.,0.));
#46525=DIRECTION('center_axis',(1.,-3.46944695195361E-16,0.));
#46526=DIRECTION('ref_axis',(3.46944695195361E-16,1.,0.));
#46527=DIRECTION('',(-1.55158384577955E-16,-0.44721359549996,0.894427190999915));
#46528=DIRECTION('',(3.46944695195361E-16,1.,0.));
#46529=DIRECTION('',(-1.55158384577955E-16,-0.447213595499958,-0.894427190999916));
#46530=DIRECTION('center_axis',(1.,0.,0.));
#46531=DIRECTION('ref_axis',(0.,0.,-1.));
#46532=DIRECTION('center_axis',(1.,0.,0.));
#46533=DIRECTION('ref_axis',(0.,0.,-1.));
#46534=DIRECTION('',(0.,0.447213595499958,0.894427190999916));
#46535=DIRECTION('',(0.,1.,0.));
#46536=DIRECTION('',(0.,0.44721359549996,-0.894427190999915));
#46537=DIRECTION('center_axis',(0.,0.,-1.));
#46538=DIRECTION('ref_axis',(-1.,0.,0.));
#46539=DIRECTION('',(-1.,0.,0.));
#46540=DIRECTION('',(1.,0.,0.));
#46541=DIRECTION('center_axis',(0.,0.894427190999915,0.44721359549996));
#46542=DIRECTION('ref_axis',(0.,-0.44721359549996,0.894427190999915));
#46543=DIRECTION('center_axis',(0.,-0.894427190999916,0.447213595499958));
#46544=DIRECTION('ref_axis',(0.,-0.447213595499958,-0.894427190999916));
#46545=DIRECTION('center_axis',(0.,0.894427190999915,0.44721359549996));
#46546=DIRECTION('ref_axis',(0.,-0.44721359549996,0.894427190999915));
#46547=DIRECTION('center_axis',(0.,-0.894427190999916,0.447213595499958));
#46548=DIRECTION('ref_axis',(0.,-0.447213595499958,-0.894427190999916));
#46549=DIRECTION('center_axis',(1.,-3.61400724161835E-16,0.));
#46550=DIRECTION('ref_axis',(3.61400724161835E-16,1.,0.));
#46551=DIRECTION('center_axis',(1.,-3.61400724161835E-16,0.));
#46552=DIRECTION('ref_axis',(3.61400724161835E-16,1.,0.));
#46553=DIRECTION('center_axis',(-1.,6.19544098563145E-17,-2.31296463463574E-16));
#46554=DIRECTION('ref_axis',(-2.31296463463574E-16,0.,1.));
#46555=DIRECTION('',(-6.19544098563145E-17,-1.,0.));
#46556=DIRECTION('',(-6.19544098563145E-17,-1.,0.));
#46557=DIRECTION('center_axis',(1.,-6.19544098563145E-17,2.31296463463574E-16));
#46558=DIRECTION('ref_axis',(2.31296463463574E-16,0.,-1.));
#46559=DIRECTION('',(-6.19544098563145E-17,-1.,0.));
#46560=DIRECTION('',(-6.19544098563145E-17,-1.,0.));
#46561=DIRECTION('center_axis',(0.904001832848161,-5.60069000631345E-17,
-0.427528579403957));
#46562=DIRECTION('ref_axis',(-0.427528579403957,3.71975701883526E-34,-0.904001832848161));
#46563=DIRECTION('',(-6.19544098563145E-17,-1.,0.));
#46564=DIRECTION('center_axis',(0.99665284201618,-6.17470386587311E-17,
0.0817503058163819));
#46565=DIRECTION('ref_axis',(0.0817503058163819,8.42971361630042E-34,-0.99665284201618));
#46566=DIRECTION('center_axis',(-0.99665284201618,6.17470386587311E-17,
-0.0817503058163822));
#46567=DIRECTION('ref_axis',(-0.0817503058163822,-1.07140226946576E-35,
0.99665284201618));
#46568=DIRECTION('',(-6.19544098563145E-17,-1.,0.));
#46569=DIRECTION('center_axis',(-0.904001832848156,5.60069000631342E-17,
0.427528579403968));
#46570=DIRECTION('ref_axis',(0.427528579403968,-1.6530393860932E-34,0.904001832848156));
#46571=DIRECTION('center_axis',(-0.904001832848156,-5.60069000631342E-17,
-0.427528579403968));
#46572=DIRECTION('ref_axis',(-0.427528579403968,-1.6530393860932E-34,0.904001832848156));
#46573=DIRECTION('',(6.19544098563145E-17,-1.,0.));
#46574=DIRECTION('center_axis',(-0.99665284201618,-6.17470386587311E-17,
0.0817503058163822));
#46575=DIRECTION('ref_axis',(0.0817503058163822,-1.07140226946576E-35,0.99665284201618));
#46576=DIRECTION('center_axis',(0.99665284201618,6.17470386587311E-17,-0.0817503058163819));
#46577=DIRECTION('ref_axis',(-0.0817503058163819,8.42971361630042E-34,-0.99665284201618));
#46578=DIRECTION('',(6.19544098563145E-17,-1.,0.));
#46579=DIRECTION('center_axis',(0.904001832848161,5.60069000631345E-17,
0.427528579403957));
#46580=DIRECTION('ref_axis',(0.427528579403957,3.71975701883526E-34,-0.904001832848161));
#46581=DIRECTION('center_axis',(1.,0.,0.));
#46582=DIRECTION('ref_axis',(0.,0.,-1.));
#46583=DIRECTION('',(0.,0.,-1.));
#46584=DIRECTION('',(0.,0.,-1.));
#46585=DIRECTION('center_axis',(0.,1.,0.));
#46586=DIRECTION('ref_axis',(0.,0.,1.));
#46587=DIRECTION('',(0.,0.,-1.));
#46588=DIRECTION('center_axis',(-1.,0.,0.));
#46589=DIRECTION('ref_axis',(0.,0.,1.));
#46590=DIRECTION('',(0.,0.,-1.));
#46591=DIRECTION('center_axis',(0.,-1.,0.));
#46592=DIRECTION('ref_axis',(0.,0.,-1.));
#46593=DIRECTION('center_axis',(0.,1.,0.));
#46594=DIRECTION('ref_axis',(1.,0.,0.));
#46595=DIRECTION('center_axis',(0.,0.,1.));
#46596=DIRECTION('ref_axis',(-1.,0.,0.));
#46597=DIRECTION('center_axis',(0.,-1.,0.));
#46598=DIRECTION('ref_axis',(1.,0.,4.44089209850063E-16));
#46599=DIRECTION('center_axis',(5.55111512312578E-16,0.,-1.));
#46600=DIRECTION('ref_axis',(-1.,0.,-5.55111512312578E-16));
#46601=DIRECTION('axis',(0.,0.,1.));
#46602=DIRECTION('refdir',(1.,0.,0.));
#46603=DIRECTION('center_axis',(0.,1.,0.));
#46604=DIRECTION('ref_axis',(1.,0.,0.));
#46605=DIRECTION('center_axis',(0.,1.,0.));
#46606=DIRECTION('ref_axis',(-1.,0.,0.));
#46607=DIRECTION('center_axis',(-1.48029736616688E-16,0.,-1.));
#46608=DIRECTION('ref_axis',(-1.,0.,1.48029736616688E-16));
#46609=DIRECTION('center_axis',(0.,1.,0.));
#46610=DIRECTION('ref_axis',(1.,0.,0.));
#46611=DIRECTION('center_axis',(0.,1.,0.));
#46612=DIRECTION('ref_axis',(1.,0.,0.));
#46613=DIRECTION('center_axis',(0.,1.,0.));
#46614=DIRECTION('ref_axis',(0.,0.,1.));
#46615=DIRECTION('center_axis',(-1.40646966953779E-16,0.,-1.));
#46616=DIRECTION('ref_axis',(-1.,0.,1.40646966953779E-16));
#46617=DIRECTION('center_axis',(0.,1.,0.));
#46618=DIRECTION('ref_axis',(0.,0.,1.));
#46619=DIRECTION('center_axis',(0.,1.,0.));
#46620=DIRECTION('ref_axis',(1.,0.,0.));
#46621=DIRECTION('center_axis',(0.,1.,0.));
#46622=DIRECTION('ref_axis',(0.,0.,1.));
#46623=DIRECTION('center_axis',(1.46081976924363E-16,0.,1.));
#46624=DIRECTION('ref_axis',(-1.,0.,1.46081976924363E-16));
#46625=DIRECTION('center_axis',(0.,1.,0.));
#46626=DIRECTION('ref_axis',(1.,0.,0.));
#46627=DIRECTION('center_axis',(0.,-1.,0.));
#46628=DIRECTION('ref_axis',(1.,0.,0.));
#46629=DIRECTION('center_axis',(1.38887491248569E-16,0.,1.));
#46630=DIRECTION('ref_axis',(-1.,0.,1.38887491248569E-16));
#46631=DIRECTION('center_axis',(0.,-1.,0.));
#46632=DIRECTION('ref_axis',(0.,0.,-1.));
#46633=DIRECTION('',(-1.,0.,0.));
#46634=DIRECTION('',(0.,0.,1.));
#46635=DIRECTION('',(-1.,0.,0.));
#46636=DIRECTION('',(0.,0.,1.));
#46637=DIRECTION('',(1.,0.,0.));
#46638=DIRECTION('',(0.,0.,1.));
#46639=DIRECTION('',(1.,0.,0.));
#46640=DIRECTION('',(1.38777878078145E-15,0.,1.));
#46641=DIRECTION('',(1.,0.,0.));
#46642=DIRECTION('',(0.,0.,1.));
#46643=DIRECTION('',(1.,0.,0.));
#46644=DIRECTION('',(0.,0.,1.));
#46645=DIRECTION('center_axis',(0.,-1.,0.));
#46646=DIRECTION('ref_axis',(0.,0.,-1.));
#46647=DIRECTION('',(0.,0.,-1.));
#46648=DIRECTION('',(1.,0.,0.));
#46649=DIRECTION('',(0.,0.,1.));
#46650=DIRECTION('',(1.,0.,0.));
#46651=DIRECTION('',(0.,0.,1.));
#46652=DIRECTION('',(-1.,0.,0.));
#46653=DIRECTION('',(-1.38777878078145E-15,0.,-1.));
#46654=DIRECTION('',(-1.,0.,0.));
#46655=DIRECTION('',(0.,0.,1.));
#46656=DIRECTION('',(1.,0.,0.));
#46657=DIRECTION('',(0.,0.,1.));
#46658=DIRECTION('',(1.,0.,0.));
#46659=DIRECTION('center_axis',(0.,0.,1.));
#46660=DIRECTION('ref_axis',(1.,0.,0.));
#46661=DIRECTION('',(0.,1.,0.));
#46662=DIRECTION('',(0.,-1.,0.));
#46663=DIRECTION('center_axis',(0.,0.,-1.));
#46664=DIRECTION('ref_axis',(-1.,0.,0.));
#46665=DIRECTION('',(0.,1.,0.));
#46666=DIRECTION('',(0.,-1.,0.));
#46667=DIRECTION('center_axis',(0.,0.,1.));
#46668=DIRECTION('ref_axis',(1.,0.,0.));
#46669=DIRECTION('',(0.,-1.,0.));
#46670=DIRECTION('',(0.,1.,0.));
#46671=DIRECTION('center_axis',(0.,0.,1.));
#46672=DIRECTION('ref_axis',(1.,0.,0.));
#46673=DIRECTION('',(0.,1.,0.));
#46674=DIRECTION('',(0.,1.,0.));
#46675=DIRECTION('center_axis',(1.,0.,0.));
#46676=DIRECTION('ref_axis',(0.,0.,-1.));
#46677=DIRECTION('center_axis',(0.,0.,-1.));
#46678=DIRECTION('ref_axis',(-1.,0.,0.));
#46679=DIRECTION('',(0.,1.,0.));
#46680=DIRECTION('',(0.,1.,0.));
#46681=DIRECTION('center_axis',(1.,0.,-1.38777878078145E-15));
#46682=DIRECTION('ref_axis',(-1.38777878078145E-15,0.,-1.));
#46683=DIRECTION('',(0.,1.,0.));
#46684=DIRECTION('center_axis',(0.,0.,-1.));
#46685=DIRECTION('ref_axis',(-1.,0.,0.));
#46686=DIRECTION('',(0.,-1.,0.));
#46687=DIRECTION('center_axis',(0.,0.,-1.));
#46688=DIRECTION('ref_axis',(-1.,0.,0.));
#46689=DIRECTION('',(-1.,-6.12323399573677E-17,8.67361737988424E-15));
#46690=DIRECTION('center_axis',(0.,0.,1.));
#46691=DIRECTION('ref_axis',(-1.,0.,0.));
#46692=DIRECTION('center_axis',(0.,0.,1.));
#46693=DIRECTION('ref_axis',(1.,0.,0.));
#46694=DIRECTION('center_axis',(0.,0.,1.));
#46695=DIRECTION('ref_axis',(1.,0.,0.));
#46696=DIRECTION('center_axis',(0.,0.,-1.));
#46697=DIRECTION('ref_axis',(-1.,0.,0.));
#46698=DIRECTION('',(-1.,0.,0.));
#46699=DIRECTION('center_axis',(0.,0.,-1.));
#46700=DIRECTION('ref_axis',(-1.,0.,0.));
#46701=DIRECTION('center_axis',(0.,0.,-1.));
#46702=DIRECTION('ref_axis',(-1.,0.,0.));
#46703=DIRECTION('',(0.,0.,1.));
#46704=DIRECTION('center_axis',(0.,0.,-1.));
#46705=DIRECTION('ref_axis',(-1.,0.,0.));
#46706=DIRECTION('',(0.,0.,1.));
#46707=DIRECTION('center_axis',(0.,0.,1.));
#46708=DIRECTION('ref_axis',(1.,0.,0.));
#46709=DIRECTION('center_axis',(0.,0.,-1.));
#46710=DIRECTION('ref_axis',(-1.,0.,0.));
#46711=DIRECTION('',(1.,6.12323399573677E-17,0.));
#46712=DIRECTION('center_axis',(0.,0.,-1.));
#46713=DIRECTION('ref_axis',(1.,0.,0.));
#46714=DIRECTION('center_axis',(0.,0.,-1.));
#46715=DIRECTION('ref_axis',(-1.,0.,0.));
#46716=DIRECTION('',(1.,0.,0.));
#46717=DIRECTION('center_axis',(0.,0.,1.));
#46718=DIRECTION('ref_axis',(-1.,0.,0.));
#46719=DIRECTION('center_axis',(0.,0.,1.));
#46720=DIRECTION('ref_axis',(1.,0.,0.));
#46721=DIRECTION('center_axis',(0.,0.,-1.));
#46722=DIRECTION('ref_axis',(-1.,0.,0.));
#46723=DIRECTION('',(0.,0.,1.));
#46724=DIRECTION('center_axis',(0.,0.,-1.));
#46725=DIRECTION('ref_axis',(-1.,0.,0.));
#46726=DIRECTION('',(0.,0.,1.));
#46727=DIRECTION('center_axis',(1.,0.,0.));
#46728=DIRECTION('ref_axis',(0.,1.,0.));
#46729=DIRECTION('center_axis',(1.,0.,0.));
#46730=DIRECTION('ref_axis',(0.,-1.,0.));
#46731=DIRECTION('',(1.,0.,0.));
#46732=DIRECTION('center_axis',(-1.,0.,0.));
#46733=DIRECTION('ref_axis',(0.,-1.,0.));
#46734=DIRECTION('',(-1.,0.,0.));
#46735=DIRECTION('center_axis',(6.12323399573677E-17,-1.,-1.38777878078145E-15));
#46736=DIRECTION('ref_axis',(-8.49769420904307E-32,1.38777878078145E-15,
-1.));
#46737=DIRECTION('',(0.,-1.38777878078145E-15,1.));
#46738=DIRECTION('',(1.,6.12323399573677E-17,0.));
#46739=DIRECTION('',(-8.49769420904308E-32,1.38777878078145E-15,-1.));
#46740=DIRECTION('',(1.,6.12323399573677E-17,0.));
#46741=DIRECTION('center_axis',(1.,0.,0.));
#46742=DIRECTION('ref_axis',(0.,1.,0.));
#46743=DIRECTION('center_axis',(1.,0.,0.));
#46744=DIRECTION('ref_axis',(0.,-1.,0.));
#46745=DIRECTION('',(1.,0.,0.));
#46746=DIRECTION('center_axis',(-1.,0.,0.));
#46747=DIRECTION('ref_axis',(0.,-1.,0.));
#46748=DIRECTION('',(-1.,0.,0.));
#46749=DIRECTION('center_axis',(0.,1.,0.));
#46750=DIRECTION('ref_axis',(0.,0.,1.));
#46751=DIRECTION('',(0.,0.,1.));
#46752=DIRECTION('',(0.,0.,1.));
#46753=DIRECTION('center_axis',(-1.,0.,0.));
#46754=DIRECTION('ref_axis',(0.,0.,1.));
#46755=DIRECTION('',(0.,-1.,0.));
#46756=DIRECTION('',(-6.12323399573677E-17,1.,0.));
#46757=DIRECTION('',(-6.12323399573677E-17,1.,0.));
#46758=DIRECTION('',(0.,-1.,0.));
#46759=DIRECTION('center_axis',(0.,0.,-1.));
#46760=DIRECTION('ref_axis',(-6.12323399573677E-17,1.,0.));
#46761=DIRECTION('',(0.,-1.,0.));
#46762=DIRECTION('center_axis',(-1.,0.,0.));
#46763=DIRECTION('ref_axis',(0.,0.,1.));
#46764=DIRECTION('',(0.,-1.,0.));
#46765=DIRECTION('',(0.,-1.,0.));
#46766=DIRECTION('',(0.,-1.,0.));
#46767=DIRECTION('center_axis',(0.,0.,-1.));
#46768=DIRECTION('ref_axis',(-1.,0.,0.));
#46769=DIRECTION('center_axis',(0.,0.,1.));
#46770=DIRECTION('ref_axis',(1.,0.,0.));
#46771=DIRECTION('center_axis',(0.,0.,-1.));
#46772=DIRECTION('ref_axis',(-6.12323399573677E-17,1.,0.));
#46773=DIRECTION('center_axis',(0.,0.,1.));
#46774=DIRECTION('ref_axis',(1.,0.,0.));
#46775=DIRECTION('',(1.,-6.12323399573677E-17,0.));
#46776=DIRECTION('center_axis',(0.,0.,-1.));
#46777=DIRECTION('ref_axis',(1.,0.,0.));
#46778=DIRECTION('center_axis',(0.,0.,-1.));
#46779=DIRECTION('ref_axis',(-1.,0.,0.));
#46780=DIRECTION('center_axis',(0.,0.,-1.));
#46781=DIRECTION('ref_axis',(-1.,0.,0.));
#46782=DIRECTION('center_axis',(0.,0.,1.));
#46783=DIRECTION('ref_axis',(1.,0.,0.));
#46784=DIRECTION('',(1.,0.,0.));
#46785=DIRECTION('center_axis',(0.,0.,1.));
#46786=DIRECTION('ref_axis',(1.,0.,0.));
#46787=DIRECTION('center_axis',(0.,0.,1.));
#46788=DIRECTION('ref_axis',(1.,0.,0.));
#46789=DIRECTION('',(0.,0.,1.));
#46790=DIRECTION('center_axis',(0.,0.,1.));
#46791=DIRECTION('ref_axis',(1.,0.,0.));
#46792=DIRECTION('',(0.,0.,1.));
#46793=DIRECTION('center_axis',(0.,0.,-1.));
#46794=DIRECTION('ref_axis',(-1.,0.,0.));
#46795=DIRECTION('center_axis',(0.,0.,1.));
#46796=DIRECTION('ref_axis',(1.,0.,0.));
#46797=DIRECTION('',(-1.,6.12323399573677E-17,-8.67361737988394E-15));
#46798=DIRECTION('center_axis',(0.,0.,1.));
#46799=DIRECTION('ref_axis',(-1.,0.,0.));
#46800=DIRECTION('center_axis',(0.,0.,1.));
#46801=DIRECTION('ref_axis',(1.,0.,0.));
#46802=DIRECTION('',(-1.,0.,0.));
#46803=DIRECTION('center_axis',(0.,0.,-1.));
#46804=DIRECTION('ref_axis',(1.,0.,0.));
#46805=DIRECTION('center_axis',(0.,0.,-1.));
#46806=DIRECTION('ref_axis',(-1.,0.,0.));
#46807=DIRECTION('center_axis',(0.,0.,1.));
#46808=DIRECTION('ref_axis',(1.,0.,0.));
#46809=DIRECTION('',(0.,0.,1.));
#46810=DIRECTION('center_axis',(0.,0.,1.));
#46811=DIRECTION('ref_axis',(1.,0.,0.));
#46812=DIRECTION('',(0.,0.,1.));
#46813=DIRECTION('center_axis',(-1.,0.,0.));
#46814=DIRECTION('ref_axis',(0.,-1.,0.));
#46815=DIRECTION('center_axis',(1.,0.,0.));
#46816=DIRECTION('ref_axis',(0.,1.,0.));
#46817=DIRECTION('',(1.,0.,0.));
#46818=DIRECTION('center_axis',(-1.,0.,0.));
#46819=DIRECTION('ref_axis',(0.,1.,0.));
#46820=DIRECTION('',(-1.,0.,0.));
#46821=DIRECTION('center_axis',(6.12323399573677E-17,1.,0.));
#46822=DIRECTION('ref_axis',(0.,0.,-1.));
#46823=DIRECTION('',(-1.,6.12323399573677E-17,0.));
#46824=DIRECTION('',(0.,0.,-1.));
#46825=DIRECTION('',(-1.,6.12323399573677E-17,0.));
#46826=DIRECTION('',(0.,0.,1.));
#46827=DIRECTION('center_axis',(1.,0.,0.));
#46828=DIRECTION('ref_axis',(0.,1.,0.));
#46829=DIRECTION('center_axis',(1.,0.,0.));
#46830=DIRECTION('ref_axis',(0.,1.,0.));
#46831=DIRECTION('',(1.,0.,0.));
#46832=DIRECTION('center_axis',(-1.,0.,0.));
#46833=DIRECTION('ref_axis',(0.,1.,0.));
#46834=DIRECTION('',(-1.,0.,0.));
#46835=DIRECTION('center_axis',(0.,1.,0.));
#46836=DIRECTION('ref_axis',(0.,0.,1.));
#46837=DIRECTION('',(0.,0.,1.));
#46838=DIRECTION('',(0.,0.,1.));
#46839=DIRECTION('center_axis',(1.,0.,0.));
#46840=DIRECTION('ref_axis',(0.,0.,-1.));
#46841=DIRECTION('',(0.,1.,0.));
#46842=DIRECTION('',(6.12323399573677E-17,1.,0.));
#46843=DIRECTION('',(6.12323399573677E-17,1.,0.));
#46844=DIRECTION('',(0.,1.,0.));
#46845=DIRECTION('center_axis',(0.,0.,1.));
#46846=DIRECTION('ref_axis',(6.12323399573677E-17,1.,0.));
#46847=DIRECTION('',(0.,-1.,0.));
#46848=DIRECTION('center_axis',(1.,0.,0.));
#46849=DIRECTION('ref_axis',(0.,0.,-1.));
#46850=DIRECTION('',(0.,1.,0.));
#46851=DIRECTION('',(0.,1.,0.));
#46852=DIRECTION('',(0.,-1.,0.));
#46853=DIRECTION('center_axis',(0.,0.,1.));
#46854=DIRECTION('ref_axis',(1.,0.,0.));
#46855=DIRECTION('center_axis',(0.,0.,1.));
#46856=DIRECTION('ref_axis',(1.,0.,0.));
#46857=DIRECTION('center_axis',(0.,0.,1.));
#46858=DIRECTION('ref_axis',(6.12323399573677E-17,1.,0.));
#46859=DIRECTION('center_axis',(0.,1.,0.));
#46860=DIRECTION('ref_axis',(1.,0.,0.));
#46861=DIRECTION('',(0.150042296859641,0.,-0.988679578606276));
#46862=DIRECTION('',(0.931242779705752,0.,-0.364399348580517));
#46863=DIRECTION('',(0.781200482846104,0.,0.624280230025758));
#46864=DIRECTION('',(-0.150042296859647,0.,0.988679578606275));
#46865=DIRECTION('',(-0.931242779705751,0.,0.364399348580519));
#46866=DIRECTION('',(-0.781200482846105,0.,-0.624280230025758));
#46867=DIRECTION('',(0.150042296859641,0.,-0.988679578606276));
#46868=DIRECTION('',(0.931242779705752,0.,-0.364399348580517));
#46869=DIRECTION('',(0.781200482846104,0.,0.624280230025758));
#46870=DIRECTION('',(-0.150042296859647,0.,0.988679578606275));
#46871=DIRECTION('',(-0.931242779705751,0.,0.364399348580519));
#46872=DIRECTION('',(-0.781200482846105,0.,-0.624280230025758));
#46873=DIRECTION('',(0.150042296859641,0.,-0.988679578606276));
#46874=DIRECTION('',(0.931242779705752,0.,-0.364399348580517));
#46875=DIRECTION('',(0.781200482846104,0.,0.624280230025758));
#46876=DIRECTION('',(-0.150042296859647,0.,0.988679578606275));
#46877=DIRECTION('',(-0.931242779705751,0.,0.364399348580519));
#46878=DIRECTION('',(-0.781200482846105,0.,-0.624280230025758));
#46879=DIRECTION('',(0.150042296859641,0.,-0.988679578606276));
#46880=DIRECTION('',(0.931242779705752,0.,-0.364399348580517));
#46881=DIRECTION('',(0.781200482846104,0.,0.624280230025758));
#46882=DIRECTION('',(-0.150042296859647,0.,0.988679578606275));
#46883=DIRECTION('',(-0.931242779705751,0.,0.364399348580519));
#46884=DIRECTION('',(-0.781200482846105,0.,-0.624280230025758));
#46885=DIRECTION('',(0.150042296859641,0.,-0.988679578606276));
#46886=DIRECTION('',(0.931242779705752,0.,-0.364399348580517));
#46887=DIRECTION('',(0.781200482846104,0.,0.624280230025758));
#46888=DIRECTION('',(-0.150042296859647,0.,0.988679578606275));
#46889=DIRECTION('',(-0.931242779705751,0.,0.364399348580519));
#46890=DIRECTION('',(-0.781200482846105,0.,-0.624280230025758));
#46891=DIRECTION('',(0.150042296859641,0.,-0.988679578606276));
#46892=DIRECTION('',(0.931242779705752,0.,-0.364399348580517));
#46893=DIRECTION('',(0.781200482846104,0.,0.624280230025758));
#46894=DIRECTION('',(-0.150042296859647,0.,0.988679578606275));
#46895=DIRECTION('',(-0.931242779705751,0.,0.364399348580519));
#46896=DIRECTION('',(-0.781200482846105,0.,-0.624280230025758));
#46897=DIRECTION('',(0.150042296859641,0.,-0.988679578606276));
#46898=DIRECTION('',(0.931242779705752,0.,-0.364399348580517));
#46899=DIRECTION('',(0.781200482846104,0.,0.624280230025758));
#46900=DIRECTION('',(-0.150042296859647,0.,0.988679578606275));
#46901=DIRECTION('',(-0.931242779705751,0.,0.364399348580519));
#46902=DIRECTION('',(-0.781200482846105,0.,-0.624280230025758));
#46903=DIRECTION('',(0.150042296859641,0.,-0.988679578606276));
#46904=DIRECTION('',(0.931242779705752,0.,-0.364399348580517));
#46905=DIRECTION('',(0.781200482846104,0.,0.624280230025758));
#46906=DIRECTION('',(-0.150042296859647,0.,0.988679578606275));
#46907=DIRECTION('',(-0.931242779705751,0.,0.364399348580519));
#46908=DIRECTION('',(-0.781200482846105,0.,-0.624280230025758));
#46909=DIRECTION('',(0.150042296859641,0.,-0.988679578606276));
#46910=DIRECTION('',(0.931242779705752,0.,-0.364399348580517));
#46911=DIRECTION('',(0.781200482846104,0.,0.624280230025758));
#46912=DIRECTION('',(-0.150042296859647,0.,0.988679578606275));
#46913=DIRECTION('',(-0.931242779705751,0.,0.364399348580519));
#46914=DIRECTION('',(-0.781200482846105,0.,-0.624280230025758));
#46915=DIRECTION('',(0.150042296859641,0.,-0.988679578606276));
#46916=DIRECTION('',(0.931242779705752,0.,-0.364399348580517));
#46917=DIRECTION('',(0.781200482846104,0.,0.624280230025758));
#46918=DIRECTION('',(-0.150042296859647,0.,0.988679578606275));
#46919=DIRECTION('',(-0.931242779705751,0.,0.364399348580519));
#46920=DIRECTION('',(-0.781200482846105,0.,-0.624280230025758));
#46921=DIRECTION('',(0.150042296859641,0.,-0.988679578606276));
#46922=DIRECTION('',(0.931242779705752,0.,-0.364399348580517));
#46923=DIRECTION('',(0.781200482846104,0.,0.624280230025758));
#46924=DIRECTION('',(-0.150042296859647,0.,0.988679578606275));
#46925=DIRECTION('',(-0.931242779705751,0.,0.364399348580519));
#46926=DIRECTION('',(-0.781200482846105,0.,-0.624280230025758));
#46927=DIRECTION('',(0.150042296859641,0.,-0.988679578606276));
#46928=DIRECTION('',(0.931242779705752,0.,-0.364399348580517));
#46929=DIRECTION('',(0.781200482846104,0.,0.624280230025758));
#46930=DIRECTION('',(-0.150042296859647,0.,0.988679578606275));
#46931=DIRECTION('',(-0.931242779705751,0.,0.364399348580519));
#46932=DIRECTION('',(-0.781200482846105,0.,-0.624280230025758));
#46933=DIRECTION('',(0.150042296859641,0.,-0.988679578606276));
#46934=DIRECTION('',(0.931242779705752,0.,-0.364399348580517));
#46935=DIRECTION('',(0.781200482846104,0.,0.624280230025758));
#46936=DIRECTION('',(-0.150042296859647,0.,0.988679578606275));
#46937=DIRECTION('',(-0.931242779705751,0.,0.364399348580519));
#46938=DIRECTION('',(-0.781200482846105,0.,-0.624280230025758));
#46939=DIRECTION('',(0.150042296859641,0.,-0.988679578606276));
#46940=DIRECTION('',(0.931242779705752,0.,-0.364399348580517));
#46941=DIRECTION('',(0.781200482846104,0.,0.624280230025758));
#46942=DIRECTION('',(-0.150042296859647,0.,0.988679578606275));
#46943=DIRECTION('',(-0.931242779705751,0.,0.364399348580519));
#46944=DIRECTION('',(-0.781200482846105,0.,-0.624280230025758));
#46945=DIRECTION('',(0.150042296859641,0.,-0.988679578606276));
#46946=DIRECTION('',(0.931242779705752,0.,-0.364399348580517));
#46947=DIRECTION('',(0.781200482846104,0.,0.624280230025758));
#46948=DIRECTION('',(-0.150042296859647,0.,0.988679578606275));
#46949=DIRECTION('',(-0.931242779705751,0.,0.364399348580519));
#46950=DIRECTION('',(-0.781200482846105,0.,-0.624280230025758));
#46951=DIRECTION('',(0.150042296859641,0.,-0.988679578606276));
#46952=DIRECTION('',(0.931242779705752,0.,-0.364399348580517));
#46953=DIRECTION('',(0.781200482846104,0.,0.624280230025758));
#46954=DIRECTION('',(-0.150042296859647,0.,0.988679578606275));
#46955=DIRECTION('',(-0.931242779705751,0.,0.364399348580519));
#46956=DIRECTION('',(-0.781200482846105,0.,-0.624280230025758));
#46957=DIRECTION('',(0.150042296859641,0.,-0.988679578606276));
#46958=DIRECTION('',(0.931242779705752,0.,-0.364399348580517));
#46959=DIRECTION('',(0.781200482846104,0.,0.624280230025758));
#46960=DIRECTION('',(-0.150042296859647,0.,0.988679578606275));
#46961=DIRECTION('',(-0.931242779705751,0.,0.364399348580519));
#46962=DIRECTION('',(-0.781200482846105,0.,-0.624280230025758));
#46963=DIRECTION('',(0.150042296859641,0.,-0.988679578606276));
#46964=DIRECTION('',(0.931242779705752,0.,-0.364399348580517));
#46965=DIRECTION('',(0.781200482846104,0.,0.624280230025758));
#46966=DIRECTION('',(-0.150042296859647,0.,0.988679578606275));
#46967=DIRECTION('',(-0.931242779705751,0.,0.364399348580519));
#46968=DIRECTION('',(-0.781200482846105,0.,-0.624280230025758));
#46969=DIRECTION('',(0.150042296859641,0.,-0.988679578606276));
#46970=DIRECTION('',(0.931242779705752,0.,-0.364399348580517));
#46971=DIRECTION('',(0.781200482846104,0.,0.624280230025758));
#46972=DIRECTION('',(-0.150042296859647,0.,0.988679578606275));
#46973=DIRECTION('',(-0.931242779705751,0.,0.364399348580519));
#46974=DIRECTION('',(-0.781200482846105,0.,-0.624280230025758));
#46975=DIRECTION('',(0.150042296859641,0.,-0.988679578606276));
#46976=DIRECTION('',(0.931242779705752,0.,-0.364399348580517));
#46977=DIRECTION('',(0.781200482846104,0.,0.624280230025758));
#46978=DIRECTION('',(-0.150042296859647,0.,0.988679578606275));
#46979=DIRECTION('',(-0.931242779705751,0.,0.364399348580519));
#46980=DIRECTION('',(-0.781200482846105,0.,-0.624280230025758));
#46981=DIRECTION('',(0.150042296859641,0.,-0.988679578606276));
#46982=DIRECTION('',(0.931242779705752,0.,-0.364399348580517));
#46983=DIRECTION('',(0.781200482846104,0.,0.624280230025758));
#46984=DIRECTION('',(-0.150042296859647,0.,0.988679578606275));
#46985=DIRECTION('',(-0.931242779705751,0.,0.364399348580519));
#46986=DIRECTION('',(-0.781200482846105,0.,-0.624280230025758));
#46987=DIRECTION('',(0.150042296859641,0.,-0.988679578606276));
#46988=DIRECTION('',(0.931242779705752,0.,-0.364399348580517));
#46989=DIRECTION('',(0.781200482846104,0.,0.624280230025758));
#46990=DIRECTION('',(-0.150042296859647,0.,0.988679578606275));
#46991=DIRECTION('',(-0.931242779705751,0.,0.364399348580519));
#46992=DIRECTION('',(-0.781200482846105,0.,-0.624280230025758));
#46993=DIRECTION('',(0.150042296859641,0.,-0.988679578606276));
#46994=DIRECTION('',(0.931242779705752,0.,-0.364399348580517));
#46995=DIRECTION('',(0.781200482846104,0.,0.624280230025758));
#46996=DIRECTION('',(-0.150042296859647,0.,0.988679578606275));
#46997=DIRECTION('',(-0.931242779705751,0.,0.364399348580519));
#46998=DIRECTION('',(-0.781200482846105,0.,-0.624280230025758));
#46999=DIRECTION('',(0.150042296859641,0.,-0.988679578606276));
#47000=DIRECTION('',(0.931242779705752,0.,-0.364399348580517));
#47001=DIRECTION('',(0.781200482846104,0.,0.624280230025758));
#47002=DIRECTION('',(-0.150042296859647,0.,0.988679578606275));
#47003=DIRECTION('',(-0.931242779705751,0.,0.364399348580519));
#47004=DIRECTION('',(-0.781200482846105,0.,-0.624280230025758));
#47005=DIRECTION('',(0.150042296859641,0.,-0.988679578606276));
#47006=DIRECTION('',(0.931242779705752,0.,-0.364399348580517));
#47007=DIRECTION('',(0.781200482846104,0.,0.624280230025758));
#47008=DIRECTION('',(-0.150042296859647,0.,0.988679578606275));
#47009=DIRECTION('',(-0.931242779705751,0.,0.364399348580519));
#47010=DIRECTION('',(-0.781200482846105,0.,-0.624280230025758));
#47011=DIRECTION('',(0.150042296859641,0.,-0.988679578606276));
#47012=DIRECTION('',(0.931242779705752,0.,-0.364399348580517));
#47013=DIRECTION('',(0.781200482846104,0.,0.624280230025758));
#47014=DIRECTION('',(-0.150042296859647,0.,0.988679578606275));
#47015=DIRECTION('',(-0.931242779705751,0.,0.364399348580519));
#47016=DIRECTION('',(-0.781200482846105,0.,-0.624280230025758));
#47017=DIRECTION('',(0.150042296859641,0.,-0.988679578606276));
#47018=DIRECTION('',(0.931242779705752,0.,-0.364399348580517));
#47019=DIRECTION('',(0.781200482846104,0.,0.624280230025758));
#47020=DIRECTION('',(-0.150042296859647,0.,0.988679578606275));
#47021=DIRECTION('',(-0.931242779705751,0.,0.364399348580519));
#47022=DIRECTION('',(-0.781200482846105,0.,-0.624280230025758));
#47023=DIRECTION('',(0.150042296859641,0.,-0.988679578606276));
#47024=DIRECTION('',(0.931242779705752,0.,-0.364399348580517));
#47025=DIRECTION('',(0.781200482846104,0.,0.624280230025758));
#47026=DIRECTION('',(-0.150042296859647,0.,0.988679578606275));
#47027=DIRECTION('',(-0.931242779705751,0.,0.364399348580519));
#47028=DIRECTION('',(-0.781200482846105,0.,-0.624280230025758));
#47029=DIRECTION('',(0.150042296859641,0.,-0.988679578606276));
#47030=DIRECTION('',(0.931242779705752,0.,-0.364399348580517));
#47031=DIRECTION('',(0.781200482846104,0.,0.624280230025758));
#47032=DIRECTION('',(-0.150042296859647,0.,0.988679578606275));
#47033=DIRECTION('',(-0.931242779705751,0.,0.364399348580519));
#47034=DIRECTION('',(-0.781200482846105,0.,-0.624280230025758));
#47035=DIRECTION('',(0.150042296859641,0.,-0.988679578606276));
#47036=DIRECTION('',(0.931242779705752,0.,-0.364399348580517));
#47037=DIRECTION('',(0.781200482846104,0.,0.624280230025758));
#47038=DIRECTION('',(-0.150042296859647,0.,0.988679578606275));
#47039=DIRECTION('',(-0.931242779705751,0.,0.364399348580519));
#47040=DIRECTION('',(-0.781200482846105,0.,-0.624280230025758));
#47041=DIRECTION('',(0.150042296859641,0.,-0.988679578606276));
#47042=DIRECTION('',(0.931242779705752,0.,-0.364399348580517));
#47043=DIRECTION('',(0.781200482846104,0.,0.624280230025758));
#47044=DIRECTION('',(-0.150042296859647,0.,0.988679578606275));
#47045=DIRECTION('',(-0.931242779705751,0.,0.364399348580519));
#47046=DIRECTION('',(-0.781200482846105,0.,-0.624280230025758));
#47047=DIRECTION('',(0.150042296859641,0.,-0.988679578606276));
#47048=DIRECTION('',(0.931242779705752,0.,-0.364399348580517));
#47049=DIRECTION('',(0.781200482846104,0.,0.624280230025758));
#47050=DIRECTION('',(-0.150042296859647,0.,0.988679578606275));
#47051=DIRECTION('',(-0.931242779705751,0.,0.364399348580519));
#47052=DIRECTION('',(-0.781200482846105,0.,-0.624280230025758));
#47053=DIRECTION('',(0.150042296859641,0.,-0.988679578606276));
#47054=DIRECTION('',(0.931242779705752,0.,-0.364399348580517));
#47055=DIRECTION('',(0.781200482846104,0.,0.624280230025758));
#47056=DIRECTION('',(-0.150042296859647,0.,0.988679578606275));
#47057=DIRECTION('',(-0.931242779705751,0.,0.364399348580519));
#47058=DIRECTION('',(-0.781200482846105,0.,-0.624280230025758));
#47059=DIRECTION('',(0.150042296859641,0.,-0.988679578606276));
#47060=DIRECTION('',(0.931242779705752,0.,-0.364399348580517));
#47061=DIRECTION('',(0.781200482846104,0.,0.624280230025758));
#47062=DIRECTION('',(-0.150042296859647,0.,0.988679578606275));
#47063=DIRECTION('',(-0.931242779705751,0.,0.364399348580519));
#47064=DIRECTION('',(-0.781200482846105,0.,-0.624280230025758));
#47065=DIRECTION('',(0.150042296859641,0.,-0.988679578606276));
#47066=DIRECTION('',(0.931242779705752,0.,-0.364399348580517));
#47067=DIRECTION('',(0.781200482846104,0.,0.624280230025758));
#47068=DIRECTION('',(-0.150042296859647,0.,0.988679578606275));
#47069=DIRECTION('',(-0.931242779705751,0.,0.364399348580519));
#47070=DIRECTION('',(-0.781200482846105,0.,-0.624280230025758));
#47071=DIRECTION('',(0.150042296859641,0.,-0.988679578606276));
#47072=DIRECTION('',(0.931242779705752,0.,-0.364399348580517));
#47073=DIRECTION('',(0.781200482846104,0.,0.624280230025758));
#47074=DIRECTION('',(-0.150042296859647,0.,0.988679578606275));
#47075=DIRECTION('',(-0.931242779705751,0.,0.364399348580519));
#47076=DIRECTION('',(-0.781200482846105,0.,-0.624280230025758));
#47077=DIRECTION('',(0.150042296859641,0.,-0.988679578606276));
#47078=DIRECTION('',(0.931242779705752,0.,-0.364399348580517));
#47079=DIRECTION('',(0.781200482846104,0.,0.624280230025758));
#47080=DIRECTION('',(-0.150042296859647,0.,0.988679578606275));
#47081=DIRECTION('',(-0.931242779705751,0.,0.364399348580519));
#47082=DIRECTION('',(-0.781200482846105,0.,-0.624280230025758));
#47083=DIRECTION('',(0.150042296859641,0.,-0.988679578606276));
#47084=DIRECTION('',(0.931242779705752,0.,-0.364399348580517));
#47085=DIRECTION('',(0.781200482846104,0.,0.624280230025758));
#47086=DIRECTION('',(-0.150042296859647,0.,0.988679578606275));
#47087=DIRECTION('',(-0.931242779705751,0.,0.364399348580519));
#47088=DIRECTION('',(-0.781200482846105,0.,-0.624280230025758));
#47089=DIRECTION('',(0.150042296859641,0.,-0.988679578606276));
#47090=DIRECTION('',(0.931242779705752,0.,-0.364399348580517));
#47091=DIRECTION('',(0.781200482846104,0.,0.624280230025758));
#47092=DIRECTION('',(-0.150042296859647,0.,0.988679578606275));
#47093=DIRECTION('',(-0.931242779705751,0.,0.364399348580519));
#47094=DIRECTION('',(-0.781200482846105,0.,-0.624280230025758));
#47095=DIRECTION('',(0.150042296859641,0.,-0.988679578606276));
#47096=DIRECTION('',(0.931242779705752,0.,-0.364399348580517));
#47097=DIRECTION('',(0.781200482846104,0.,0.624280230025758));
#47098=DIRECTION('',(-0.150042296859647,0.,0.988679578606275));
#47099=DIRECTION('',(-0.931242779705751,0.,0.364399348580519));
#47100=DIRECTION('',(-0.781200482846105,0.,-0.624280230025758));
#47101=DIRECTION('',(0.150042296859641,0.,-0.988679578606276));
#47102=DIRECTION('',(0.931242779705752,0.,-0.364399348580517));
#47103=DIRECTION('',(0.781200482846104,0.,0.624280230025758));
#47104=DIRECTION('',(-0.150042296859647,0.,0.988679578606275));
#47105=DIRECTION('',(-0.931242779705751,0.,0.364399348580519));
#47106=DIRECTION('',(-0.781200482846105,0.,-0.624280230025758));
#47107=DIRECTION('',(0.150042296859641,0.,-0.988679578606276));
#47108=DIRECTION('',(0.931242779705752,0.,-0.364399348580517));
#47109=DIRECTION('',(0.781200482846104,0.,0.624280230025758));
#47110=DIRECTION('',(-0.150042296859647,0.,0.988679578606275));
#47111=DIRECTION('',(-0.931242779705751,0.,0.364399348580519));
#47112=DIRECTION('',(-0.781200482846105,0.,-0.624280230025758));
#47113=DIRECTION('',(0.150042296859641,0.,-0.988679578606276));
#47114=DIRECTION('',(0.931242779705752,0.,-0.364399348580517));
#47115=DIRECTION('',(0.781200482846104,0.,0.624280230025758));
#47116=DIRECTION('',(-0.150042296859647,0.,0.988679578606275));
#47117=DIRECTION('',(-0.931242779705751,0.,0.364399348580519));
#47118=DIRECTION('',(-0.781200482846105,0.,-0.624280230025758));
#47119=DIRECTION('',(0.150042296859641,0.,-0.988679578606276));
#47120=DIRECTION('',(0.931242779705752,0.,-0.364399348580517));
#47121=DIRECTION('',(0.781200482846104,0.,0.624280230025758));
#47122=DIRECTION('',(-0.150042296859647,0.,0.988679578606275));
#47123=DIRECTION('',(-0.931242779705751,0.,0.364399348580519));
#47124=DIRECTION('',(-0.781200482846105,0.,-0.624280230025758));
#47125=DIRECTION('',(0.150042296859641,0.,-0.988679578606276));
#47126=DIRECTION('',(0.931242779705752,0.,-0.364399348580517));
#47127=DIRECTION('',(0.781200482846104,0.,0.624280230025758));
#47128=DIRECTION('',(-0.150042296859647,0.,0.988679578606275));
#47129=DIRECTION('',(-0.931242779705751,0.,0.364399348580519));
#47130=DIRECTION('',(-0.781200482846105,0.,-0.624280230025758));
#47131=DIRECTION('',(0.150042296859641,0.,-0.988679578606276));
#47132=DIRECTION('',(0.931242779705752,0.,-0.364399348580517));
#47133=DIRECTION('',(0.781200482846104,0.,0.624280230025758));
#47134=DIRECTION('',(-0.150042296859647,0.,0.988679578606275));
#47135=DIRECTION('',(-0.931242779705751,0.,0.364399348580519));
#47136=DIRECTION('',(-0.781200482846105,0.,-0.624280230025758));
#47137=DIRECTION('',(0.150042296859641,0.,-0.988679578606276));
#47138=DIRECTION('',(0.931242779705752,0.,-0.364399348580517));
#47139=DIRECTION('',(0.781200482846104,0.,0.624280230025758));
#47140=DIRECTION('',(-0.150042296859647,0.,0.988679578606275));
#47141=DIRECTION('',(-0.931242779705751,0.,0.364399348580519));
#47142=DIRECTION('',(-0.781200482846105,0.,-0.624280230025758));
#47143=DIRECTION('',(0.150042296859641,0.,-0.988679578606276));
#47144=DIRECTION('',(0.931242779705752,0.,-0.364399348580517));
#47145=DIRECTION('',(0.781200482846104,0.,0.624280230025758));
#47146=DIRECTION('',(-0.150042296859647,0.,0.988679578606275));
#47147=DIRECTION('',(-0.931242779705751,0.,0.364399348580519));
#47148=DIRECTION('',(-0.781200482846105,0.,-0.624280230025758));
#47149=DIRECTION('',(0.150042296859641,0.,-0.988679578606276));
#47150=DIRECTION('',(0.931242779705752,0.,-0.364399348580517));
#47151=DIRECTION('',(0.781200482846104,0.,0.624280230025758));
#47152=DIRECTION('',(-0.150042296859647,0.,0.988679578606275));
#47153=DIRECTION('',(-0.931242779705751,0.,0.364399348580519));
#47154=DIRECTION('',(-0.781200482846105,0.,-0.624280230025758));
#47155=DIRECTION('',(0.150042296859641,0.,-0.988679578606276));
#47156=DIRECTION('',(0.931242779705752,0.,-0.364399348580517));
#47157=DIRECTION('',(0.781200482846104,0.,0.624280230025758));
#47158=DIRECTION('',(-0.150042296859647,0.,0.988679578606275));
#47159=DIRECTION('',(-0.931242779705751,0.,0.364399348580519));
#47160=DIRECTION('',(-0.781200482846105,0.,-0.624280230025758));
#47161=DIRECTION('',(0.150042296859641,0.,-0.988679578606276));
#47162=DIRECTION('',(0.931242779705752,0.,-0.364399348580517));
#47163=DIRECTION('',(0.781200482846104,0.,0.624280230025758));
#47164=DIRECTION('',(-0.150042296859647,0.,0.988679578606275));
#47165=DIRECTION('',(-0.931242779705751,0.,0.364399348580519));
#47166=DIRECTION('',(-0.781200482846105,0.,-0.624280230025758));
#47167=DIRECTION('',(0.150042296859641,0.,-0.988679578606276));
#47168=DIRECTION('',(0.931242779705752,0.,-0.364399348580517));
#47169=DIRECTION('',(0.781200482846104,0.,0.624280230025758));
#47170=DIRECTION('',(-0.150042296859647,0.,0.988679578606275));
#47171=DIRECTION('',(-0.931242779705751,0.,0.364399348580519));
#47172=DIRECTION('',(-0.781200482846105,0.,-0.624280230025758));
#47173=DIRECTION('',(0.150042296859641,0.,-0.988679578606276));
#47174=DIRECTION('',(0.931242779705752,0.,-0.364399348580517));
#47175=DIRECTION('',(0.781200482846104,0.,0.624280230025758));
#47176=DIRECTION('',(-0.150042296859647,0.,0.988679578606275));
#47177=DIRECTION('',(-0.931242779705751,0.,0.364399348580519));
#47178=DIRECTION('',(-0.781200482846105,0.,-0.624280230025758));
#47179=DIRECTION('',(0.150042296859641,0.,-0.988679578606276));
#47180=DIRECTION('',(0.931242779705752,0.,-0.364399348580517));
#47181=DIRECTION('',(0.781200482846104,0.,0.624280230025758));
#47182=DIRECTION('',(-0.150042296859647,0.,0.988679578606275));
#47183=DIRECTION('',(-0.931242779705751,0.,0.364399348580519));
#47184=DIRECTION('',(-0.781200482846105,0.,-0.624280230025758));
#47185=DIRECTION('',(0.150042296859641,0.,-0.988679578606276));
#47186=DIRECTION('',(0.931242779705752,0.,-0.364399348580517));
#47187=DIRECTION('',(0.781200482846104,0.,0.624280230025758));
#47188=DIRECTION('',(-0.150042296859647,0.,0.988679578606275));
#47189=DIRECTION('',(-0.931242779705751,0.,0.364399348580519));
#47190=DIRECTION('',(-0.781200482846105,0.,-0.624280230025758));
#47191=DIRECTION('',(0.150042296859641,0.,-0.988679578606276));
#47192=DIRECTION('',(0.931242779705752,0.,-0.364399348580517));
#47193=DIRECTION('',(0.781200482846104,0.,0.624280230025758));
#47194=DIRECTION('',(-0.150042296859647,0.,0.988679578606275));
#47195=DIRECTION('',(-0.931242779705751,0.,0.364399348580519));
#47196=DIRECTION('',(-0.781200482846105,0.,-0.624280230025758));
#47197=DIRECTION('',(0.150042296859641,0.,-0.988679578606276));
#47198=DIRECTION('',(0.931242779705752,0.,-0.364399348580517));
#47199=DIRECTION('',(0.781200482846104,0.,0.624280230025758));
#47200=DIRECTION('',(-0.150042296859647,0.,0.988679578606275));
#47201=DIRECTION('',(-0.931242779705751,0.,0.364399348580519));
#47202=DIRECTION('',(-0.781200482846105,0.,-0.624280230025758));
#47203=DIRECTION('',(0.150042296859641,0.,-0.988679578606276));
#47204=DIRECTION('',(0.931242779705752,0.,-0.364399348580517));
#47205=DIRECTION('',(0.781200482846104,0.,0.624280230025758));
#47206=DIRECTION('',(-0.150042296859647,0.,0.988679578606275));
#47207=DIRECTION('',(-0.931242779705751,0.,0.364399348580519));
#47208=DIRECTION('',(-0.781200482846105,0.,-0.624280230025758));
#47209=DIRECTION('',(0.150042296859641,0.,-0.988679578606276));
#47210=DIRECTION('',(0.931242779705752,0.,-0.364399348580517));
#47211=DIRECTION('',(0.781200482846104,0.,0.624280230025758));
#47212=DIRECTION('',(-0.150042296859647,0.,0.988679578606275));
#47213=DIRECTION('',(-0.931242779705751,0.,0.364399348580519));
#47214=DIRECTION('',(-0.781200482846105,0.,-0.624280230025758));
#47215=DIRECTION('',(0.150042296859641,0.,-0.988679578606276));
#47216=DIRECTION('',(0.931242779705752,0.,-0.364399348580517));
#47217=DIRECTION('',(0.781200482846104,0.,0.624280230025758));
#47218=DIRECTION('',(-0.150042296859647,0.,0.988679578606275));
#47219=DIRECTION('',(-0.931242779705751,0.,0.364399348580519));
#47220=DIRECTION('',(-0.781200482846105,0.,-0.624280230025758));
#47221=DIRECTION('',(0.150042296859641,0.,-0.988679578606276));
#47222=DIRECTION('',(0.931242779705752,0.,-0.364399348580517));
#47223=DIRECTION('',(0.781200482846104,0.,0.624280230025758));
#47224=DIRECTION('',(-0.150042296859647,0.,0.988679578606275));
#47225=DIRECTION('',(-0.931242779705751,0.,0.364399348580519));
#47226=DIRECTION('',(-0.781200482846105,0.,-0.624280230025758));
#47227=DIRECTION('',(0.150042296859641,0.,-0.988679578606276));
#47228=DIRECTION('',(0.931242779705752,0.,-0.364399348580517));
#47229=DIRECTION('',(0.781200482846104,0.,0.624280230025758));
#47230=DIRECTION('',(-0.150042296859647,0.,0.988679578606275));
#47231=DIRECTION('',(-0.931242779705751,0.,0.364399348580519));
#47232=DIRECTION('',(-0.781200482846105,0.,-0.624280230025758));
#47233=DIRECTION('',(0.150042296859641,0.,-0.988679578606276));
#47234=DIRECTION('',(0.931242779705752,0.,-0.364399348580517));
#47235=DIRECTION('',(0.781200482846104,0.,0.624280230025758));
#47236=DIRECTION('',(-0.150042296859647,0.,0.988679578606275));
#47237=DIRECTION('',(-0.931242779705751,0.,0.364399348580519));
#47238=DIRECTION('',(-0.781200482846105,0.,-0.624280230025758));
#47239=DIRECTION('',(0.150042296859641,0.,-0.988679578606276));
#47240=DIRECTION('',(0.931242779705752,0.,-0.364399348580517));
#47241=DIRECTION('',(0.781200482846104,0.,0.624280230025758));
#47242=DIRECTION('',(-0.150042296859647,0.,0.988679578606275));
#47243=DIRECTION('',(-0.931242779705751,0.,0.364399348580519));
#47244=DIRECTION('',(-0.781200482846105,0.,-0.624280230025758));
#47245=DIRECTION('',(0.150042296859641,0.,-0.988679578606276));
#47246=DIRECTION('',(0.931242779705752,0.,-0.364399348580517));
#47247=DIRECTION('',(0.781200482846104,0.,0.624280230025758));
#47248=DIRECTION('',(-0.150042296859647,0.,0.988679578606275));
#47249=DIRECTION('',(-0.931242779705751,0.,0.364399348580519));
#47250=DIRECTION('',(-0.781200482846105,0.,-0.624280230025758));
#47251=DIRECTION('',(0.150042296859641,0.,-0.988679578606276));
#47252=DIRECTION('',(0.931242779705752,0.,-0.364399348580517));
#47253=DIRECTION('',(0.781200482846104,0.,0.624280230025758));
#47254=DIRECTION('',(-0.150042296859647,0.,0.988679578606275));
#47255=DIRECTION('',(-0.931242779705751,0.,0.364399348580519));
#47256=DIRECTION('',(-0.781200482846105,0.,-0.624280230025758));
#47257=DIRECTION('',(0.150042296859641,0.,-0.988679578606276));
#47258=DIRECTION('',(0.931242779705752,0.,-0.364399348580517));
#47259=DIRECTION('',(0.781200482846104,0.,0.624280230025758));
#47260=DIRECTION('',(-0.150042296859647,0.,0.988679578606275));
#47261=DIRECTION('',(-0.931242779705751,0.,0.364399348580519));
#47262=DIRECTION('',(-0.781200482846105,0.,-0.624280230025758));
#47263=DIRECTION('',(0.150042296859641,0.,-0.988679578606276));
#47264=DIRECTION('',(0.931242779705752,0.,-0.364399348580517));
#47265=DIRECTION('',(0.781200482846104,0.,0.624280230025758));
#47266=DIRECTION('',(-0.150042296859647,0.,0.988679578606275));
#47267=DIRECTION('',(-0.931242779705751,0.,0.364399348580519));
#47268=DIRECTION('',(-0.781200482846105,0.,-0.624280230025758));
#47269=DIRECTION('',(0.150042296859641,0.,-0.988679578606276));
#47270=DIRECTION('',(0.931242779705752,0.,-0.364399348580517));
#47271=DIRECTION('',(0.781200482846104,0.,0.624280230025758));
#47272=DIRECTION('',(-0.150042296859647,0.,0.988679578606275));
#47273=DIRECTION('',(-0.931242779705751,0.,0.364399348580519));
#47274=DIRECTION('',(-0.781200482846105,0.,-0.624280230025758));
#47275=DIRECTION('',(0.150042296859641,0.,-0.988679578606276));
#47276=DIRECTION('',(0.931242779705752,0.,-0.364399348580517));
#47277=DIRECTION('',(0.781200482846104,0.,0.624280230025758));
#47278=DIRECTION('',(-0.150042296859647,0.,0.988679578606275));
#47279=DIRECTION('',(-0.931242779705751,0.,0.364399348580519));
#47280=DIRECTION('',(-0.781200482846105,0.,-0.624280230025758));
#47281=DIRECTION('',(0.150042296859641,0.,-0.988679578606276));
#47282=DIRECTION('',(0.931242779705752,0.,-0.364399348580517));
#47283=DIRECTION('',(0.781200482846104,0.,0.624280230025758));
#47284=DIRECTION('',(-0.150042296859647,0.,0.988679578606275));
#47285=DIRECTION('',(-0.931242779705751,0.,0.364399348580519));
#47286=DIRECTION('',(-0.781200482846105,0.,-0.624280230025758));
#47287=DIRECTION('',(0.150042296859641,0.,-0.988679578606276));
#47288=DIRECTION('',(0.931242779705752,0.,-0.364399348580517));
#47289=DIRECTION('',(0.781200482846104,0.,0.624280230025758));
#47290=DIRECTION('',(-0.150042296859647,0.,0.988679578606275));
#47291=DIRECTION('',(-0.931242779705751,0.,0.364399348580519));
#47292=DIRECTION('',(-0.781200482846105,0.,-0.624280230025758));
#47293=DIRECTION('',(0.150042296859641,0.,-0.988679578606276));
#47294=DIRECTION('',(0.931242779705752,0.,-0.364399348580517));
#47295=DIRECTION('',(0.781200482846104,0.,0.624280230025758));
#47296=DIRECTION('',(-0.150042296859647,0.,0.988679578606275));
#47297=DIRECTION('',(-0.931242779705751,0.,0.364399348580519));
#47298=DIRECTION('',(-0.781200482846105,0.,-0.624280230025758));
#47299=DIRECTION('',(0.150042296859641,0.,-0.988679578606276));
#47300=DIRECTION('',(0.931242779705752,0.,-0.364399348580517));
#47301=DIRECTION('',(0.781200482846104,0.,0.624280230025758));
#47302=DIRECTION('',(-0.150042296859647,0.,0.988679578606275));
#47303=DIRECTION('',(-0.931242779705751,0.,0.364399348580519));
#47304=DIRECTION('',(-0.781200482846105,0.,-0.624280230025758));
#47305=DIRECTION('',(0.150042296859641,0.,-0.988679578606276));
#47306=DIRECTION('',(0.931242779705752,0.,-0.364399348580517));
#47307=DIRECTION('',(0.781200482846104,0.,0.624280230025758));
#47308=DIRECTION('',(-0.150042296859647,0.,0.988679578606275));
#47309=DIRECTION('',(-0.931242779705751,0.,0.364399348580519));
#47310=DIRECTION('',(-0.781200482846105,0.,-0.624280230025758));
#47311=DIRECTION('',(0.150042296859641,0.,-0.988679578606276));
#47312=DIRECTION('',(0.931242779705752,0.,-0.364399348580517));
#47313=DIRECTION('',(0.781200482846104,0.,0.624280230025758));
#47314=DIRECTION('',(-0.150042296859647,0.,0.988679578606275));
#47315=DIRECTION('',(-0.931242779705751,0.,0.364399348580519));
#47316=DIRECTION('',(-0.781200482846105,0.,-0.624280230025758));
#47317=DIRECTION('',(0.150042296859641,0.,-0.988679578606276));
#47318=DIRECTION('',(0.931242779705752,0.,-0.364399348580517));
#47319=DIRECTION('',(0.781200482846104,0.,0.624280230025758));
#47320=DIRECTION('',(-0.150042296859647,0.,0.988679578606275));
#47321=DIRECTION('',(-0.931242779705751,0.,0.364399348580519));
#47322=DIRECTION('',(-0.781200482846105,0.,-0.624280230025758));
#47323=DIRECTION('',(0.150042296859641,0.,-0.988679578606276));
#47324=DIRECTION('',(0.931242779705752,0.,-0.364399348580517));
#47325=DIRECTION('',(0.781200482846104,0.,0.624280230025758));
#47326=DIRECTION('',(-0.150042296859647,0.,0.988679578606275));
#47327=DIRECTION('',(-0.931242779705751,0.,0.364399348580519));
#47328=DIRECTION('',(-0.781200482846105,0.,-0.624280230025758));
#47329=DIRECTION('',(0.150042296859641,0.,-0.988679578606276));
#47330=DIRECTION('',(0.931242779705752,0.,-0.364399348580517));
#47331=DIRECTION('',(0.781200482846104,0.,0.624280230025758));
#47332=DIRECTION('',(-0.150042296859647,0.,0.988679578606275));
#47333=DIRECTION('',(-0.931242779705751,0.,0.364399348580519));
#47334=DIRECTION('',(-0.781200482846105,0.,-0.624280230025758));
#47335=DIRECTION('',(0.150042296859641,0.,-0.988679578606276));
#47336=DIRECTION('',(0.931242779705752,0.,-0.364399348580517));
#47337=DIRECTION('',(0.781200482846104,0.,0.624280230025758));
#47338=DIRECTION('',(-0.150042296859647,0.,0.988679578606275));
#47339=DIRECTION('',(-0.931242779705751,0.,0.364399348580519));
#47340=DIRECTION('',(-0.781200482846105,0.,-0.624280230025758));
#47341=DIRECTION('',(0.150042296859641,0.,-0.988679578606276));
#47342=DIRECTION('',(0.931242779705752,0.,-0.364399348580517));
#47343=DIRECTION('',(0.781200482846104,0.,0.624280230025758));
#47344=DIRECTION('',(-0.150042296859647,0.,0.988679578606275));
#47345=DIRECTION('',(-0.931242779705751,0.,0.364399348580519));
#47346=DIRECTION('',(-0.781200482846105,0.,-0.624280230025758));
#47347=DIRECTION('',(0.150042296859641,0.,-0.988679578606276));
#47348=DIRECTION('',(0.931242779705752,0.,-0.364399348580517));
#47349=DIRECTION('',(0.781200482846104,0.,0.624280230025758));
#47350=DIRECTION('',(-0.150042296859647,0.,0.988679578606275));
#47351=DIRECTION('',(-0.931242779705751,0.,0.364399348580519));
#47352=DIRECTION('',(-0.781200482846105,0.,-0.624280230025758));
#47353=DIRECTION('',(0.150042296859641,0.,-0.988679578606276));
#47354=DIRECTION('',(0.931242779705752,0.,-0.364399348580517));
#47355=DIRECTION('',(0.781200482846104,0.,0.624280230025758));
#47356=DIRECTION('',(-0.150042296859647,0.,0.988679578606275));
#47357=DIRECTION('',(-0.931242779705751,0.,0.364399348580519));
#47358=DIRECTION('',(-0.781200482846105,0.,-0.624280230025758));
#47359=DIRECTION('',(0.150042296859641,0.,-0.988679578606276));
#47360=DIRECTION('',(0.931242779705752,0.,-0.364399348580517));
#47361=DIRECTION('',(0.781200482846104,0.,0.624280230025758));
#47362=DIRECTION('',(-0.150042296859647,0.,0.988679578606275));
#47363=DIRECTION('',(-0.931242779705751,0.,0.364399348580519));
#47364=DIRECTION('',(-0.781200482846105,0.,-0.624280230025758));
#47365=DIRECTION('',(0.150042296859641,0.,-0.988679578606276));
#47366=DIRECTION('',(0.931242779705752,0.,-0.364399348580517));
#47367=DIRECTION('',(0.781200482846104,0.,0.624280230025758));
#47368=DIRECTION('',(-0.150042296859647,0.,0.988679578606275));
#47369=DIRECTION('',(-0.931242779705751,0.,0.364399348580519));
#47370=DIRECTION('',(-0.781200482846105,0.,-0.624280230025758));
#47371=DIRECTION('',(0.150042296859641,0.,-0.988679578606276));
#47372=DIRECTION('',(0.931242779705752,0.,-0.364399348580517));
#47373=DIRECTION('',(0.781200482846104,0.,0.624280230025758));
#47374=DIRECTION('',(-0.150042296859647,0.,0.988679578606275));
#47375=DIRECTION('',(-0.931242779705751,0.,0.364399348580519));
#47376=DIRECTION('',(-0.781200482846105,0.,-0.624280230025758));
#47377=DIRECTION('',(0.150042296859641,0.,-0.988679578606276));
#47378=DIRECTION('',(0.931242779705752,0.,-0.364399348580517));
#47379=DIRECTION('',(0.781200482846104,0.,0.624280230025758));
#47380=DIRECTION('',(-0.150042296859647,0.,0.988679578606275));
#47381=DIRECTION('',(-0.931242779705751,0.,0.364399348580519));
#47382=DIRECTION('',(-0.781200482846105,0.,-0.624280230025758));
#47383=DIRECTION('',(0.150042296859641,0.,-0.988679578606276));
#47384=DIRECTION('',(0.931242779705752,0.,-0.364399348580517));
#47385=DIRECTION('',(0.781200482846104,0.,0.624280230025758));
#47386=DIRECTION('',(-0.150042296859647,0.,0.988679578606275));
#47387=DIRECTION('',(-0.931242779705751,0.,0.364399348580519));
#47388=DIRECTION('',(-0.781200482846105,0.,-0.624280230025758));
#47389=DIRECTION('',(0.150042296859641,0.,-0.988679578606276));
#47390=DIRECTION('',(0.931242779705752,0.,-0.364399348580517));
#47391=DIRECTION('',(0.781200482846104,0.,0.624280230025758));
#47392=DIRECTION('',(-0.150042296859647,0.,0.988679578606275));
#47393=DIRECTION('',(-0.931242779705751,0.,0.364399348580519));
#47394=DIRECTION('',(-0.781200482846105,0.,-0.624280230025758));
#47395=DIRECTION('',(0.150042296859641,0.,-0.988679578606276));
#47396=DIRECTION('',(0.931242779705752,0.,-0.364399348580517));
#47397=DIRECTION('',(0.781200482846104,0.,0.624280230025758));
#47398=DIRECTION('',(-0.150042296859647,0.,0.988679578606275));
#47399=DIRECTION('',(-0.931242779705751,0.,0.364399348580519));
#47400=DIRECTION('',(-0.781200482846105,0.,-0.624280230025758));
#47401=DIRECTION('',(0.150042296859641,0.,-0.988679578606276));
#47402=DIRECTION('',(0.931242779705752,0.,-0.364399348580517));
#47403=DIRECTION('',(0.781200482846104,0.,0.624280230025758));
#47404=DIRECTION('',(-0.150042296859647,0.,0.988679578606275));
#47405=DIRECTION('',(-0.931242779705751,0.,0.364399348580519));
#47406=DIRECTION('',(-0.781200482846105,0.,-0.624280230025758));
#47407=DIRECTION('',(0.150042296859641,0.,-0.988679578606276));
#47408=DIRECTION('',(0.931242779705752,0.,-0.364399348580517));
#47409=DIRECTION('',(0.781200482846104,0.,0.624280230025758));
#47410=DIRECTION('',(-0.150042296859647,0.,0.988679578606275));
#47411=DIRECTION('',(-0.931242779705751,0.,0.364399348580519));
#47412=DIRECTION('',(-0.781200482846105,0.,-0.624280230025758));
#47413=DIRECTION('',(0.150042296859641,0.,-0.988679578606276));
#47414=DIRECTION('',(0.931242779705752,0.,-0.364399348580517));
#47415=DIRECTION('',(0.781200482846104,0.,0.624280230025758));
#47416=DIRECTION('',(-0.150042296859647,0.,0.988679578606275));
#47417=DIRECTION('',(-0.931242779705751,0.,0.364399348580519));
#47418=DIRECTION('',(-0.781200482846105,0.,-0.624280230025758));
#47419=DIRECTION('',(0.150042296859641,0.,-0.988679578606276));
#47420=DIRECTION('',(0.931242779705752,0.,-0.364399348580517));
#47421=DIRECTION('',(0.781200482846104,0.,0.624280230025758));
#47422=DIRECTION('',(-0.150042296859647,0.,0.988679578606275));
#47423=DIRECTION('',(-0.931242779705751,0.,0.364399348580519));
#47424=DIRECTION('',(-0.781200482846105,0.,-0.624280230025758));
#47425=DIRECTION('',(0.150042296859641,0.,-0.988679578606276));
#47426=DIRECTION('',(0.931242779705752,0.,-0.364399348580517));
#47427=DIRECTION('',(0.781200482846104,0.,0.624280230025758));
#47428=DIRECTION('',(-0.150042296859647,0.,0.988679578606275));
#47429=DIRECTION('',(-0.931242779705751,0.,0.364399348580519));
#47430=DIRECTION('',(-0.781200482846105,0.,-0.624280230025758));
#47431=DIRECTION('',(0.150042296859641,0.,-0.988679578606276));
#47432=DIRECTION('',(0.931242779705752,0.,-0.364399348580517));
#47433=DIRECTION('',(0.781200482846104,0.,0.624280230025758));
#47434=DIRECTION('',(-0.150042296859647,0.,0.988679578606275));
#47435=DIRECTION('',(-0.931242779705751,0.,0.364399348580519));
#47436=DIRECTION('',(-0.781200482846105,0.,-0.624280230025758));
#47437=DIRECTION('',(0.150042296859641,0.,-0.988679578606276));
#47438=DIRECTION('',(0.931242779705752,0.,-0.364399348580517));
#47439=DIRECTION('',(0.781200482846104,0.,0.624280230025758));
#47440=DIRECTION('',(-0.150042296859647,0.,0.988679578606275));
#47441=DIRECTION('',(-0.931242779705751,0.,0.364399348580519));
#47442=DIRECTION('',(-0.781200482846105,0.,-0.624280230025758));
#47443=DIRECTION('',(0.150042296859641,0.,-0.988679578606276));
#47444=DIRECTION('',(0.931242779705752,0.,-0.364399348580517));
#47445=DIRECTION('',(0.781200482846104,0.,0.624280230025758));
#47446=DIRECTION('',(-0.150042296859647,0.,0.988679578606275));
#47447=DIRECTION('',(-0.931242779705751,0.,0.364399348580519));
#47448=DIRECTION('',(-0.781200482846105,0.,-0.624280230025758));
#47449=DIRECTION('',(0.150042296859641,0.,-0.988679578606276));
#47450=DIRECTION('',(0.931242779705752,0.,-0.364399348580517));
#47451=DIRECTION('',(0.781200482846104,0.,0.624280230025758));
#47452=DIRECTION('',(-0.150042296859647,0.,0.988679578606275));
#47453=DIRECTION('',(-0.931242779705751,0.,0.364399348580519));
#47454=DIRECTION('',(-0.781200482846105,0.,-0.624280230025758));
#47455=DIRECTION('',(0.150042296859641,0.,-0.988679578606276));
#47456=DIRECTION('',(0.931242779705752,0.,-0.364399348580517));
#47457=DIRECTION('',(0.781200482846104,0.,0.624280230025758));
#47458=DIRECTION('',(-0.150042296859647,0.,0.988679578606275));
#47459=DIRECTION('',(-0.931242779705751,0.,0.364399348580519));
#47460=DIRECTION('',(-0.781200482846105,0.,-0.624280230025758));
#47461=DIRECTION('',(0.150042296859641,0.,-0.988679578606276));
#47462=DIRECTION('',(0.931242779705752,0.,-0.364399348580517));
#47463=DIRECTION('',(0.781200482846104,0.,0.624280230025758));
#47464=DIRECTION('',(-0.150042296859647,0.,0.988679578606275));
#47465=DIRECTION('',(-0.931242779705751,0.,0.364399348580519));
#47466=DIRECTION('',(-0.781200482846105,0.,-0.624280230025758));
#47467=DIRECTION('',(0.150042296859641,0.,-0.988679578606276));
#47468=DIRECTION('',(0.931242779705752,0.,-0.364399348580517));
#47469=DIRECTION('',(0.781200482846104,0.,0.624280230025758));
#47470=DIRECTION('',(-0.150042296859647,0.,0.988679578606275));
#47471=DIRECTION('',(-0.931242779705751,0.,0.364399348580519));
#47472=DIRECTION('',(-0.781200482846105,0.,-0.624280230025758));
#47473=DIRECTION('',(0.150042296859641,0.,-0.988679578606276));
#47474=DIRECTION('',(0.931242779705752,0.,-0.364399348580517));
#47475=DIRECTION('',(0.781200482846104,0.,0.624280230025758));
#47476=DIRECTION('',(-0.150042296859647,0.,0.988679578606275));
#47477=DIRECTION('',(-0.931242779705751,0.,0.364399348580519));
#47478=DIRECTION('',(-0.781200482846105,0.,-0.624280230025758));
#47479=DIRECTION('',(0.150042296859641,0.,-0.988679578606276));
#47480=DIRECTION('',(0.931242779705752,0.,-0.364399348580517));
#47481=DIRECTION('',(0.781200482846104,0.,0.624280230025758));
#47482=DIRECTION('',(-0.150042296859647,0.,0.988679578606275));
#47483=DIRECTION('',(-0.931242779705751,0.,0.364399348580519));
#47484=DIRECTION('',(-0.781200482846105,0.,-0.624280230025758));
#47485=DIRECTION('',(0.150042296859641,0.,-0.988679578606276));
#47486=DIRECTION('',(0.931242779705752,0.,-0.364399348580517));
#47487=DIRECTION('',(0.781200482846104,0.,0.624280230025758));
#47488=DIRECTION('',(-0.150042296859647,0.,0.988679578606275));
#47489=DIRECTION('',(-0.931242779705751,0.,0.364399348580519));
#47490=DIRECTION('',(-0.781200482846105,0.,-0.624280230025758));
#47491=DIRECTION('',(0.150042296859641,0.,-0.988679578606276));
#47492=DIRECTION('',(0.931242779705752,0.,-0.364399348580517));
#47493=DIRECTION('',(0.781200482846104,0.,0.624280230025758));
#47494=DIRECTION('',(-0.150042296859647,0.,0.988679578606275));
#47495=DIRECTION('',(-0.931242779705751,0.,0.364399348580519));
#47496=DIRECTION('',(-0.781200482846105,0.,-0.624280230025758));
#47497=DIRECTION('',(0.150042296859641,0.,-0.988679578606276));
#47498=DIRECTION('',(0.931242779705752,0.,-0.364399348580517));
#47499=DIRECTION('',(0.781200482846104,0.,0.624280230025758));
#47500=DIRECTION('',(-0.150042296859647,0.,0.988679578606275));
#47501=DIRECTION('',(-0.931242779705751,0.,0.364399348580519));
#47502=DIRECTION('',(-0.781200482846105,0.,-0.624280230025758));
#47503=DIRECTION('',(0.150042296859641,0.,-0.988679578606276));
#47504=DIRECTION('',(0.931242779705752,0.,-0.364399348580517));
#47505=DIRECTION('',(0.781200482846104,0.,0.624280230025758));
#47506=DIRECTION('',(-0.150042296859647,0.,0.988679578606275));
#47507=DIRECTION('',(-0.931242779705751,0.,0.364399348580519));
#47508=DIRECTION('',(-0.781200482846105,0.,-0.624280230025758));
#47509=DIRECTION('',(0.150042296859641,0.,-0.988679578606276));
#47510=DIRECTION('',(0.931242779705752,0.,-0.364399348580517));
#47511=DIRECTION('',(0.781200482846104,0.,0.624280230025758));
#47512=DIRECTION('',(-0.150042296859647,0.,0.988679578606275));
#47513=DIRECTION('',(-0.931242779705751,0.,0.364399348580519));
#47514=DIRECTION('',(-0.781200482846105,0.,-0.624280230025758));
#47515=DIRECTION('',(0.150042296859641,0.,-0.988679578606276));
#47516=DIRECTION('',(0.931242779705752,0.,-0.364399348580517));
#47517=DIRECTION('',(0.781200482846104,0.,0.624280230025758));
#47518=DIRECTION('',(-0.150042296859647,0.,0.988679578606275));
#47519=DIRECTION('',(-0.931242779705751,0.,0.364399348580519));
#47520=DIRECTION('',(-0.781200482846105,0.,-0.624280230025758));
#47521=DIRECTION('',(0.150042296859641,0.,-0.988679578606276));
#47522=DIRECTION('',(0.931242779705752,0.,-0.364399348580517));
#47523=DIRECTION('',(0.781200482846104,0.,0.624280230025758));
#47524=DIRECTION('',(-0.150042296859647,0.,0.988679578606275));
#47525=DIRECTION('',(-0.931242779705751,0.,0.364399348580519));
#47526=DIRECTION('',(-0.781200482846105,0.,-0.624280230025758));
#47527=DIRECTION('',(0.150042296859641,0.,-0.988679578606276));
#47528=DIRECTION('',(0.931242779705752,0.,-0.364399348580517));
#47529=DIRECTION('',(0.781200482846104,0.,0.624280230025758));
#47530=DIRECTION('',(-0.150042296859647,0.,0.988679578606275));
#47531=DIRECTION('',(-0.931242779705751,0.,0.364399348580519));
#47532=DIRECTION('',(-0.781200482846105,0.,-0.624280230025758));
#47533=DIRECTION('',(0.150042296859641,0.,-0.988679578606276));
#47534=DIRECTION('',(0.931242779705752,0.,-0.364399348580517));
#47535=DIRECTION('',(0.781200482846104,0.,0.624280230025758));
#47536=DIRECTION('',(-0.150042296859647,0.,0.988679578606275));
#47537=DIRECTION('',(-0.931242779705751,0.,0.364399348580519));
#47538=DIRECTION('',(-0.781200482846105,0.,-0.624280230025758));
#47539=DIRECTION('',(0.150042296859641,0.,-0.988679578606276));
#47540=DIRECTION('',(0.931242779705752,0.,-0.364399348580517));
#47541=DIRECTION('',(0.781200482846104,0.,0.624280230025758));
#47542=DIRECTION('',(-0.150042296859647,0.,0.988679578606275));
#47543=DIRECTION('',(-0.931242779705751,0.,0.364399348580519));
#47544=DIRECTION('',(-0.781200482846105,0.,-0.624280230025758));
#47545=DIRECTION('',(0.150042296859641,0.,-0.988679578606276));
#47546=DIRECTION('',(0.931242779705752,0.,-0.364399348580517));
#47547=DIRECTION('',(0.781200482846104,0.,0.624280230025758));
#47548=DIRECTION('',(-0.150042296859647,0.,0.988679578606275));
#47549=DIRECTION('',(-0.931242779705751,0.,0.364399348580519));
#47550=DIRECTION('',(-0.781200482846105,0.,-0.624280230025758));
#47551=DIRECTION('',(0.150042296859641,0.,-0.988679578606276));
#47552=DIRECTION('',(0.931242779705752,0.,-0.364399348580517));
#47553=DIRECTION('',(0.781200482846104,0.,0.624280230025758));
#47554=DIRECTION('',(-0.150042296859647,0.,0.988679578606275));
#47555=DIRECTION('',(-0.931242779705751,0.,0.364399348580519));
#47556=DIRECTION('',(-0.781200482846105,0.,-0.624280230025758));
#47557=DIRECTION('',(0.150042296859641,0.,-0.988679578606276));
#47558=DIRECTION('',(0.931242779705752,0.,-0.364399348580517));
#47559=DIRECTION('',(0.781200482846104,0.,0.624280230025758));
#47560=DIRECTION('',(-0.150042296859647,0.,0.988679578606275));
#47561=DIRECTION('',(-0.931242779705751,0.,0.364399348580519));
#47562=DIRECTION('',(-0.781200482846105,0.,-0.624280230025758));
#47563=DIRECTION('',(0.150042296859641,0.,-0.988679578606276));
#47564=DIRECTION('',(0.931242779705752,0.,-0.364399348580517));
#47565=DIRECTION('',(0.781200482846104,0.,0.624280230025758));
#47566=DIRECTION('',(-0.150042296859647,0.,0.988679578606275));
#47567=DIRECTION('',(-0.931242779705751,0.,0.364399348580519));
#47568=DIRECTION('',(-0.781200482846105,0.,-0.624280230025758));
#47569=DIRECTION('',(0.150042296859641,0.,-0.988679578606276));
#47570=DIRECTION('',(0.931242779705752,0.,-0.364399348580517));
#47571=DIRECTION('',(0.781200482846104,0.,0.624280230025758));
#47572=DIRECTION('',(-0.150042296859647,0.,0.988679578606275));
#47573=DIRECTION('',(-0.931242779705751,0.,0.364399348580519));
#47574=DIRECTION('',(-0.781200482846105,0.,-0.624280230025758));
#47575=DIRECTION('',(0.150042296859641,0.,-0.988679578606276));
#47576=DIRECTION('',(0.931242779705752,0.,-0.364399348580517));
#47577=DIRECTION('',(0.781200482846104,0.,0.624280230025758));
#47578=DIRECTION('',(-0.150042296859647,0.,0.988679578606275));
#47579=DIRECTION('',(-0.931242779705751,0.,0.364399348580519));
#47580=DIRECTION('',(-0.781200482846105,0.,-0.624280230025758));
#47581=DIRECTION('',(0.150042296859641,0.,-0.988679578606276));
#47582=DIRECTION('',(0.931242779705752,0.,-0.364399348580517));
#47583=DIRECTION('',(0.781200482846104,0.,0.624280230025758));
#47584=DIRECTION('',(-0.150042296859647,0.,0.988679578606275));
#47585=DIRECTION('',(-0.931242779705751,0.,0.364399348580519));
#47586=DIRECTION('',(-0.781200482846105,0.,-0.624280230025758));
#47587=DIRECTION('',(0.150042296859641,0.,-0.988679578606276));
#47588=DIRECTION('',(0.931242779705752,0.,-0.364399348580517));
#47589=DIRECTION('',(0.781200482846104,0.,0.624280230025758));
#47590=DIRECTION('',(-0.150042296859647,0.,0.988679578606275));
#47591=DIRECTION('',(-0.931242779705751,0.,0.364399348580519));
#47592=DIRECTION('',(-0.781200482846105,0.,-0.624280230025758));
#47593=DIRECTION('',(0.150042296859641,0.,-0.988679578606276));
#47594=DIRECTION('',(0.931242779705752,0.,-0.364399348580517));
#47595=DIRECTION('',(0.781200482846104,0.,0.624280230025758));
#47596=DIRECTION('',(-0.150042296859647,0.,0.988679578606275));
#47597=DIRECTION('',(-0.931242779705751,0.,0.364399348580519));
#47598=DIRECTION('',(-0.781200482846105,0.,-0.624280230025758));
#47599=DIRECTION('',(0.150042296859641,0.,-0.988679578606276));
#47600=DIRECTION('',(0.931242779705752,0.,-0.364399348580517));
#47601=DIRECTION('',(0.781200482846104,0.,0.624280230025758));
#47602=DIRECTION('',(-0.150042296859647,0.,0.988679578606275));
#47603=DIRECTION('',(-0.931242779705751,0.,0.364399348580519));
#47604=DIRECTION('',(-0.781200482846105,0.,-0.624280230025758));
#47605=DIRECTION('',(0.150042296859641,0.,-0.988679578606276));
#47606=DIRECTION('',(0.931242779705752,0.,-0.364399348580517));
#47607=DIRECTION('',(0.781200482846104,0.,0.624280230025758));
#47608=DIRECTION('',(-0.150042296859647,0.,0.988679578606275));
#47609=DIRECTION('',(-0.931242779705751,0.,0.364399348580519));
#47610=DIRECTION('',(-0.781200482846105,0.,-0.624280230025758));
#47611=DIRECTION('',(0.150042296859641,0.,-0.988679578606276));
#47612=DIRECTION('',(0.931242779705752,0.,-0.364399348580517));
#47613=DIRECTION('',(0.781200482846104,0.,0.624280230025758));
#47614=DIRECTION('',(-0.150042296859647,0.,0.988679578606275));
#47615=DIRECTION('',(-0.931242779705751,0.,0.364399348580519));
#47616=DIRECTION('',(-0.781200482846105,0.,-0.624280230025758));
#47617=DIRECTION('',(0.150042296859641,0.,-0.988679578606276));
#47618=DIRECTION('',(0.931242779705752,0.,-0.364399348580517));
#47619=DIRECTION('',(0.781200482846104,0.,0.624280230025758));
#47620=DIRECTION('',(-0.150042296859647,0.,0.988679578606275));
#47621=DIRECTION('',(-0.931242779705751,0.,0.364399348580519));
#47622=DIRECTION('',(-0.781200482846105,0.,-0.624280230025758));
#47623=DIRECTION('',(0.150042296859641,0.,-0.988679578606276));
#47624=DIRECTION('',(0.931242779705752,0.,-0.364399348580517));
#47625=DIRECTION('',(0.781200482846104,0.,0.624280230025758));
#47626=DIRECTION('',(-0.150042296859647,0.,0.988679578606275));
#47627=DIRECTION('',(-0.931242779705751,0.,0.364399348580519));
#47628=DIRECTION('',(-0.781200482846105,0.,-0.624280230025758));
#47629=DIRECTION('',(0.150042296859641,0.,-0.988679578606276));
#47630=DIRECTION('',(0.931242779705752,0.,-0.364399348580517));
#47631=DIRECTION('',(0.781200482846104,0.,0.624280230025758));
#47632=DIRECTION('',(-0.150042296859647,0.,0.988679578606275));
#47633=DIRECTION('',(-0.931242779705751,0.,0.364399348580519));
#47634=DIRECTION('',(-0.781200482846105,0.,-0.624280230025758));
#47635=DIRECTION('',(0.150042296859641,0.,-0.988679578606276));
#47636=DIRECTION('',(0.931242779705752,0.,-0.364399348580517));
#47637=DIRECTION('',(0.781200482846104,0.,0.624280230025758));
#47638=DIRECTION('',(-0.150042296859647,0.,0.988679578606275));
#47639=DIRECTION('',(-0.931242779705751,0.,0.364399348580519));
#47640=DIRECTION('',(-0.781200482846105,0.,-0.624280230025758));
#47641=DIRECTION('',(0.150042296859641,0.,-0.988679578606276));
#47642=DIRECTION('',(0.931242779705752,0.,-0.364399348580517));
#47643=DIRECTION('',(0.781200482846104,0.,0.624280230025758));
#47644=DIRECTION('',(-0.150042296859647,0.,0.988679578606275));
#47645=DIRECTION('',(-0.931242779705751,0.,0.364399348580519));
#47646=DIRECTION('',(-0.781200482846105,0.,-0.624280230025758));
#47647=DIRECTION('',(0.150042296859641,0.,-0.988679578606276));
#47648=DIRECTION('',(0.931242779705752,0.,-0.364399348580517));
#47649=DIRECTION('',(0.781200482846104,0.,0.624280230025758));
#47650=DIRECTION('',(-0.150042296859647,0.,0.988679578606275));
#47651=DIRECTION('',(-0.931242779705751,0.,0.364399348580519));
#47652=DIRECTION('',(-0.781200482846105,0.,-0.624280230025758));
#47653=DIRECTION('',(0.150042296859641,0.,-0.988679578606276));
#47654=DIRECTION('',(0.931242779705752,0.,-0.364399348580517));
#47655=DIRECTION('',(0.781200482846104,0.,0.624280230025758));
#47656=DIRECTION('',(-0.150042296859647,0.,0.988679578606275));
#47657=DIRECTION('',(-0.931242779705751,0.,0.364399348580519));
#47658=DIRECTION('',(-0.781200482846105,0.,-0.624280230025758));
#47659=DIRECTION('',(0.150042296859641,0.,-0.988679578606276));
#47660=DIRECTION('',(0.931242779705752,0.,-0.364399348580517));
#47661=DIRECTION('',(0.781200482846104,0.,0.624280230025758));
#47662=DIRECTION('',(-0.150042296859647,0.,0.988679578606275));
#47663=DIRECTION('',(-0.931242779705751,0.,0.364399348580519));
#47664=DIRECTION('',(-0.781200482846105,0.,-0.624280230025758));
#47665=DIRECTION('',(0.150042296859641,0.,-0.988679578606276));
#47666=DIRECTION('',(0.931242779705752,0.,-0.364399348580517));
#47667=DIRECTION('',(0.781200482846104,0.,0.624280230025758));
#47668=DIRECTION('',(-0.150042296859647,0.,0.988679578606275));
#47669=DIRECTION('',(-0.931242779705751,0.,0.364399348580519));
#47670=DIRECTION('',(-0.781200482846105,0.,-0.624280230025758));
#47671=DIRECTION('',(0.150042296859641,0.,-0.988679578606276));
#47672=DIRECTION('',(0.931242779705752,0.,-0.364399348580517));
#47673=DIRECTION('',(0.781200482846104,0.,0.624280230025758));
#47674=DIRECTION('',(-0.150042296859647,0.,0.988679578606275));
#47675=DIRECTION('',(-0.931242779705751,0.,0.364399348580519));
#47676=DIRECTION('',(-0.781200482846105,0.,-0.624280230025758));
#47677=DIRECTION('',(0.150042296859641,0.,-0.988679578606276));
#47678=DIRECTION('',(0.931242779705752,0.,-0.364399348580517));
#47679=DIRECTION('',(0.781200482846104,0.,0.624280230025758));
#47680=DIRECTION('',(-0.150042296859647,0.,0.988679578606275));
#47681=DIRECTION('',(-0.931242779705751,0.,0.364399348580519));
#47682=DIRECTION('',(-0.781200482846105,0.,-0.624280230025758));
#47683=DIRECTION('',(0.150042296859641,0.,-0.988679578606276));
#47684=DIRECTION('',(0.931242779705752,0.,-0.364399348580517));
#47685=DIRECTION('',(0.781200482846104,0.,0.624280230025758));
#47686=DIRECTION('',(-0.150042296859647,0.,0.988679578606275));
#47687=DIRECTION('',(-0.931242779705751,0.,0.364399348580519));
#47688=DIRECTION('',(-0.781200482846105,0.,-0.624280230025758));
#47689=DIRECTION('',(0.150042296859641,0.,-0.988679578606276));
#47690=DIRECTION('',(0.931242779705752,0.,-0.364399348580517));
#47691=DIRECTION('',(0.781200482846104,0.,0.624280230025758));
#47692=DIRECTION('',(-0.150042296859647,0.,0.988679578606275));
#47693=DIRECTION('',(-0.931242779705751,0.,0.364399348580519));
#47694=DIRECTION('',(-0.781200482846105,0.,-0.624280230025758));
#47695=DIRECTION('',(0.150042296859641,0.,-0.988679578606276));
#47696=DIRECTION('',(0.931242779705752,0.,-0.364399348580517));
#47697=DIRECTION('',(0.781200482846104,0.,0.624280230025758));
#47698=DIRECTION('',(-0.150042296859647,0.,0.988679578606275));
#47699=DIRECTION('',(-0.931242779705751,0.,0.364399348580519));
#47700=DIRECTION('',(-0.781200482846105,0.,-0.624280230025758));
#47701=DIRECTION('',(0.150042296859641,0.,-0.988679578606276));
#47702=DIRECTION('',(0.931242779705752,0.,-0.364399348580517));
#47703=DIRECTION('',(0.781200482846104,0.,0.624280230025758));
#47704=DIRECTION('',(-0.150042296859647,0.,0.988679578606275));
#47705=DIRECTION('',(-0.931242779705751,0.,0.364399348580519));
#47706=DIRECTION('',(-0.781200482846105,0.,-0.624280230025758));
#47707=DIRECTION('',(0.150042296859641,0.,-0.988679578606276));
#47708=DIRECTION('',(0.931242779705752,0.,-0.364399348580517));
#47709=DIRECTION('',(0.781200482846104,0.,0.624280230025758));
#47710=DIRECTION('',(-0.150042296859647,0.,0.988679578606275));
#47711=DIRECTION('',(-0.931242779705751,0.,0.364399348580519));
#47712=DIRECTION('',(-0.781200482846105,0.,-0.624280230025758));
#47713=DIRECTION('',(0.150042296859641,0.,-0.988679578606276));
#47714=DIRECTION('',(0.931242779705752,0.,-0.364399348580517));
#47715=DIRECTION('',(0.781200482846104,0.,0.624280230025758));
#47716=DIRECTION('',(-0.150042296859647,0.,0.988679578606275));
#47717=DIRECTION('',(-0.931242779705751,0.,0.364399348580519));
#47718=DIRECTION('',(-0.781200482846105,0.,-0.624280230025758));
#47719=DIRECTION('',(0.150042296859641,0.,-0.988679578606276));
#47720=DIRECTION('',(0.931242779705752,0.,-0.364399348580517));
#47721=DIRECTION('',(0.781200482846104,0.,0.624280230025758));
#47722=DIRECTION('',(-0.150042296859647,0.,0.988679578606275));
#47723=DIRECTION('',(-0.931242779705751,0.,0.364399348580519));
#47724=DIRECTION('',(-0.781200482846105,0.,-0.624280230025758));
#47725=DIRECTION('',(0.150042296859641,0.,-0.988679578606276));
#47726=DIRECTION('',(0.931242779705752,0.,-0.364399348580517));
#47727=DIRECTION('',(0.781200482846104,0.,0.624280230025758));
#47728=DIRECTION('',(-0.150042296859647,0.,0.988679578606275));
#47729=DIRECTION('',(-0.931242779705751,0.,0.364399348580519));
#47730=DIRECTION('',(-0.781200482846105,0.,-0.624280230025758));
#47731=DIRECTION('',(0.150042296859641,0.,-0.988679578606276));
#47732=DIRECTION('',(0.931242779705752,0.,-0.364399348580517));
#47733=DIRECTION('',(0.781200482846104,0.,0.624280230025758));
#47734=DIRECTION('',(-0.150042296859647,0.,0.988679578606275));
#47735=DIRECTION('',(-0.931242779705751,0.,0.364399348580519));
#47736=DIRECTION('',(-0.781200482846105,0.,-0.624280230025758));
#47737=DIRECTION('',(0.150042296859641,0.,-0.988679578606276));
#47738=DIRECTION('',(0.931242779705752,0.,-0.364399348580517));
#47739=DIRECTION('',(0.781200482846104,0.,0.624280230025758));
#47740=DIRECTION('',(-0.150042296859647,0.,0.988679578606275));
#47741=DIRECTION('',(-0.931242779705751,0.,0.364399348580519));
#47742=DIRECTION('',(-0.781200482846105,0.,-0.624280230025758));
#47743=DIRECTION('',(0.150042296859641,0.,-0.988679578606276));
#47744=DIRECTION('',(0.931242779705752,0.,-0.364399348580517));
#47745=DIRECTION('',(0.781200482846104,0.,0.624280230025758));
#47746=DIRECTION('',(-0.150042296859647,0.,0.988679578606275));
#47747=DIRECTION('',(-0.931242779705751,0.,0.364399348580519));
#47748=DIRECTION('',(-0.781200482846105,0.,-0.624280230025758));
#47749=DIRECTION('',(0.150042296859641,0.,-0.988679578606276));
#47750=DIRECTION('',(0.931242779705752,0.,-0.364399348580517));
#47751=DIRECTION('',(0.781200482846104,0.,0.624280230025758));
#47752=DIRECTION('',(-0.150042296859647,0.,0.988679578606275));
#47753=DIRECTION('',(-0.931242779705751,0.,0.364399348580519));
#47754=DIRECTION('',(-0.781200482846105,0.,-0.624280230025758));
#47755=DIRECTION('',(0.150042296859641,0.,-0.988679578606276));
#47756=DIRECTION('',(0.931242779705752,0.,-0.364399348580517));
#47757=DIRECTION('',(0.781200482846104,0.,0.624280230025758));
#47758=DIRECTION('',(-0.150042296859647,0.,0.988679578606275));
#47759=DIRECTION('',(-0.931242779705751,0.,0.364399348580519));
#47760=DIRECTION('',(-0.781200482846105,0.,-0.624280230025758));
#47761=DIRECTION('',(0.150042296859641,0.,-0.988679578606276));
#47762=DIRECTION('',(0.931242779705752,0.,-0.364399348580517));
#47763=DIRECTION('',(0.781200482846104,0.,0.624280230025758));
#47764=DIRECTION('',(-0.150042296859647,0.,0.988679578606275));
#47765=DIRECTION('',(-0.931242779705751,0.,0.364399348580519));
#47766=DIRECTION('',(-0.781200482846105,0.,-0.624280230025758));
#47767=DIRECTION('',(0.150042296859641,0.,-0.988679578606276));
#47768=DIRECTION('',(0.931242779705752,0.,-0.364399348580517));
#47769=DIRECTION('',(0.781200482846104,0.,0.624280230025758));
#47770=DIRECTION('',(-0.150042296859647,0.,0.988679578606275));
#47771=DIRECTION('',(-0.931242779705751,0.,0.364399348580519));
#47772=DIRECTION('',(-0.781200482846105,0.,-0.624280230025758));
#47773=DIRECTION('',(0.150042296859641,0.,-0.988679578606276));
#47774=DIRECTION('',(0.931242779705752,0.,-0.364399348580517));
#47775=DIRECTION('',(0.781200482846104,0.,0.624280230025758));
#47776=DIRECTION('',(-0.150042296859647,0.,0.988679578606275));
#47777=DIRECTION('',(-0.931242779705751,0.,0.364399348580519));
#47778=DIRECTION('',(-0.781200482846105,0.,-0.624280230025758));
#47779=DIRECTION('',(0.150042296859641,0.,-0.988679578606276));
#47780=DIRECTION('',(0.931242779705752,0.,-0.364399348580517));
#47781=DIRECTION('',(0.781200482846104,0.,0.624280230025758));
#47782=DIRECTION('',(-0.150042296859647,0.,0.988679578606275));
#47783=DIRECTION('',(-0.931242779705751,0.,0.364399348580519));
#47784=DIRECTION('',(-0.781200482846105,0.,-0.624280230025758));
#47785=DIRECTION('',(0.150042296859641,0.,-0.988679578606276));
#47786=DIRECTION('',(0.931242779705752,0.,-0.364399348580517));
#47787=DIRECTION('',(0.781200482846104,0.,0.624280230025758));
#47788=DIRECTION('',(-0.150042296859647,0.,0.988679578606275));
#47789=DIRECTION('',(-0.931242779705751,0.,0.364399348580519));
#47790=DIRECTION('',(-0.781200482846105,0.,-0.624280230025758));
#47791=DIRECTION('',(0.150042296859641,0.,-0.988679578606276));
#47792=DIRECTION('',(0.931242779705752,0.,-0.364399348580517));
#47793=DIRECTION('',(0.781200482846104,0.,0.624280230025758));
#47794=DIRECTION('',(-0.150042296859647,0.,0.988679578606275));
#47795=DIRECTION('',(-0.931242779705751,0.,0.364399348580519));
#47796=DIRECTION('',(-0.781200482846105,0.,-0.624280230025758));
#47797=DIRECTION('',(0.150042296859641,0.,-0.988679578606276));
#47798=DIRECTION('',(0.931242779705752,0.,-0.364399348580517));
#47799=DIRECTION('',(0.781200482846104,0.,0.624280230025758));
#47800=DIRECTION('',(-0.150042296859647,0.,0.988679578606275));
#47801=DIRECTION('',(-0.931242779705751,0.,0.364399348580519));
#47802=DIRECTION('',(-0.781200482846105,0.,-0.624280230025758));
#47803=DIRECTION('',(0.150042296859641,0.,-0.988679578606276));
#47804=DIRECTION('',(0.931242779705752,0.,-0.364399348580517));
#47805=DIRECTION('',(0.781200482846104,0.,0.624280230025758));
#47806=DIRECTION('',(-0.150042296859647,0.,0.988679578606275));
#47807=DIRECTION('',(-0.931242779705751,0.,0.364399348580519));
#47808=DIRECTION('',(-0.781200482846105,0.,-0.624280230025758));
#47809=DIRECTION('',(0.150042296859641,0.,-0.988679578606276));
#47810=DIRECTION('',(0.931242779705752,0.,-0.364399348580517));
#47811=DIRECTION('',(0.781200482846104,0.,0.624280230025758));
#47812=DIRECTION('',(-0.150042296859647,0.,0.988679578606275));
#47813=DIRECTION('',(-0.931242779705751,0.,0.364399348580519));
#47814=DIRECTION('',(-0.781200482846105,0.,-0.624280230025758));
#47815=DIRECTION('',(0.150042296859641,0.,-0.988679578606276));
#47816=DIRECTION('',(0.931242779705752,0.,-0.364399348580517));
#47817=DIRECTION('',(0.781200482846104,0.,0.624280230025758));
#47818=DIRECTION('',(-0.150042296859647,0.,0.988679578606275));
#47819=DIRECTION('',(-0.931242779705751,0.,0.364399348580519));
#47820=DIRECTION('',(-0.781200482846105,0.,-0.624280230025758));
#47821=DIRECTION('',(0.150042296859641,0.,-0.988679578606276));
#47822=DIRECTION('',(0.931242779705752,0.,-0.364399348580517));
#47823=DIRECTION('',(0.781200482846104,0.,0.624280230025758));
#47824=DIRECTION('',(-0.150042296859647,0.,0.988679578606275));
#47825=DIRECTION('',(-0.931242779705751,0.,0.364399348580519));
#47826=DIRECTION('',(-0.781200482846105,0.,-0.624280230025758));
#47827=DIRECTION('',(0.150042296859641,0.,-0.988679578606276));
#47828=DIRECTION('',(0.931242779705752,0.,-0.364399348580517));
#47829=DIRECTION('',(0.781200482846104,0.,0.624280230025758));
#47830=DIRECTION('',(-0.150042296859647,0.,0.988679578606275));
#47831=DIRECTION('',(-0.931242779705751,0.,0.364399348580519));
#47832=DIRECTION('',(-0.781200482846105,0.,-0.624280230025758));
#47833=DIRECTION('',(0.150042296859641,0.,-0.988679578606276));
#47834=DIRECTION('',(0.931242779705752,0.,-0.364399348580517));
#47835=DIRECTION('',(0.781200482846104,0.,0.624280230025758));
#47836=DIRECTION('',(-0.150042296859647,0.,0.988679578606275));
#47837=DIRECTION('',(-0.931242779705751,0.,0.364399348580519));
#47838=DIRECTION('',(-0.781200482846105,0.,-0.624280230025758));
#47839=DIRECTION('',(0.150042296859641,0.,-0.988679578606276));
#47840=DIRECTION('',(0.931242779705752,0.,-0.364399348580517));
#47841=DIRECTION('',(0.781200482846104,0.,0.624280230025758));
#47842=DIRECTION('',(-0.150042296859647,0.,0.988679578606275));
#47843=DIRECTION('',(-0.931242779705751,0.,0.364399348580519));
#47844=DIRECTION('',(-0.781200482846105,0.,-0.624280230025758));
#47845=DIRECTION('',(0.150042296859641,0.,-0.988679578606276));
#47846=DIRECTION('',(0.931242779705752,0.,-0.364399348580517));
#47847=DIRECTION('',(0.781200482846104,0.,0.624280230025758));
#47848=DIRECTION('',(-0.150042296859647,0.,0.988679578606275));
#47849=DIRECTION('',(-0.931242779705751,0.,0.364399348580519));
#47850=DIRECTION('',(-0.781200482846105,0.,-0.624280230025758));
#47851=DIRECTION('',(0.150042296859641,0.,-0.988679578606276));
#47852=DIRECTION('',(0.931242779705752,0.,-0.364399348580517));
#47853=DIRECTION('',(0.781200482846104,0.,0.624280230025758));
#47854=DIRECTION('',(-0.150042296859647,0.,0.988679578606275));
#47855=DIRECTION('',(-0.931242779705751,0.,0.364399348580519));
#47856=DIRECTION('',(-0.781200482846105,0.,-0.624280230025758));
#47857=DIRECTION('',(0.150042296859641,0.,-0.988679578606276));
#47858=DIRECTION('',(0.931242779705752,0.,-0.364399348580517));
#47859=DIRECTION('',(0.781200482846104,0.,0.624280230025758));
#47860=DIRECTION('',(-0.150042296859647,0.,0.988679578606275));
#47861=DIRECTION('',(-0.931242779705751,0.,0.364399348580519));
#47862=DIRECTION('',(-0.781200482846105,0.,-0.624280230025758));
#47863=DIRECTION('',(0.150042296859641,0.,-0.988679578606276));
#47864=DIRECTION('',(0.931242779705752,0.,-0.364399348580517));
#47865=DIRECTION('',(0.781200482846104,0.,0.624280230025758));
#47866=DIRECTION('',(-0.150042296859647,0.,0.988679578606275));
#47867=DIRECTION('',(-0.931242779705751,0.,0.364399348580519));
#47868=DIRECTION('',(-0.781200482846105,0.,-0.624280230025758));
#47869=DIRECTION('',(0.150042296859641,0.,-0.988679578606276));
#47870=DIRECTION('',(0.931242779705752,0.,-0.364399348580517));
#47871=DIRECTION('',(0.781200482846104,0.,0.624280230025758));
#47872=DIRECTION('',(-0.150042296859647,0.,0.988679578606275));
#47873=DIRECTION('',(-0.931242779705751,0.,0.364399348580519));
#47874=DIRECTION('',(-0.781200482846105,0.,-0.624280230025758));
#47875=DIRECTION('',(0.150042296859641,0.,-0.988679578606276));
#47876=DIRECTION('',(0.931242779705752,0.,-0.364399348580517));
#47877=DIRECTION('',(0.781200482846104,0.,0.624280230025758));
#47878=DIRECTION('',(-0.150042296859647,0.,0.988679578606275));
#47879=DIRECTION('',(-0.931242779705751,0.,0.364399348580519));
#47880=DIRECTION('',(-0.781200482846105,0.,-0.624280230025758));
#47881=DIRECTION('',(0.150042296859641,0.,-0.988679578606276));
#47882=DIRECTION('',(0.931242779705752,0.,-0.364399348580517));
#47883=DIRECTION('',(0.781200482846104,0.,0.624280230025758));
#47884=DIRECTION('',(-0.150042296859647,0.,0.988679578606275));
#47885=DIRECTION('',(-0.931242779705751,0.,0.364399348580519));
#47886=DIRECTION('',(-0.781200482846105,0.,-0.624280230025758));
#47887=DIRECTION('',(0.150042296859641,0.,-0.988679578606276));
#47888=DIRECTION('',(0.931242779705752,0.,-0.364399348580517));
#47889=DIRECTION('',(0.781200482846104,0.,0.624280230025758));
#47890=DIRECTION('',(-0.150042296859647,0.,0.988679578606275));
#47891=DIRECTION('',(-0.931242779705751,0.,0.364399348580519));
#47892=DIRECTION('',(-0.781200482846105,0.,-0.624280230025758));
#47893=DIRECTION('',(0.150042296859641,0.,-0.988679578606276));
#47894=DIRECTION('',(0.931242779705752,0.,-0.364399348580517));
#47895=DIRECTION('',(0.781200482846104,0.,0.624280230025758));
#47896=DIRECTION('',(-0.150042296859647,0.,0.988679578606275));
#47897=DIRECTION('',(-0.931242779705751,0.,0.364399348580519));
#47898=DIRECTION('',(-0.781200482846105,0.,-0.624280230025758));
#47899=DIRECTION('',(0.150042296859641,0.,-0.988679578606276));
#47900=DIRECTION('',(0.931242779705752,0.,-0.364399348580517));
#47901=DIRECTION('',(0.781200482846104,0.,0.624280230025758));
#47902=DIRECTION('',(-0.150042296859647,0.,0.988679578606275));
#47903=DIRECTION('',(-0.931242779705751,0.,0.364399348580519));
#47904=DIRECTION('',(-0.781200482846105,0.,-0.624280230025758));
#47905=DIRECTION('',(0.150042296859641,0.,-0.988679578606276));
#47906=DIRECTION('',(0.931242779705752,0.,-0.364399348580517));
#47907=DIRECTION('',(0.781200482846104,0.,0.624280230025758));
#47908=DIRECTION('',(-0.150042296859647,0.,0.988679578606275));
#47909=DIRECTION('',(-0.931242779705751,0.,0.364399348580519));
#47910=DIRECTION('',(-0.781200482846105,0.,-0.624280230025758));
#47911=DIRECTION('',(0.150042296859641,0.,-0.988679578606276));
#47912=DIRECTION('',(0.931242779705752,0.,-0.364399348580517));
#47913=DIRECTION('',(0.781200482846104,0.,0.624280230025758));
#47914=DIRECTION('',(-0.150042296859647,0.,0.988679578606275));
#47915=DIRECTION('',(-0.931242779705751,0.,0.364399348580519));
#47916=DIRECTION('',(-0.781200482846105,0.,-0.624280230025758));
#47917=DIRECTION('',(0.150042296859641,0.,-0.988679578606276));
#47918=DIRECTION('',(0.931242779705752,0.,-0.364399348580517));
#47919=DIRECTION('',(0.781200482846104,0.,0.624280230025758));
#47920=DIRECTION('',(-0.150042296859647,0.,0.988679578606275));
#47921=DIRECTION('',(-0.931242779705751,0.,0.364399348580519));
#47922=DIRECTION('',(-0.781200482846105,0.,-0.624280230025758));
#47923=DIRECTION('',(0.150042296859641,0.,-0.988679578606276));
#47924=DIRECTION('',(0.931242779705752,0.,-0.364399348580517));
#47925=DIRECTION('',(0.781200482846104,0.,0.624280230025758));
#47926=DIRECTION('',(-0.150042296859647,0.,0.988679578606275));
#47927=DIRECTION('',(-0.931242779705751,0.,0.364399348580519));
#47928=DIRECTION('',(-0.781200482846105,0.,-0.624280230025758));
#47929=DIRECTION('',(0.150042296859641,0.,-0.988679578606276));
#47930=DIRECTION('',(0.931242779705752,0.,-0.364399348580517));
#47931=DIRECTION('',(0.781200482846104,0.,0.624280230025758));
#47932=DIRECTION('',(-0.150042296859647,0.,0.988679578606275));
#47933=DIRECTION('',(-0.931242779705751,0.,0.364399348580519));
#47934=DIRECTION('',(-0.781200482846105,0.,-0.624280230025758));
#47935=DIRECTION('',(0.150042296859641,0.,-0.988679578606276));
#47936=DIRECTION('',(0.931242779705752,0.,-0.364399348580517));
#47937=DIRECTION('',(0.781200482846104,0.,0.624280230025758));
#47938=DIRECTION('',(-0.150042296859647,0.,0.988679578606275));
#47939=DIRECTION('',(-0.931242779705751,0.,0.364399348580519));
#47940=DIRECTION('',(-0.781200482846105,0.,-0.624280230025758));
#47941=DIRECTION('',(0.150042296859641,0.,-0.988679578606276));
#47942=DIRECTION('',(0.931242779705752,0.,-0.364399348580517));
#47943=DIRECTION('',(0.781200482846104,0.,0.624280230025758));
#47944=DIRECTION('',(-0.150042296859647,0.,0.988679578606275));
#47945=DIRECTION('',(-0.931242779705751,0.,0.364399348580519));
#47946=DIRECTION('',(-0.781200482846105,0.,-0.624280230025758));
#47947=DIRECTION('',(0.150042296859641,0.,-0.988679578606276));
#47948=DIRECTION('',(0.931242779705752,0.,-0.364399348580517));
#47949=DIRECTION('',(0.781200482846104,0.,0.624280230025758));
#47950=DIRECTION('',(-0.150042296859647,0.,0.988679578606275));
#47951=DIRECTION('',(-0.931242779705751,0.,0.364399348580519));
#47952=DIRECTION('',(-0.781200482846105,0.,-0.624280230025758));
#47953=DIRECTION('',(0.150042296859641,0.,-0.988679578606276));
#47954=DIRECTION('',(0.931242779705752,0.,-0.364399348580517));
#47955=DIRECTION('',(0.781200482846104,0.,0.624280230025758));
#47956=DIRECTION('',(-0.150042296859647,0.,0.988679578606275));
#47957=DIRECTION('',(-0.931242779705751,0.,0.364399348580519));
#47958=DIRECTION('',(-0.781200482846105,0.,-0.624280230025758));
#47959=DIRECTION('',(0.150042296859641,0.,-0.988679578606276));
#47960=DIRECTION('',(0.931242779705752,0.,-0.364399348580517));
#47961=DIRECTION('',(0.781200482846104,0.,0.624280230025758));
#47962=DIRECTION('',(-0.150042296859647,0.,0.988679578606275));
#47963=DIRECTION('',(-0.931242779705751,0.,0.364399348580519));
#47964=DIRECTION('',(-0.781200482846105,0.,-0.624280230025758));
#47965=DIRECTION('',(0.150042296859641,0.,-0.988679578606276));
#47966=DIRECTION('',(0.931242779705752,0.,-0.364399348580517));
#47967=DIRECTION('',(0.781200482846104,0.,0.624280230025758));
#47968=DIRECTION('',(-0.150042296859647,0.,0.988679578606275));
#47969=DIRECTION('',(-0.931242779705751,0.,0.364399348580519));
#47970=DIRECTION('',(-0.781200482846105,0.,-0.624280230025758));
#47971=DIRECTION('',(0.150042296859641,0.,-0.988679578606276));
#47972=DIRECTION('',(0.931242779705752,0.,-0.364399348580517));
#47973=DIRECTION('',(0.781200482846104,0.,0.624280230025758));
#47974=DIRECTION('',(-0.150042296859647,0.,0.988679578606275));
#47975=DIRECTION('',(-0.931242779705751,0.,0.364399348580519));
#47976=DIRECTION('',(-0.781200482846105,0.,-0.624280230025758));
#47977=DIRECTION('center_axis',(0.,1.,0.));
#47978=DIRECTION('ref_axis',(1.,0.,0.));
#47979=DIRECTION('',(0.931242779705752,0.,-0.364399348580517));
#47980=DIRECTION('',(0.150042296859641,0.,-0.988679578606276));
#47981=DIRECTION('',(-0.781200482846105,0.,-0.624280230025758));
#47982=DIRECTION('',(-0.931242779705751,0.,0.364399348580519));
#47983=DIRECTION('',(-0.150042296859647,0.,0.988679578606275));
#47984=DIRECTION('',(0.781200482846104,0.,0.624280230025758));
#47985=DIRECTION('',(0.931242779705752,0.,-0.364399348580517));
#47986=DIRECTION('',(0.150042296859641,0.,-0.988679578606276));
#47987=DIRECTION('',(-0.781200482846105,0.,-0.624280230025758));
#47988=DIRECTION('',(-0.931242779705751,0.,0.364399348580519));
#47989=DIRECTION('',(-0.150042296859647,0.,0.988679578606275));
#47990=DIRECTION('',(0.781200482846104,0.,0.624280230025758));
#47991=DIRECTION('',(0.931242779705752,0.,-0.364399348580517));
#47992=DIRECTION('',(0.150042296859641,0.,-0.988679578606276));
#47993=DIRECTION('',(-0.781200482846105,0.,-0.624280230025758));
#47994=DIRECTION('',(-0.931242779705751,0.,0.364399348580519));
#47995=DIRECTION('',(-0.150042296859647,0.,0.988679578606275));
#47996=DIRECTION('',(0.781200482846104,0.,0.624280230025758));
#47997=DIRECTION('',(0.931242779705752,0.,-0.364399348580517));
#47998=DIRECTION('',(0.150042296859641,0.,-0.988679578606276));
#47999=DIRECTION('',(-0.781200482846105,0.,-0.624280230025758));
#48000=DIRECTION('',(-0.931242779705751,0.,0.364399348580519));
#48001=DIRECTION('',(-0.150042296859647,0.,0.988679578606275));
#48002=DIRECTION('',(0.781200482846104,0.,0.624280230025758));
#48003=DIRECTION('',(0.931242779705752,0.,-0.364399348580517));
#48004=DIRECTION('',(0.150042296859641,0.,-0.988679578606276));
#48005=DIRECTION('',(-0.781200482846105,0.,-0.624280230025758));
#48006=DIRECTION('',(-0.931242779705751,0.,0.364399348580519));
#48007=DIRECTION('',(-0.150042296859647,0.,0.988679578606275));
#48008=DIRECTION('',(0.781200482846104,0.,0.624280230025758));
#48009=DIRECTION('',(0.931242779705752,0.,-0.364399348580517));
#48010=DIRECTION('',(0.150042296859641,0.,-0.988679578606276));
#48011=DIRECTION('',(-0.781200482846105,0.,-0.624280230025758));
#48012=DIRECTION('',(-0.931242779705751,0.,0.364399348580519));
#48013=DIRECTION('',(-0.150042296859647,0.,0.988679578606275));
#48014=DIRECTION('',(0.781200482846104,0.,0.624280230025758));
#48015=DIRECTION('',(0.931242779705752,0.,-0.364399348580517));
#48016=DIRECTION('',(0.150042296859641,0.,-0.988679578606276));
#48017=DIRECTION('',(-0.781200482846105,0.,-0.624280230025758));
#48018=DIRECTION('',(-0.931242779705751,0.,0.364399348580519));
#48019=DIRECTION('',(-0.150042296859647,0.,0.988679578606275));
#48020=DIRECTION('',(0.781200482846104,0.,0.624280230025758));
#48021=DIRECTION('',(0.931242779705752,0.,-0.364399348580517));
#48022=DIRECTION('',(0.150042296859641,0.,-0.988679578606276));
#48023=DIRECTION('',(-0.781200482846105,0.,-0.624280230025758));
#48024=DIRECTION('',(-0.931242779705751,0.,0.364399348580519));
#48025=DIRECTION('',(-0.150042296859647,0.,0.988679578606275));
#48026=DIRECTION('',(0.781200482846104,0.,0.624280230025758));
#48027=DIRECTION('',(0.931242779705752,0.,-0.364399348580517));
#48028=DIRECTION('',(0.150042296859641,0.,-0.988679578606276));
#48029=DIRECTION('',(-0.781200482846105,0.,-0.624280230025758));
#48030=DIRECTION('',(-0.931242779705751,0.,0.364399348580519));
#48031=DIRECTION('',(-0.150042296859647,0.,0.988679578606275));
#48032=DIRECTION('',(0.781200482846104,0.,0.624280230025758));
#48033=DIRECTION('',(0.931242779705752,0.,-0.364399348580517));
#48034=DIRECTION('',(0.150042296859641,0.,-0.988679578606276));
#48035=DIRECTION('',(-0.781200482846105,0.,-0.624280230025758));
#48036=DIRECTION('',(-0.931242779705751,0.,0.364399348580519));
#48037=DIRECTION('',(-0.150042296859647,0.,0.988679578606275));
#48038=DIRECTION('',(0.781200482846104,0.,0.624280230025758));
#48039=DIRECTION('',(0.931242779705752,0.,-0.364399348580517));
#48040=DIRECTION('',(0.150042296859641,0.,-0.988679578606276));
#48041=DIRECTION('',(-0.781200482846105,0.,-0.624280230025758));
#48042=DIRECTION('',(-0.931242779705751,0.,0.364399348580519));
#48043=DIRECTION('',(-0.150042296859647,0.,0.988679578606275));
#48044=DIRECTION('',(0.781200482846104,0.,0.624280230025758));
#48045=DIRECTION('',(0.931242779705752,0.,-0.364399348580517));
#48046=DIRECTION('',(0.150042296859641,0.,-0.988679578606276));
#48047=DIRECTION('',(-0.781200482846105,0.,-0.624280230025758));
#48048=DIRECTION('',(-0.931242779705751,0.,0.364399348580519));
#48049=DIRECTION('',(-0.150042296859647,0.,0.988679578606275));
#48050=DIRECTION('',(0.781200482846104,0.,0.624280230025758));
#48051=DIRECTION('',(0.931242779705752,0.,-0.364399348580517));
#48052=DIRECTION('',(0.150042296859641,0.,-0.988679578606276));
#48053=DIRECTION('',(-0.781200482846105,0.,-0.624280230025758));
#48054=DIRECTION('',(-0.931242779705751,0.,0.364399348580519));
#48055=DIRECTION('',(-0.150042296859647,0.,0.988679578606275));
#48056=DIRECTION('',(0.781200482846104,0.,0.624280230025758));
#48057=DIRECTION('',(0.931242779705752,0.,-0.364399348580517));
#48058=DIRECTION('',(0.150042296859641,0.,-0.988679578606276));
#48059=DIRECTION('',(-0.781200482846105,0.,-0.624280230025758));
#48060=DIRECTION('',(-0.931242779705751,0.,0.364399348580519));
#48061=DIRECTION('',(-0.150042296859647,0.,0.988679578606275));
#48062=DIRECTION('',(0.781200482846104,0.,0.624280230025758));
#48063=DIRECTION('',(0.931242779705752,0.,-0.364399348580517));
#48064=DIRECTION('',(0.150042296859641,0.,-0.988679578606276));
#48065=DIRECTION('',(-0.781200482846105,0.,-0.624280230025758));
#48066=DIRECTION('',(-0.931242779705751,0.,0.364399348580519));
#48067=DIRECTION('',(-0.150042296859647,0.,0.988679578606275));
#48068=DIRECTION('',(0.781200482846104,0.,0.624280230025758));
#48069=DIRECTION('',(0.931242779705752,0.,-0.364399348580517));
#48070=DIRECTION('',(0.150042296859641,0.,-0.988679578606276));
#48071=DIRECTION('',(-0.781200482846105,0.,-0.624280230025758));
#48072=DIRECTION('',(-0.931242779705751,0.,0.364399348580519));
#48073=DIRECTION('',(-0.150042296859647,0.,0.988679578606275));
#48074=DIRECTION('',(0.781200482846104,0.,0.624280230025758));
#48075=DIRECTION('',(0.931242779705752,0.,-0.364399348580517));
#48076=DIRECTION('',(0.150042296859641,0.,-0.988679578606276));
#48077=DIRECTION('',(-0.781200482846105,0.,-0.624280230025758));
#48078=DIRECTION('',(-0.931242779705751,0.,0.364399348580519));
#48079=DIRECTION('',(-0.150042296859647,0.,0.988679578606275));
#48080=DIRECTION('',(0.781200482846104,0.,0.624280230025758));
#48081=DIRECTION('',(0.931242779705752,0.,-0.364399348580517));
#48082=DIRECTION('',(0.150042296859641,0.,-0.988679578606276));
#48083=DIRECTION('',(-0.781200482846105,0.,-0.624280230025758));
#48084=DIRECTION('',(-0.931242779705751,0.,0.364399348580519));
#48085=DIRECTION('',(-0.150042296859647,0.,0.988679578606275));
#48086=DIRECTION('',(0.781200482846104,0.,0.624280230025758));
#48087=DIRECTION('',(0.931242779705752,0.,-0.364399348580517));
#48088=DIRECTION('',(0.150042296859641,0.,-0.988679578606276));
#48089=DIRECTION('',(-0.781200482846105,0.,-0.624280230025758));
#48090=DIRECTION('',(-0.931242779705751,0.,0.364399348580519));
#48091=DIRECTION('',(-0.150042296859647,0.,0.988679578606275));
#48092=DIRECTION('',(0.781200482846104,0.,0.624280230025758));
#48093=DIRECTION('',(0.931242779705752,0.,-0.364399348580517));
#48094=DIRECTION('',(0.150042296859641,0.,-0.988679578606276));
#48095=DIRECTION('',(-0.781200482846105,0.,-0.624280230025758));
#48096=DIRECTION('',(-0.931242779705751,0.,0.364399348580519));
#48097=DIRECTION('',(-0.150042296859647,0.,0.988679578606275));
#48098=DIRECTION('',(0.781200482846104,0.,0.624280230025758));
#48099=DIRECTION('',(0.931242779705752,0.,-0.364399348580517));
#48100=DIRECTION('',(0.150042296859641,0.,-0.988679578606276));
#48101=DIRECTION('',(-0.781200482846105,0.,-0.624280230025758));
#48102=DIRECTION('',(-0.931242779705751,0.,0.364399348580519));
#48103=DIRECTION('',(-0.150042296859647,0.,0.988679578606275));
#48104=DIRECTION('',(0.781200482846104,0.,0.624280230025758));
#48105=DIRECTION('',(0.931242779705752,0.,-0.364399348580517));
#48106=DIRECTION('',(0.150042296859641,0.,-0.988679578606276));
#48107=DIRECTION('',(-0.781200482846105,0.,-0.624280230025758));
#48108=DIRECTION('',(-0.931242779705751,0.,0.364399348580519));
#48109=DIRECTION('',(-0.150042296859647,0.,0.988679578606275));
#48110=DIRECTION('',(0.781200482846104,0.,0.624280230025758));
#48111=DIRECTION('',(0.931242779705752,0.,-0.364399348580517));
#48112=DIRECTION('',(0.150042296859641,0.,-0.988679578606276));
#48113=DIRECTION('',(-0.781200482846105,0.,-0.624280230025758));
#48114=DIRECTION('',(-0.931242779705751,0.,0.364399348580519));
#48115=DIRECTION('',(-0.150042296859647,0.,0.988679578606275));
#48116=DIRECTION('',(0.781200482846104,0.,0.624280230025758));
#48117=DIRECTION('',(0.931242779705752,0.,-0.364399348580517));
#48118=DIRECTION('',(0.150042296859641,0.,-0.988679578606276));
#48119=DIRECTION('',(-0.781200482846105,0.,-0.624280230025758));
#48120=DIRECTION('',(-0.931242779705751,0.,0.364399348580519));
#48121=DIRECTION('',(-0.150042296859647,0.,0.988679578606275));
#48122=DIRECTION('',(0.781200482846104,0.,0.624280230025758));
#48123=DIRECTION('',(0.931242779705752,0.,-0.364399348580517));
#48124=DIRECTION('',(0.150042296859641,0.,-0.988679578606276));
#48125=DIRECTION('',(-0.781200482846105,0.,-0.624280230025758));
#48126=DIRECTION('',(-0.931242779705751,0.,0.364399348580519));
#48127=DIRECTION('',(-0.150042296859647,0.,0.988679578606275));
#48128=DIRECTION('',(0.781200482846104,0.,0.624280230025758));
#48129=DIRECTION('',(0.931242779705752,0.,-0.364399348580517));
#48130=DIRECTION('',(0.150042296859641,0.,-0.988679578606276));
#48131=DIRECTION('',(-0.781200482846105,0.,-0.624280230025758));
#48132=DIRECTION('',(-0.931242779705751,0.,0.364399348580519));
#48133=DIRECTION('',(-0.150042296859647,0.,0.988679578606275));
#48134=DIRECTION('',(0.781200482846104,0.,0.624280230025758));
#48135=DIRECTION('',(0.931242779705752,0.,-0.364399348580517));
#48136=DIRECTION('',(0.150042296859641,0.,-0.988679578606276));
#48137=DIRECTION('',(-0.781200482846105,0.,-0.624280230025758));
#48138=DIRECTION('',(-0.931242779705751,0.,0.364399348580519));
#48139=DIRECTION('',(-0.150042296859647,0.,0.988679578606275));
#48140=DIRECTION('',(0.781200482846104,0.,0.624280230025758));
#48141=DIRECTION('',(0.931242779705752,0.,-0.364399348580517));
#48142=DIRECTION('',(0.150042296859641,0.,-0.988679578606276));
#48143=DIRECTION('',(-0.781200482846105,0.,-0.624280230025758));
#48144=DIRECTION('',(-0.931242779705751,0.,0.364399348580519));
#48145=DIRECTION('',(-0.150042296859647,0.,0.988679578606275));
#48146=DIRECTION('',(0.781200482846104,0.,0.624280230025758));
#48147=DIRECTION('',(0.931242779705752,0.,-0.364399348580517));
#48148=DIRECTION('',(0.150042296859641,0.,-0.988679578606276));
#48149=DIRECTION('',(-0.781200482846105,0.,-0.624280230025758));
#48150=DIRECTION('',(-0.931242779705751,0.,0.364399348580519));
#48151=DIRECTION('',(-0.150042296859647,0.,0.988679578606275));
#48152=DIRECTION('',(0.781200482846104,0.,0.624280230025758));
#48153=DIRECTION('',(0.931242779705752,0.,-0.364399348580517));
#48154=DIRECTION('',(0.150042296859641,0.,-0.988679578606276));
#48155=DIRECTION('',(-0.781200482846105,0.,-0.624280230025758));
#48156=DIRECTION('',(-0.931242779705751,0.,0.364399348580519));
#48157=DIRECTION('',(-0.150042296859647,0.,0.988679578606275));
#48158=DIRECTION('',(0.781200482846104,0.,0.624280230025758));
#48159=DIRECTION('',(0.931242779705752,0.,-0.364399348580517));
#48160=DIRECTION('',(0.150042296859641,0.,-0.988679578606276));
#48161=DIRECTION('',(-0.781200482846105,0.,-0.624280230025758));
#48162=DIRECTION('',(-0.931242779705751,0.,0.364399348580519));
#48163=DIRECTION('',(-0.150042296859647,0.,0.988679578606275));
#48164=DIRECTION('',(0.781200482846104,0.,0.624280230025758));
#48165=DIRECTION('',(0.931242779705752,0.,-0.364399348580517));
#48166=DIRECTION('',(0.150042296859641,0.,-0.988679578606276));
#48167=DIRECTION('',(-0.781200482846105,0.,-0.624280230025758));
#48168=DIRECTION('',(-0.931242779705751,0.,0.364399348580519));
#48169=DIRECTION('',(-0.150042296859647,0.,0.988679578606275));
#48170=DIRECTION('',(0.781200482846104,0.,0.624280230025758));
#48171=DIRECTION('',(0.931242779705752,0.,-0.364399348580517));
#48172=DIRECTION('',(0.150042296859641,0.,-0.988679578606276));
#48173=DIRECTION('',(-0.781200482846105,0.,-0.624280230025758));
#48174=DIRECTION('',(-0.931242779705751,0.,0.364399348580519));
#48175=DIRECTION('',(-0.150042296859647,0.,0.988679578606275));
#48176=DIRECTION('',(0.781200482846104,0.,0.624280230025758));
#48177=DIRECTION('',(0.931242779705752,0.,-0.364399348580517));
#48178=DIRECTION('',(0.150042296859641,0.,-0.988679578606276));
#48179=DIRECTION('',(-0.781200482846105,0.,-0.624280230025758));
#48180=DIRECTION('',(-0.931242779705751,0.,0.364399348580519));
#48181=DIRECTION('',(-0.150042296859647,0.,0.988679578606275));
#48182=DIRECTION('',(0.781200482846104,0.,0.624280230025758));
#48183=DIRECTION('',(0.931242779705752,0.,-0.364399348580517));
#48184=DIRECTION('',(0.150042296859641,0.,-0.988679578606276));
#48185=DIRECTION('',(-0.781200482846105,0.,-0.624280230025758));
#48186=DIRECTION('',(-0.931242779705751,0.,0.364399348580519));
#48187=DIRECTION('',(-0.150042296859647,0.,0.988679578606275));
#48188=DIRECTION('',(0.781200482846104,0.,0.624280230025758));
#48189=DIRECTION('',(0.931242779705752,0.,-0.364399348580517));
#48190=DIRECTION('',(0.150042296859641,0.,-0.988679578606276));
#48191=DIRECTION('',(-0.781200482846105,0.,-0.624280230025758));
#48192=DIRECTION('',(-0.931242779705751,0.,0.364399348580519));
#48193=DIRECTION('',(-0.150042296859647,0.,0.988679578606275));
#48194=DIRECTION('',(0.781200482846104,0.,0.624280230025758));
#48195=DIRECTION('',(0.931242779705752,0.,-0.364399348580517));
#48196=DIRECTION('',(0.150042296859641,0.,-0.988679578606276));
#48197=DIRECTION('',(-0.781200482846105,0.,-0.624280230025758));
#48198=DIRECTION('',(-0.931242779705751,0.,0.364399348580519));
#48199=DIRECTION('',(-0.150042296859647,0.,0.988679578606275));
#48200=DIRECTION('',(0.781200482846104,0.,0.624280230025758));
#48201=DIRECTION('',(0.931242779705752,0.,-0.364399348580517));
#48202=DIRECTION('',(0.150042296859641,0.,-0.988679578606276));
#48203=DIRECTION('',(-0.781200482846105,0.,-0.624280230025758));
#48204=DIRECTION('',(-0.931242779705751,0.,0.364399348580519));
#48205=DIRECTION('',(-0.150042296859647,0.,0.988679578606275));
#48206=DIRECTION('',(0.781200482846104,0.,0.624280230025758));
#48207=DIRECTION('',(0.931242779705752,0.,-0.364399348580517));
#48208=DIRECTION('',(0.150042296859641,0.,-0.988679578606276));
#48209=DIRECTION('',(-0.781200482846105,0.,-0.624280230025758));
#48210=DIRECTION('',(-0.931242779705751,0.,0.364399348580519));
#48211=DIRECTION('',(-0.150042296859647,0.,0.988679578606275));
#48212=DIRECTION('',(0.781200482846104,0.,0.624280230025758));
#48213=DIRECTION('',(0.931242779705752,0.,-0.364399348580517));
#48214=DIRECTION('',(0.150042296859641,0.,-0.988679578606276));
#48215=DIRECTION('',(-0.781200482846105,0.,-0.624280230025758));
#48216=DIRECTION('',(-0.931242779705751,0.,0.364399348580519));
#48217=DIRECTION('',(-0.150042296859647,0.,0.988679578606275));
#48218=DIRECTION('',(0.781200482846104,0.,0.624280230025758));
#48219=DIRECTION('',(0.931242779705752,0.,-0.364399348580517));
#48220=DIRECTION('',(0.150042296859641,0.,-0.988679578606276));
#48221=DIRECTION('',(-0.781200482846105,0.,-0.624280230025758));
#48222=DIRECTION('',(-0.931242779705751,0.,0.364399348580519));
#48223=DIRECTION('',(-0.150042296859647,0.,0.988679578606275));
#48224=DIRECTION('',(0.781200482846104,0.,0.624280230025758));
#48225=DIRECTION('',(0.931242779705752,0.,-0.364399348580517));
#48226=DIRECTION('',(0.150042296859641,0.,-0.988679578606276));
#48227=DIRECTION('',(-0.781200482846105,0.,-0.624280230025758));
#48228=DIRECTION('',(-0.931242779705751,0.,0.364399348580519));
#48229=DIRECTION('',(-0.150042296859647,0.,0.988679578606275));
#48230=DIRECTION('',(0.781200482846104,0.,0.624280230025758));
#48231=DIRECTION('',(0.931242779705752,0.,-0.364399348580517));
#48232=DIRECTION('',(0.150042296859641,0.,-0.988679578606276));
#48233=DIRECTION('',(-0.781200482846105,0.,-0.624280230025758));
#48234=DIRECTION('',(-0.931242779705751,0.,0.364399348580519));
#48235=DIRECTION('',(-0.150042296859647,0.,0.988679578606275));
#48236=DIRECTION('',(0.781200482846104,0.,0.624280230025758));
#48237=DIRECTION('',(0.931242779705752,0.,-0.364399348580517));
#48238=DIRECTION('',(0.150042296859641,0.,-0.988679578606276));
#48239=DIRECTION('',(-0.781200482846105,0.,-0.624280230025758));
#48240=DIRECTION('',(-0.931242779705751,0.,0.364399348580519));
#48241=DIRECTION('',(-0.150042296859647,0.,0.988679578606275));
#48242=DIRECTION('',(0.781200482846104,0.,0.624280230025758));
#48243=DIRECTION('',(0.931242779705752,0.,-0.364399348580517));
#48244=DIRECTION('',(0.150042296859641,0.,-0.988679578606276));
#48245=DIRECTION('',(-0.781200482846105,0.,-0.624280230025758));
#48246=DIRECTION('',(-0.931242779705751,0.,0.364399348580519));
#48247=DIRECTION('',(-0.150042296859647,0.,0.988679578606275));
#48248=DIRECTION('',(0.781200482846104,0.,0.624280230025758));
#48249=DIRECTION('',(0.931242779705752,0.,-0.364399348580517));
#48250=DIRECTION('',(0.150042296859641,0.,-0.988679578606276));
#48251=DIRECTION('',(-0.781200482846105,0.,-0.624280230025758));
#48252=DIRECTION('',(-0.931242779705751,0.,0.364399348580519));
#48253=DIRECTION('',(-0.150042296859647,0.,0.988679578606275));
#48254=DIRECTION('',(0.781200482846104,0.,0.624280230025758));
#48255=DIRECTION('',(0.931242779705752,0.,-0.364399348580517));
#48256=DIRECTION('',(0.150042296859641,0.,-0.988679578606276));
#48257=DIRECTION('',(-0.781200482846105,0.,-0.624280230025758));
#48258=DIRECTION('',(-0.931242779705751,0.,0.364399348580519));
#48259=DIRECTION('',(-0.150042296859647,0.,0.988679578606275));
#48260=DIRECTION('',(0.781200482846104,0.,0.624280230025758));
#48261=DIRECTION('',(0.931242779705752,0.,-0.364399348580517));
#48262=DIRECTION('',(0.150042296859641,0.,-0.988679578606276));
#48263=DIRECTION('',(-0.781200482846105,0.,-0.624280230025758));
#48264=DIRECTION('',(-0.931242779705751,0.,0.364399348580519));
#48265=DIRECTION('',(-0.150042296859647,0.,0.988679578606275));
#48266=DIRECTION('',(0.781200482846104,0.,0.624280230025758));
#48267=DIRECTION('',(0.931242779705752,0.,-0.364399348580517));
#48268=DIRECTION('',(0.150042296859641,0.,-0.988679578606276));
#48269=DIRECTION('',(-0.781200482846105,0.,-0.624280230025758));
#48270=DIRECTION('',(-0.931242779705751,0.,0.364399348580519));
#48271=DIRECTION('',(-0.150042296859647,0.,0.988679578606275));
#48272=DIRECTION('',(0.781200482846104,0.,0.624280230025758));
#48273=DIRECTION('',(0.931242779705752,0.,-0.364399348580517));
#48274=DIRECTION('',(0.150042296859641,0.,-0.988679578606276));
#48275=DIRECTION('',(-0.781200482846105,0.,-0.624280230025758));
#48276=DIRECTION('',(-0.931242779705751,0.,0.364399348580519));
#48277=DIRECTION('',(-0.150042296859647,0.,0.988679578606275));
#48278=DIRECTION('',(0.781200482846104,0.,0.624280230025758));
#48279=DIRECTION('',(0.931242779705752,0.,-0.364399348580517));
#48280=DIRECTION('',(0.150042296859641,0.,-0.988679578606276));
#48281=DIRECTION('',(-0.781200482846105,0.,-0.624280230025758));
#48282=DIRECTION('',(-0.931242779705751,0.,0.364399348580519));
#48283=DIRECTION('',(-0.150042296859647,0.,0.988679578606275));
#48284=DIRECTION('',(0.781200482846104,0.,0.624280230025758));
#48285=DIRECTION('',(0.931242779705752,0.,-0.364399348580517));
#48286=DIRECTION('',(0.150042296859641,0.,-0.988679578606276));
#48287=DIRECTION('',(-0.781200482846105,0.,-0.624280230025758));
#48288=DIRECTION('',(-0.931242779705751,0.,0.364399348580519));
#48289=DIRECTION('',(-0.150042296859647,0.,0.988679578606275));
#48290=DIRECTION('',(0.781200482846104,0.,0.624280230025758));
#48291=DIRECTION('',(0.931242779705752,0.,-0.364399348580517));
#48292=DIRECTION('',(0.150042296859641,0.,-0.988679578606276));
#48293=DIRECTION('',(-0.781200482846105,0.,-0.624280230025758));
#48294=DIRECTION('',(-0.931242779705751,0.,0.364399348580519));
#48295=DIRECTION('',(-0.150042296859647,0.,0.988679578606275));
#48296=DIRECTION('',(0.781200482846104,0.,0.624280230025758));
#48297=DIRECTION('',(0.931242779705752,0.,-0.364399348580517));
#48298=DIRECTION('',(0.150042296859641,0.,-0.988679578606276));
#48299=DIRECTION('',(-0.781200482846105,0.,-0.624280230025758));
#48300=DIRECTION('',(-0.931242779705751,0.,0.364399348580519));
#48301=DIRECTION('',(-0.150042296859647,0.,0.988679578606275));
#48302=DIRECTION('',(0.781200482846104,0.,0.624280230025758));
#48303=DIRECTION('',(0.931242779705752,0.,-0.364399348580517));
#48304=DIRECTION('',(0.150042296859641,0.,-0.988679578606276));
#48305=DIRECTION('',(-0.781200482846105,0.,-0.624280230025758));
#48306=DIRECTION('',(-0.931242779705751,0.,0.364399348580519));
#48307=DIRECTION('',(-0.150042296859647,0.,0.988679578606275));
#48308=DIRECTION('',(0.781200482846104,0.,0.624280230025758));
#48309=DIRECTION('',(0.931242779705752,0.,-0.364399348580517));
#48310=DIRECTION('',(0.150042296859641,0.,-0.988679578606276));
#48311=DIRECTION('',(-0.781200482846105,0.,-0.624280230025758));
#48312=DIRECTION('',(-0.931242779705751,0.,0.364399348580519));
#48313=DIRECTION('',(-0.150042296859647,0.,0.988679578606275));
#48314=DIRECTION('',(0.781200482846104,0.,0.624280230025758));
#48315=DIRECTION('',(0.931242779705752,0.,-0.364399348580517));
#48316=DIRECTION('',(0.150042296859641,0.,-0.988679578606276));
#48317=DIRECTION('',(-0.781200482846105,0.,-0.624280230025758));
#48318=DIRECTION('',(-0.931242779705751,0.,0.364399348580519));
#48319=DIRECTION('',(-0.150042296859647,0.,0.988679578606275));
#48320=DIRECTION('',(0.781200482846104,0.,0.624280230025758));
#48321=DIRECTION('',(0.931242779705752,0.,-0.364399348580517));
#48322=DIRECTION('',(0.150042296859641,0.,-0.988679578606276));
#48323=DIRECTION('',(-0.781200482846105,0.,-0.624280230025758));
#48324=DIRECTION('',(-0.931242779705751,0.,0.364399348580519));
#48325=DIRECTION('',(-0.150042296859647,0.,0.988679578606275));
#48326=DIRECTION('',(0.781200482846104,0.,0.624280230025758));
#48327=DIRECTION('',(0.931242779705752,0.,-0.364399348580517));
#48328=DIRECTION('',(0.150042296859641,0.,-0.988679578606276));
#48329=DIRECTION('',(-0.781200482846105,0.,-0.624280230025758));
#48330=DIRECTION('',(-0.931242779705751,0.,0.364399348580519));
#48331=DIRECTION('',(-0.150042296859647,0.,0.988679578606275));
#48332=DIRECTION('',(0.781200482846104,0.,0.624280230025758));
#48333=DIRECTION('',(0.931242779705752,0.,-0.364399348580517));
#48334=DIRECTION('',(0.150042296859641,0.,-0.988679578606276));
#48335=DIRECTION('',(-0.781200482846105,0.,-0.624280230025758));
#48336=DIRECTION('',(-0.931242779705751,0.,0.364399348580519));
#48337=DIRECTION('',(-0.150042296859647,0.,0.988679578606275));
#48338=DIRECTION('',(0.781200482846104,0.,0.624280230025758));
#48339=DIRECTION('',(0.931242779705752,0.,-0.364399348580517));
#48340=DIRECTION('',(0.150042296859641,0.,-0.988679578606276));
#48341=DIRECTION('',(-0.781200482846105,0.,-0.624280230025758));
#48342=DIRECTION('',(-0.931242779705751,0.,0.364399348580519));
#48343=DIRECTION('',(-0.150042296859647,0.,0.988679578606275));
#48344=DIRECTION('',(0.781200482846104,0.,0.624280230025758));
#48345=DIRECTION('',(0.931242779705752,0.,-0.364399348580517));
#48346=DIRECTION('',(0.150042296859641,0.,-0.988679578606276));
#48347=DIRECTION('',(-0.781200482846105,0.,-0.624280230025758));
#48348=DIRECTION('',(-0.931242779705751,0.,0.364399348580519));
#48349=DIRECTION('',(-0.150042296859647,0.,0.988679578606275));
#48350=DIRECTION('',(0.781200482846104,0.,0.624280230025758));
#48351=DIRECTION('',(0.931242779705752,0.,-0.364399348580517));
#48352=DIRECTION('',(0.150042296859641,0.,-0.988679578606276));
#48353=DIRECTION('',(-0.781200482846105,0.,-0.624280230025758));
#48354=DIRECTION('',(-0.931242779705751,0.,0.364399348580519));
#48355=DIRECTION('',(-0.150042296859647,0.,0.988679578606275));
#48356=DIRECTION('',(0.781200482846104,0.,0.624280230025758));
#48357=DIRECTION('',(0.931242779705752,0.,-0.364399348580517));
#48358=DIRECTION('',(0.150042296859641,0.,-0.988679578606276));
#48359=DIRECTION('',(-0.781200482846105,0.,-0.624280230025758));
#48360=DIRECTION('',(-0.931242779705751,0.,0.364399348580519));
#48361=DIRECTION('',(-0.150042296859647,0.,0.988679578606275));
#48362=DIRECTION('',(0.781200482846104,0.,0.624280230025758));
#48363=DIRECTION('',(0.931242779705752,0.,-0.364399348580517));
#48364=DIRECTION('',(0.150042296859641,0.,-0.988679578606276));
#48365=DIRECTION('',(-0.781200482846105,0.,-0.624280230025758));
#48366=DIRECTION('',(-0.931242779705751,0.,0.364399348580519));
#48367=DIRECTION('',(-0.150042296859647,0.,0.988679578606275));
#48368=DIRECTION('',(0.781200482846104,0.,0.624280230025758));
#48369=DIRECTION('',(0.931242779705752,0.,-0.364399348580517));
#48370=DIRECTION('',(0.150042296859641,0.,-0.988679578606276));
#48371=DIRECTION('',(-0.781200482846105,0.,-0.624280230025758));
#48372=DIRECTION('',(-0.931242779705751,0.,0.364399348580519));
#48373=DIRECTION('',(-0.150042296859647,0.,0.988679578606275));
#48374=DIRECTION('',(0.781200482846104,0.,0.624280230025758));
#48375=DIRECTION('',(0.931242779705752,0.,-0.364399348580517));
#48376=DIRECTION('',(0.150042296859641,0.,-0.988679578606276));
#48377=DIRECTION('',(-0.781200482846105,0.,-0.624280230025758));
#48378=DIRECTION('',(-0.931242779705751,0.,0.364399348580519));
#48379=DIRECTION('',(-0.150042296859647,0.,0.988679578606275));
#48380=DIRECTION('',(0.781200482846104,0.,0.624280230025758));
#48381=DIRECTION('',(0.931242779705752,0.,-0.364399348580517));
#48382=DIRECTION('',(0.150042296859641,0.,-0.988679578606276));
#48383=DIRECTION('',(-0.781200482846105,0.,-0.624280230025758));
#48384=DIRECTION('',(-0.931242779705751,0.,0.364399348580519));
#48385=DIRECTION('',(-0.150042296859647,0.,0.988679578606275));
#48386=DIRECTION('',(0.781200482846104,0.,0.624280230025758));
#48387=DIRECTION('',(0.931242779705752,0.,-0.364399348580517));
#48388=DIRECTION('',(0.150042296859641,0.,-0.988679578606276));
#48389=DIRECTION('',(-0.781200482846105,0.,-0.624280230025758));
#48390=DIRECTION('',(-0.931242779705751,0.,0.364399348580519));
#48391=DIRECTION('',(-0.150042296859647,0.,0.988679578606275));
#48392=DIRECTION('',(0.781200482846104,0.,0.624280230025758));
#48393=DIRECTION('',(0.931242779705752,0.,-0.364399348580517));
#48394=DIRECTION('',(0.150042296859641,0.,-0.988679578606276));
#48395=DIRECTION('',(-0.781200482846105,0.,-0.624280230025758));
#48396=DIRECTION('',(-0.931242779705751,0.,0.364399348580519));
#48397=DIRECTION('',(-0.150042296859647,0.,0.988679578606275));
#48398=DIRECTION('',(0.781200482846104,0.,0.624280230025758));
#48399=DIRECTION('',(0.931242779705752,0.,-0.364399348580517));
#48400=DIRECTION('',(0.150042296859641,0.,-0.988679578606276));
#48401=DIRECTION('',(-0.781200482846105,0.,-0.624280230025758));
#48402=DIRECTION('',(-0.931242779705751,0.,0.364399348580519));
#48403=DIRECTION('',(-0.150042296859647,0.,0.988679578606275));
#48404=DIRECTION('',(0.781200482846104,0.,0.624280230025758));
#48405=DIRECTION('',(0.931242779705752,0.,-0.364399348580517));
#48406=DIRECTION('',(0.150042296859641,0.,-0.988679578606276));
#48407=DIRECTION('',(-0.781200482846105,0.,-0.624280230025758));
#48408=DIRECTION('',(-0.931242779705751,0.,0.364399348580519));
#48409=DIRECTION('',(-0.150042296859647,0.,0.988679578606275));
#48410=DIRECTION('',(0.781200482846104,0.,0.624280230025758));
#48411=DIRECTION('',(0.931242779705752,0.,-0.364399348580517));
#48412=DIRECTION('',(0.150042296859641,0.,-0.988679578606276));
#48413=DIRECTION('',(-0.781200482846105,0.,-0.624280230025758));
#48414=DIRECTION('',(-0.931242779705751,0.,0.364399348580519));
#48415=DIRECTION('',(-0.150042296859647,0.,0.988679578606275));
#48416=DIRECTION('',(0.781200482846104,0.,0.624280230025758));
#48417=DIRECTION('',(0.931242779705752,0.,-0.364399348580517));
#48418=DIRECTION('',(0.150042296859641,0.,-0.988679578606276));
#48419=DIRECTION('',(-0.781200482846105,0.,-0.624280230025758));
#48420=DIRECTION('',(-0.931242779705751,0.,0.364399348580519));
#48421=DIRECTION('',(-0.150042296859647,0.,0.988679578606275));
#48422=DIRECTION('',(0.781200482846104,0.,0.624280230025758));
#48423=DIRECTION('',(0.931242779705752,0.,-0.364399348580517));
#48424=DIRECTION('',(0.150042296859641,0.,-0.988679578606276));
#48425=DIRECTION('',(-0.781200482846105,0.,-0.624280230025758));
#48426=DIRECTION('',(-0.931242779705751,0.,0.364399348580519));
#48427=DIRECTION('',(-0.150042296859647,0.,0.988679578606275));
#48428=DIRECTION('',(0.781200482846104,0.,0.624280230025758));
#48429=DIRECTION('',(0.931242779705752,0.,-0.364399348580517));
#48430=DIRECTION('',(0.150042296859641,0.,-0.988679578606276));
#48431=DIRECTION('',(-0.781200482846105,0.,-0.624280230025758));
#48432=DIRECTION('',(-0.931242779705751,0.,0.364399348580519));
#48433=DIRECTION('',(-0.150042296859647,0.,0.988679578606275));
#48434=DIRECTION('',(0.781200482846104,0.,0.624280230025758));
#48435=DIRECTION('',(0.931242779705752,0.,-0.364399348580517));
#48436=DIRECTION('',(0.150042296859641,0.,-0.988679578606276));
#48437=DIRECTION('',(-0.781200482846105,0.,-0.624280230025758));
#48438=DIRECTION('',(-0.931242779705751,0.,0.364399348580519));
#48439=DIRECTION('',(-0.150042296859647,0.,0.988679578606275));
#48440=DIRECTION('',(0.781200482846104,0.,0.624280230025758));
#48441=DIRECTION('',(0.931242779705752,0.,-0.364399348580517));
#48442=DIRECTION('',(0.150042296859641,0.,-0.988679578606276));
#48443=DIRECTION('',(-0.781200482846105,0.,-0.624280230025758));
#48444=DIRECTION('',(-0.931242779705751,0.,0.364399348580519));
#48445=DIRECTION('',(-0.150042296859647,0.,0.988679578606275));
#48446=DIRECTION('',(0.781200482846104,0.,0.624280230025758));
#48447=DIRECTION('',(0.931242779705752,0.,-0.364399348580517));
#48448=DIRECTION('',(0.150042296859641,0.,-0.988679578606276));
#48449=DIRECTION('',(-0.781200482846105,0.,-0.624280230025758));
#48450=DIRECTION('',(-0.931242779705751,0.,0.364399348580519));
#48451=DIRECTION('',(-0.150042296859647,0.,0.988679578606275));
#48452=DIRECTION('',(0.781200482846104,0.,0.624280230025758));
#48453=DIRECTION('',(0.931242779705752,0.,-0.364399348580517));
#48454=DIRECTION('',(0.150042296859641,0.,-0.988679578606276));
#48455=DIRECTION('',(-0.781200482846105,0.,-0.624280230025758));
#48456=DIRECTION('',(-0.931242779705751,0.,0.364399348580519));
#48457=DIRECTION('',(-0.150042296859647,0.,0.988679578606275));
#48458=DIRECTION('',(0.781200482846104,0.,0.624280230025758));
#48459=DIRECTION('',(0.931242779705752,0.,-0.364399348580517));
#48460=DIRECTION('',(0.150042296859641,0.,-0.988679578606276));
#48461=DIRECTION('',(-0.781200482846105,0.,-0.624280230025758));
#48462=DIRECTION('',(-0.931242779705751,0.,0.364399348580519));
#48463=DIRECTION('',(-0.150042296859647,0.,0.988679578606275));
#48464=DIRECTION('',(0.781200482846104,0.,0.624280230025758));
#48465=DIRECTION('',(0.931242779705752,0.,-0.364399348580517));
#48466=DIRECTION('',(0.150042296859641,0.,-0.988679578606276));
#48467=DIRECTION('',(-0.781200482846105,0.,-0.624280230025758));
#48468=DIRECTION('',(-0.931242779705751,0.,0.364399348580519));
#48469=DIRECTION('',(-0.150042296859647,0.,0.988679578606275));
#48470=DIRECTION('',(0.781200482846104,0.,0.624280230025758));
#48471=DIRECTION('',(0.931242779705752,0.,-0.364399348580517));
#48472=DIRECTION('',(0.150042296859641,0.,-0.988679578606276));
#48473=DIRECTION('',(-0.781200482846105,0.,-0.624280230025758));
#48474=DIRECTION('',(-0.931242779705751,0.,0.364399348580519));
#48475=DIRECTION('',(-0.150042296859647,0.,0.988679578606275));
#48476=DIRECTION('',(0.781200482846104,0.,0.624280230025758));
#48477=DIRECTION('',(0.931242779705752,0.,-0.364399348580517));
#48478=DIRECTION('',(0.150042296859641,0.,-0.988679578606276));
#48479=DIRECTION('',(-0.781200482846105,0.,-0.624280230025758));
#48480=DIRECTION('',(-0.931242779705751,0.,0.364399348580519));
#48481=DIRECTION('',(-0.150042296859647,0.,0.988679578606275));
#48482=DIRECTION('',(0.781200482846104,0.,0.624280230025758));
#48483=DIRECTION('',(0.931242779705752,0.,-0.364399348580517));
#48484=DIRECTION('',(0.150042296859641,0.,-0.988679578606276));
#48485=DIRECTION('',(-0.781200482846105,0.,-0.624280230025758));
#48486=DIRECTION('',(-0.931242779705751,0.,0.364399348580519));
#48487=DIRECTION('',(-0.150042296859647,0.,0.988679578606275));
#48488=DIRECTION('',(0.781200482846104,0.,0.624280230025758));
#48489=DIRECTION('',(0.931242779705752,0.,-0.364399348580517));
#48490=DIRECTION('',(0.150042296859641,0.,-0.988679578606276));
#48491=DIRECTION('',(-0.781200482846105,0.,-0.624280230025758));
#48492=DIRECTION('',(-0.931242779705751,0.,0.364399348580519));
#48493=DIRECTION('',(-0.150042296859647,0.,0.988679578606275));
#48494=DIRECTION('',(0.781200482846104,0.,0.624280230025758));
#48495=DIRECTION('',(0.931242779705752,0.,-0.364399348580517));
#48496=DIRECTION('',(0.150042296859641,0.,-0.988679578606276));
#48497=DIRECTION('',(-0.781200482846105,0.,-0.624280230025758));
#48498=DIRECTION('',(-0.931242779705751,0.,0.364399348580519));
#48499=DIRECTION('',(-0.150042296859647,0.,0.988679578606275));
#48500=DIRECTION('',(0.781200482846104,0.,0.624280230025758));
#48501=DIRECTION('',(0.931242779705752,0.,-0.364399348580517));
#48502=DIRECTION('',(0.150042296859641,0.,-0.988679578606276));
#48503=DIRECTION('',(-0.781200482846105,0.,-0.624280230025758));
#48504=DIRECTION('',(-0.931242779705751,0.,0.364399348580519));
#48505=DIRECTION('',(-0.150042296859647,0.,0.988679578606275));
#48506=DIRECTION('',(0.781200482846104,0.,0.624280230025758));
#48507=DIRECTION('',(0.931242779705752,0.,-0.364399348580517));
#48508=DIRECTION('',(0.150042296859641,0.,-0.988679578606276));
#48509=DIRECTION('',(-0.781200482846105,0.,-0.624280230025758));
#48510=DIRECTION('',(-0.931242779705751,0.,0.364399348580519));
#48511=DIRECTION('',(-0.150042296859647,0.,0.988679578606275));
#48512=DIRECTION('',(0.781200482846104,0.,0.624280230025758));
#48513=DIRECTION('',(0.931242779705752,0.,-0.364399348580517));
#48514=DIRECTION('',(0.150042296859641,0.,-0.988679578606276));
#48515=DIRECTION('',(-0.781200482846105,0.,-0.624280230025758));
#48516=DIRECTION('',(-0.931242779705751,0.,0.364399348580519));
#48517=DIRECTION('',(-0.150042296859647,0.,0.988679578606275));
#48518=DIRECTION('',(0.781200482846104,0.,0.624280230025758));
#48519=DIRECTION('',(0.931242779705752,0.,-0.364399348580517));
#48520=DIRECTION('',(0.150042296859641,0.,-0.988679578606276));
#48521=DIRECTION('',(-0.781200482846105,0.,-0.624280230025758));
#48522=DIRECTION('',(-0.931242779705751,0.,0.364399348580519));
#48523=DIRECTION('',(-0.150042296859647,0.,0.988679578606275));
#48524=DIRECTION('',(0.781200482846104,0.,0.624280230025758));
#48525=DIRECTION('',(0.931242779705752,0.,-0.364399348580517));
#48526=DIRECTION('',(0.150042296859641,0.,-0.988679578606276));
#48527=DIRECTION('',(-0.781200482846105,0.,-0.624280230025758));
#48528=DIRECTION('',(-0.931242779705751,0.,0.364399348580519));
#48529=DIRECTION('',(-0.150042296859647,0.,0.988679578606275));
#48530=DIRECTION('',(0.781200482846104,0.,0.624280230025758));
#48531=DIRECTION('',(0.931242779705752,0.,-0.364399348580517));
#48532=DIRECTION('',(0.150042296859641,0.,-0.988679578606276));
#48533=DIRECTION('',(-0.781200482846105,0.,-0.624280230025758));
#48534=DIRECTION('',(-0.931242779705751,0.,0.364399348580519));
#48535=DIRECTION('',(-0.150042296859647,0.,0.988679578606275));
#48536=DIRECTION('',(0.781200482846104,0.,0.624280230025758));
#48537=DIRECTION('',(0.931242779705752,0.,-0.364399348580517));
#48538=DIRECTION('',(0.150042296859641,0.,-0.988679578606276));
#48539=DIRECTION('',(-0.781200482846105,0.,-0.624280230025758));
#48540=DIRECTION('',(-0.931242779705751,0.,0.364399348580519));
#48541=DIRECTION('',(-0.150042296859647,0.,0.988679578606275));
#48542=DIRECTION('',(0.781200482846104,0.,0.624280230025758));
#48543=DIRECTION('',(0.931242779705752,0.,-0.364399348580517));
#48544=DIRECTION('',(0.150042296859641,0.,-0.988679578606276));
#48545=DIRECTION('',(-0.781200482846105,0.,-0.624280230025758));
#48546=DIRECTION('',(-0.931242779705751,0.,0.364399348580519));
#48547=DIRECTION('',(-0.150042296859647,0.,0.988679578606275));
#48548=DIRECTION('',(0.781200482846104,0.,0.624280230025758));
#48549=DIRECTION('',(0.931242779705752,0.,-0.364399348580517));
#48550=DIRECTION('',(0.150042296859641,0.,-0.988679578606276));
#48551=DIRECTION('',(-0.781200482846105,0.,-0.624280230025758));
#48552=DIRECTION('',(-0.931242779705751,0.,0.364399348580519));
#48553=DIRECTION('',(-0.150042296859647,0.,0.988679578606275));
#48554=DIRECTION('',(0.781200482846104,0.,0.624280230025758));
#48555=DIRECTION('',(0.931242779705752,0.,-0.364399348580517));
#48556=DIRECTION('',(0.150042296859641,0.,-0.988679578606276));
#48557=DIRECTION('',(-0.781200482846105,0.,-0.624280230025758));
#48558=DIRECTION('',(-0.931242779705751,0.,0.364399348580519));
#48559=DIRECTION('',(-0.150042296859647,0.,0.988679578606275));
#48560=DIRECTION('',(0.781200482846104,0.,0.624280230025758));
#48561=DIRECTION('',(0.931242779705752,0.,-0.364399348580517));
#48562=DIRECTION('',(0.150042296859641,0.,-0.988679578606276));
#48563=DIRECTION('',(-0.781200482846105,0.,-0.624280230025758));
#48564=DIRECTION('',(-0.931242779705751,0.,0.364399348580519));
#48565=DIRECTION('',(-0.150042296859647,0.,0.988679578606275));
#48566=DIRECTION('',(0.781200482846104,0.,0.624280230025758));
#48567=DIRECTION('',(0.931242779705752,0.,-0.364399348580517));
#48568=DIRECTION('',(0.150042296859641,0.,-0.988679578606276));
#48569=DIRECTION('',(-0.781200482846105,0.,-0.624280230025758));
#48570=DIRECTION('',(-0.931242779705751,0.,0.364399348580519));
#48571=DIRECTION('',(-0.150042296859647,0.,0.988679578606275));
#48572=DIRECTION('',(0.781200482846104,0.,0.624280230025758));
#48573=DIRECTION('',(0.931242779705752,0.,-0.364399348580517));
#48574=DIRECTION('',(0.150042296859641,0.,-0.988679578606276));
#48575=DIRECTION('',(-0.781200482846105,0.,-0.624280230025758));
#48576=DIRECTION('',(-0.931242779705751,0.,0.364399348580519));
#48577=DIRECTION('',(-0.150042296859647,0.,0.988679578606275));
#48578=DIRECTION('',(0.781200482846104,0.,0.624280230025758));
#48579=DIRECTION('',(0.931242779705752,0.,-0.364399348580517));
#48580=DIRECTION('',(0.150042296859641,0.,-0.988679578606276));
#48581=DIRECTION('',(-0.781200482846105,0.,-0.624280230025758));
#48582=DIRECTION('',(-0.931242779705751,0.,0.364399348580519));
#48583=DIRECTION('',(-0.150042296859647,0.,0.988679578606275));
#48584=DIRECTION('',(0.781200482846104,0.,0.624280230025758));
#48585=DIRECTION('',(0.931242779705752,0.,-0.364399348580517));
#48586=DIRECTION('',(0.150042296859641,0.,-0.988679578606276));
#48587=DIRECTION('',(-0.781200482846105,0.,-0.624280230025758));
#48588=DIRECTION('',(-0.931242779705751,0.,0.364399348580519));
#48589=DIRECTION('',(-0.150042296859647,0.,0.988679578606275));
#48590=DIRECTION('',(0.781200482846104,0.,0.624280230025758));
#48591=DIRECTION('',(0.931242779705752,0.,-0.364399348580517));
#48592=DIRECTION('',(0.150042296859641,0.,-0.988679578606276));
#48593=DIRECTION('',(-0.781200482846105,0.,-0.624280230025758));
#48594=DIRECTION('',(-0.931242779705751,0.,0.364399348580519));
#48595=DIRECTION('',(-0.150042296859647,0.,0.988679578606275));
#48596=DIRECTION('',(0.781200482846104,0.,0.624280230025758));
#48597=DIRECTION('',(0.931242779705752,0.,-0.364399348580517));
#48598=DIRECTION('',(0.150042296859641,0.,-0.988679578606276));
#48599=DIRECTION('',(-0.781200482846105,0.,-0.624280230025758));
#48600=DIRECTION('',(-0.931242779705751,0.,0.364399348580519));
#48601=DIRECTION('',(-0.150042296859647,0.,0.988679578606275));
#48602=DIRECTION('',(0.781200482846104,0.,0.624280230025758));
#48603=DIRECTION('',(0.931242779705752,0.,-0.364399348580517));
#48604=DIRECTION('',(0.150042296859641,0.,-0.988679578606276));
#48605=DIRECTION('',(-0.781200482846105,0.,-0.624280230025758));
#48606=DIRECTION('',(-0.931242779705751,0.,0.364399348580519));
#48607=DIRECTION('',(-0.150042296859647,0.,0.988679578606275));
#48608=DIRECTION('',(0.781200482846104,0.,0.624280230025758));
#48609=DIRECTION('',(0.931242779705752,0.,-0.364399348580517));
#48610=DIRECTION('',(0.150042296859641,0.,-0.988679578606276));
#48611=DIRECTION('',(-0.781200482846105,0.,-0.624280230025758));
#48612=DIRECTION('',(-0.931242779705751,0.,0.364399348580519));
#48613=DIRECTION('',(-0.150042296859647,0.,0.988679578606275));
#48614=DIRECTION('',(0.781200482846104,0.,0.624280230025758));
#48615=DIRECTION('',(0.931242779705752,0.,-0.364399348580517));
#48616=DIRECTION('',(0.150042296859641,0.,-0.988679578606276));
#48617=DIRECTION('',(-0.781200482846105,0.,-0.624280230025758));
#48618=DIRECTION('',(-0.931242779705751,0.,0.364399348580519));
#48619=DIRECTION('',(-0.150042296859647,0.,0.988679578606275));
#48620=DIRECTION('',(0.781200482846104,0.,0.624280230025758));
#48621=DIRECTION('',(0.931242779705752,0.,-0.364399348580517));
#48622=DIRECTION('',(0.150042296859641,0.,-0.988679578606276));
#48623=DIRECTION('',(-0.781200482846105,0.,-0.624280230025758));
#48624=DIRECTION('',(-0.931242779705751,0.,0.364399348580519));
#48625=DIRECTION('',(-0.150042296859647,0.,0.988679578606275));
#48626=DIRECTION('',(0.781200482846104,0.,0.624280230025758));
#48627=DIRECTION('',(0.931242779705752,0.,-0.364399348580517));
#48628=DIRECTION('',(0.150042296859641,0.,-0.988679578606276));
#48629=DIRECTION('',(-0.781200482846105,0.,-0.624280230025758));
#48630=DIRECTION('',(-0.931242779705751,0.,0.364399348580519));
#48631=DIRECTION('',(-0.150042296859647,0.,0.988679578606275));
#48632=DIRECTION('',(0.781200482846104,0.,0.624280230025758));
#48633=DIRECTION('',(0.931242779705752,0.,-0.364399348580517));
#48634=DIRECTION('',(0.150042296859641,0.,-0.988679578606276));
#48635=DIRECTION('',(-0.781200482846105,0.,-0.624280230025758));
#48636=DIRECTION('',(-0.931242779705751,0.,0.364399348580519));
#48637=DIRECTION('',(-0.150042296859647,0.,0.988679578606275));
#48638=DIRECTION('',(0.781200482846104,0.,0.624280230025758));
#48639=DIRECTION('',(0.931242779705752,0.,-0.364399348580517));
#48640=DIRECTION('',(0.150042296859641,0.,-0.988679578606276));
#48641=DIRECTION('',(-0.781200482846105,0.,-0.624280230025758));
#48642=DIRECTION('',(-0.931242779705751,0.,0.364399348580519));
#48643=DIRECTION('',(-0.150042296859647,0.,0.988679578606275));
#48644=DIRECTION('',(0.781200482846104,0.,0.624280230025758));
#48645=DIRECTION('',(0.931242779705752,0.,-0.364399348580517));
#48646=DIRECTION('',(0.150042296859641,0.,-0.988679578606276));
#48647=DIRECTION('',(-0.781200482846105,0.,-0.624280230025758));
#48648=DIRECTION('',(-0.931242779705751,0.,0.364399348580519));
#48649=DIRECTION('',(-0.150042296859647,0.,0.988679578606275));
#48650=DIRECTION('',(0.781200482846104,0.,0.624280230025758));
#48651=DIRECTION('',(0.931242779705752,0.,-0.364399348580517));
#48652=DIRECTION('',(0.150042296859641,0.,-0.988679578606276));
#48653=DIRECTION('',(-0.781200482846105,0.,-0.624280230025758));
#48654=DIRECTION('',(-0.931242779705751,0.,0.364399348580519));
#48655=DIRECTION('',(-0.150042296859647,0.,0.988679578606275));
#48656=DIRECTION('',(0.781200482846104,0.,0.624280230025758));
#48657=DIRECTION('',(0.931242779705752,0.,-0.364399348580517));
#48658=DIRECTION('',(0.150042296859641,0.,-0.988679578606276));
#48659=DIRECTION('',(-0.781200482846105,0.,-0.624280230025758));
#48660=DIRECTION('',(-0.931242779705751,0.,0.364399348580519));
#48661=DIRECTION('',(-0.150042296859647,0.,0.988679578606275));
#48662=DIRECTION('',(0.781200482846104,0.,0.624280230025758));
#48663=DIRECTION('',(0.931242779705752,0.,-0.364399348580517));
#48664=DIRECTION('',(0.150042296859641,0.,-0.988679578606276));
#48665=DIRECTION('',(-0.781200482846105,0.,-0.624280230025758));
#48666=DIRECTION('',(-0.931242779705751,0.,0.364399348580519));
#48667=DIRECTION('',(-0.150042296859647,0.,0.988679578606275));
#48668=DIRECTION('',(0.781200482846104,0.,0.624280230025758));
#48669=DIRECTION('',(0.931242779705752,0.,-0.364399348580517));
#48670=DIRECTION('',(0.150042296859641,0.,-0.988679578606276));
#48671=DIRECTION('',(-0.781200482846105,0.,-0.624280230025758));
#48672=DIRECTION('',(-0.931242779705751,0.,0.364399348580519));
#48673=DIRECTION('',(-0.150042296859647,0.,0.988679578606275));
#48674=DIRECTION('',(0.781200482846104,0.,0.624280230025758));
#48675=DIRECTION('',(0.931242779705752,0.,-0.364399348580517));
#48676=DIRECTION('',(0.150042296859641,0.,-0.988679578606276));
#48677=DIRECTION('',(-0.781200482846105,0.,-0.624280230025758));
#48678=DIRECTION('',(-0.931242779705751,0.,0.364399348580519));
#48679=DIRECTION('',(-0.150042296859647,0.,0.988679578606275));
#48680=DIRECTION('',(0.781200482846104,0.,0.624280230025758));
#48681=DIRECTION('',(0.931242779705752,0.,-0.364399348580517));
#48682=DIRECTION('',(0.150042296859641,0.,-0.988679578606276));
#48683=DIRECTION('',(-0.781200482846105,0.,-0.624280230025758));
#48684=DIRECTION('',(-0.931242779705751,0.,0.364399348580519));
#48685=DIRECTION('',(-0.150042296859647,0.,0.988679578606275));
#48686=DIRECTION('',(0.781200482846104,0.,0.624280230025758));
#48687=DIRECTION('',(0.931242779705752,0.,-0.364399348580517));
#48688=DIRECTION('',(0.150042296859641,0.,-0.988679578606276));
#48689=DIRECTION('',(-0.781200482846105,0.,-0.624280230025758));
#48690=DIRECTION('',(-0.931242779705751,0.,0.364399348580519));
#48691=DIRECTION('',(-0.150042296859647,0.,0.988679578606275));
#48692=DIRECTION('',(0.781200482846104,0.,0.624280230025758));
#48693=DIRECTION('',(0.931242779705752,0.,-0.364399348580517));
#48694=DIRECTION('',(0.150042296859641,0.,-0.988679578606276));
#48695=DIRECTION('',(-0.781200482846105,0.,-0.624280230025758));
#48696=DIRECTION('',(-0.931242779705751,0.,0.364399348580519));
#48697=DIRECTION('',(-0.150042296859647,0.,0.988679578606275));
#48698=DIRECTION('',(0.781200482846104,0.,0.624280230025758));
#48699=DIRECTION('',(0.931242779705752,0.,-0.364399348580517));
#48700=DIRECTION('',(0.150042296859641,0.,-0.988679578606276));
#48701=DIRECTION('',(-0.781200482846105,0.,-0.624280230025758));
#48702=DIRECTION('',(-0.931242779705751,0.,0.364399348580519));
#48703=DIRECTION('',(-0.150042296859647,0.,0.988679578606275));
#48704=DIRECTION('',(0.781200482846104,0.,0.624280230025758));
#48705=DIRECTION('',(0.931242779705752,0.,-0.364399348580517));
#48706=DIRECTION('',(0.150042296859641,0.,-0.988679578606276));
#48707=DIRECTION('',(-0.781200482846105,0.,-0.624280230025758));
#48708=DIRECTION('',(-0.931242779705751,0.,0.364399348580519));
#48709=DIRECTION('',(-0.150042296859647,0.,0.988679578606275));
#48710=DIRECTION('',(0.781200482846104,0.,0.624280230025758));
#48711=DIRECTION('',(0.931242779705752,0.,-0.364399348580517));
#48712=DIRECTION('',(0.150042296859641,0.,-0.988679578606276));
#48713=DIRECTION('',(-0.781200482846105,0.,-0.624280230025758));
#48714=DIRECTION('',(-0.931242779705751,0.,0.364399348580519));
#48715=DIRECTION('',(-0.150042296859647,0.,0.988679578606275));
#48716=DIRECTION('',(0.781200482846104,0.,0.624280230025758));
#48717=DIRECTION('',(0.931242779705752,0.,-0.364399348580517));
#48718=DIRECTION('',(0.150042296859641,0.,-0.988679578606276));
#48719=DIRECTION('',(-0.781200482846105,0.,-0.624280230025758));
#48720=DIRECTION('',(-0.931242779705751,0.,0.364399348580519));
#48721=DIRECTION('',(-0.150042296859647,0.,0.988679578606275));
#48722=DIRECTION('',(0.781200482846104,0.,0.624280230025758));
#48723=DIRECTION('',(0.931242779705752,0.,-0.364399348580517));
#48724=DIRECTION('',(0.150042296859641,0.,-0.988679578606276));
#48725=DIRECTION('',(-0.781200482846105,0.,-0.624280230025758));
#48726=DIRECTION('',(-0.931242779705751,0.,0.364399348580519));
#48727=DIRECTION('',(-0.150042296859647,0.,0.988679578606275));
#48728=DIRECTION('',(0.781200482846104,0.,0.624280230025758));
#48729=DIRECTION('',(0.931242779705752,0.,-0.364399348580517));
#48730=DIRECTION('',(0.150042296859641,0.,-0.988679578606276));
#48731=DIRECTION('',(-0.781200482846105,0.,-0.624280230025758));
#48732=DIRECTION('',(-0.931242779705751,0.,0.364399348580519));
#48733=DIRECTION('',(-0.150042296859647,0.,0.988679578606275));
#48734=DIRECTION('',(0.781200482846104,0.,0.624280230025758));
#48735=DIRECTION('',(0.931242779705752,0.,-0.364399348580517));
#48736=DIRECTION('',(0.150042296859641,0.,-0.988679578606276));
#48737=DIRECTION('',(-0.781200482846105,0.,-0.624280230025758));
#48738=DIRECTION('',(-0.931242779705751,0.,0.364399348580519));
#48739=DIRECTION('',(-0.150042296859647,0.,0.988679578606275));
#48740=DIRECTION('',(0.781200482846104,0.,0.624280230025758));
#48741=DIRECTION('',(0.931242779705752,0.,-0.364399348580517));
#48742=DIRECTION('',(0.150042296859641,0.,-0.988679578606276));
#48743=DIRECTION('',(-0.781200482846105,0.,-0.624280230025758));
#48744=DIRECTION('',(-0.931242779705751,0.,0.364399348580519));
#48745=DIRECTION('',(-0.150042296859647,0.,0.988679578606275));
#48746=DIRECTION('',(0.781200482846104,0.,0.624280230025758));
#48747=DIRECTION('',(0.931242779705752,0.,-0.364399348580517));
#48748=DIRECTION('',(0.150042296859641,0.,-0.988679578606276));
#48749=DIRECTION('',(-0.781200482846105,0.,-0.624280230025758));
#48750=DIRECTION('',(-0.931242779705751,0.,0.364399348580519));
#48751=DIRECTION('',(-0.150042296859647,0.,0.988679578606275));
#48752=DIRECTION('',(0.781200482846104,0.,0.624280230025758));
#48753=DIRECTION('',(0.931242779705752,0.,-0.364399348580517));
#48754=DIRECTION('',(0.150042296859641,0.,-0.988679578606276));
#48755=DIRECTION('',(-0.781200482846105,0.,-0.624280230025758));
#48756=DIRECTION('',(-0.931242779705751,0.,0.364399348580519));
#48757=DIRECTION('',(-0.150042296859647,0.,0.988679578606275));
#48758=DIRECTION('',(0.781200482846104,0.,0.624280230025758));
#48759=DIRECTION('',(0.931242779705752,0.,-0.364399348580517));
#48760=DIRECTION('',(0.150042296859641,0.,-0.988679578606276));
#48761=DIRECTION('',(-0.781200482846105,0.,-0.624280230025758));
#48762=DIRECTION('',(-0.931242779705751,0.,0.364399348580519));
#48763=DIRECTION('',(-0.150042296859647,0.,0.988679578606275));
#48764=DIRECTION('',(0.781200482846104,0.,0.624280230025758));
#48765=DIRECTION('',(0.931242779705752,0.,-0.364399348580517));
#48766=DIRECTION('',(0.150042296859641,0.,-0.988679578606276));
#48767=DIRECTION('',(-0.781200482846105,0.,-0.624280230025758));
#48768=DIRECTION('',(-0.931242779705751,0.,0.364399348580519));
#48769=DIRECTION('',(-0.150042296859647,0.,0.988679578606275));
#48770=DIRECTION('',(0.781200482846104,0.,0.624280230025758));
#48771=DIRECTION('',(0.931242779705752,0.,-0.364399348580517));
#48772=DIRECTION('',(0.150042296859641,0.,-0.988679578606276));
#48773=DIRECTION('',(-0.781200482846105,0.,-0.624280230025758));
#48774=DIRECTION('',(-0.931242779705751,0.,0.364399348580519));
#48775=DIRECTION('',(-0.150042296859647,0.,0.988679578606275));
#48776=DIRECTION('',(0.781200482846104,0.,0.624280230025758));
#48777=DIRECTION('',(0.931242779705752,0.,-0.364399348580517));
#48778=DIRECTION('',(0.150042296859641,0.,-0.988679578606276));
#48779=DIRECTION('',(-0.781200482846105,0.,-0.624280230025758));
#48780=DIRECTION('',(-0.931242779705751,0.,0.364399348580519));
#48781=DIRECTION('',(-0.150042296859647,0.,0.988679578606275));
#48782=DIRECTION('',(0.781200482846104,0.,0.624280230025758));
#48783=DIRECTION('',(0.931242779705752,0.,-0.364399348580517));
#48784=DIRECTION('',(0.150042296859641,0.,-0.988679578606276));
#48785=DIRECTION('',(-0.781200482846105,0.,-0.624280230025758));
#48786=DIRECTION('',(-0.931242779705751,0.,0.364399348580519));
#48787=DIRECTION('',(-0.150042296859647,0.,0.988679578606275));
#48788=DIRECTION('',(0.781200482846104,0.,0.624280230025758));
#48789=DIRECTION('',(0.931242779705752,0.,-0.364399348580517));
#48790=DIRECTION('',(0.150042296859641,0.,-0.988679578606276));
#48791=DIRECTION('',(-0.781200482846105,0.,-0.624280230025758));
#48792=DIRECTION('',(-0.931242779705751,0.,0.364399348580519));
#48793=DIRECTION('',(-0.150042296859647,0.,0.988679578606275));
#48794=DIRECTION('',(0.781200482846104,0.,0.624280230025758));
#48795=DIRECTION('',(0.931242779705752,0.,-0.364399348580517));
#48796=DIRECTION('',(0.150042296859641,0.,-0.988679578606276));
#48797=DIRECTION('',(-0.781200482846105,0.,-0.624280230025758));
#48798=DIRECTION('',(-0.931242779705751,0.,0.364399348580519));
#48799=DIRECTION('',(-0.150042296859647,0.,0.988679578606275));
#48800=DIRECTION('',(0.781200482846104,0.,0.624280230025758));
#48801=DIRECTION('',(0.931242779705752,0.,-0.364399348580517));
#48802=DIRECTION('',(0.150042296859641,0.,-0.988679578606276));
#48803=DIRECTION('',(-0.781200482846105,0.,-0.624280230025758));
#48804=DIRECTION('',(-0.931242779705751,0.,0.364399348580519));
#48805=DIRECTION('',(-0.150042296859647,0.,0.988679578606275));
#48806=DIRECTION('',(0.781200482846104,0.,0.624280230025758));
#48807=DIRECTION('',(0.931242779705752,0.,-0.364399348580517));
#48808=DIRECTION('',(0.150042296859641,0.,-0.988679578606276));
#48809=DIRECTION('',(-0.781200482846105,0.,-0.624280230025758));
#48810=DIRECTION('',(-0.931242779705751,0.,0.364399348580519));
#48811=DIRECTION('',(-0.150042296859647,0.,0.988679578606275));
#48812=DIRECTION('',(0.781200482846104,0.,0.624280230025758));
#48813=DIRECTION('',(0.931242779705752,0.,-0.364399348580517));
#48814=DIRECTION('',(0.150042296859641,0.,-0.988679578606276));
#48815=DIRECTION('',(-0.781200482846105,0.,-0.624280230025758));
#48816=DIRECTION('',(-0.931242779705751,0.,0.364399348580519));
#48817=DIRECTION('',(-0.150042296859647,0.,0.988679578606275));
#48818=DIRECTION('',(0.781200482846104,0.,0.624280230025758));
#48819=DIRECTION('',(0.931242779705752,0.,-0.364399348580517));
#48820=DIRECTION('',(0.150042296859641,0.,-0.988679578606276));
#48821=DIRECTION('',(-0.781200482846105,0.,-0.624280230025758));
#48822=DIRECTION('',(-0.931242779705751,0.,0.364399348580519));
#48823=DIRECTION('',(-0.150042296859647,0.,0.988679578606275));
#48824=DIRECTION('',(0.781200482846104,0.,0.624280230025758));
#48825=DIRECTION('',(0.931242779705752,0.,-0.364399348580517));
#48826=DIRECTION('',(0.150042296859641,0.,-0.988679578606276));
#48827=DIRECTION('',(-0.781200482846105,0.,-0.624280230025758));
#48828=DIRECTION('',(-0.931242779705751,0.,0.364399348580519));
#48829=DIRECTION('',(-0.150042296859647,0.,0.988679578606275));
#48830=DIRECTION('',(0.781200482846104,0.,0.624280230025758));
#48831=DIRECTION('',(0.931242779705752,0.,-0.364399348580517));
#48832=DIRECTION('',(0.150042296859641,0.,-0.988679578606276));
#48833=DIRECTION('',(-0.781200482846105,0.,-0.624280230025758));
#48834=DIRECTION('',(-0.931242779705751,0.,0.364399348580519));
#48835=DIRECTION('',(-0.150042296859647,0.,0.988679578606275));
#48836=DIRECTION('',(0.781200482846104,0.,0.624280230025758));
#48837=DIRECTION('',(0.931242779705752,0.,-0.364399348580517));
#48838=DIRECTION('',(0.150042296859641,0.,-0.988679578606276));
#48839=DIRECTION('',(-0.781200482846105,0.,-0.624280230025758));
#48840=DIRECTION('',(-0.931242779705751,0.,0.364399348580519));
#48841=DIRECTION('',(-0.150042296859647,0.,0.988679578606275));
#48842=DIRECTION('',(0.781200482846104,0.,0.624280230025758));
#48843=DIRECTION('',(0.931242779705752,0.,-0.364399348580517));
#48844=DIRECTION('',(0.150042296859641,0.,-0.988679578606276));
#48845=DIRECTION('',(-0.781200482846105,0.,-0.624280230025758));
#48846=DIRECTION('',(-0.931242779705751,0.,0.364399348580519));
#48847=DIRECTION('',(-0.150042296859647,0.,0.988679578606275));
#48848=DIRECTION('',(0.781200482846104,0.,0.624280230025758));
#48849=DIRECTION('',(0.931242779705752,0.,-0.364399348580517));
#48850=DIRECTION('',(0.150042296859641,0.,-0.988679578606276));
#48851=DIRECTION('',(-0.781200482846105,0.,-0.624280230025758));
#48852=DIRECTION('',(-0.931242779705751,0.,0.364399348580519));
#48853=DIRECTION('',(-0.150042296859647,0.,0.988679578606275));
#48854=DIRECTION('',(0.781200482846104,0.,0.624280230025758));
#48855=DIRECTION('',(0.931242779705752,0.,-0.364399348580517));
#48856=DIRECTION('',(0.150042296859641,0.,-0.988679578606276));
#48857=DIRECTION('',(-0.781200482846105,0.,-0.624280230025758));
#48858=DIRECTION('',(-0.931242779705751,0.,0.364399348580519));
#48859=DIRECTION('',(-0.150042296859647,0.,0.988679578606275));
#48860=DIRECTION('',(0.781200482846104,0.,0.624280230025758));
#48861=DIRECTION('',(0.931242779705752,0.,-0.364399348580517));
#48862=DIRECTION('',(0.150042296859641,0.,-0.988679578606276));
#48863=DIRECTION('',(-0.781200482846105,0.,-0.624280230025758));
#48864=DIRECTION('',(-0.931242779705751,0.,0.364399348580519));
#48865=DIRECTION('',(-0.150042296859647,0.,0.988679578606275));
#48866=DIRECTION('',(0.781200482846104,0.,0.624280230025758));
#48867=DIRECTION('',(0.931242779705752,0.,-0.364399348580517));
#48868=DIRECTION('',(0.150042296859641,0.,-0.988679578606276));
#48869=DIRECTION('',(-0.781200482846105,0.,-0.624280230025758));
#48870=DIRECTION('',(-0.931242779705751,0.,0.364399348580519));
#48871=DIRECTION('',(-0.150042296859647,0.,0.988679578606275));
#48872=DIRECTION('',(0.781200482846104,0.,0.624280230025758));
#48873=DIRECTION('',(0.931242779705752,0.,-0.364399348580517));
#48874=DIRECTION('',(0.150042296859641,0.,-0.988679578606276));
#48875=DIRECTION('',(-0.781200482846105,0.,-0.624280230025758));
#48876=DIRECTION('',(-0.931242779705751,0.,0.364399348580519));
#48877=DIRECTION('',(-0.150042296859647,0.,0.988679578606275));
#48878=DIRECTION('',(0.781200482846104,0.,0.624280230025758));
#48879=DIRECTION('',(0.931242779705752,0.,-0.364399348580517));
#48880=DIRECTION('',(0.150042296859641,0.,-0.988679578606276));
#48881=DIRECTION('',(-0.781200482846105,0.,-0.624280230025758));
#48882=DIRECTION('',(-0.931242779705751,0.,0.364399348580519));
#48883=DIRECTION('',(-0.150042296859647,0.,0.988679578606275));
#48884=DIRECTION('',(0.781200482846104,0.,0.624280230025758));
#48885=DIRECTION('',(0.931242779705752,0.,-0.364399348580517));
#48886=DIRECTION('',(0.150042296859641,0.,-0.988679578606276));
#48887=DIRECTION('',(-0.781200482846105,0.,-0.624280230025758));
#48888=DIRECTION('',(-0.931242779705751,0.,0.364399348580519));
#48889=DIRECTION('',(-0.150042296859647,0.,0.988679578606275));
#48890=DIRECTION('',(0.781200482846104,0.,0.624280230025758));
#48891=DIRECTION('',(0.931242779705752,0.,-0.364399348580517));
#48892=DIRECTION('',(0.150042296859641,0.,-0.988679578606276));
#48893=DIRECTION('',(-0.781200482846105,0.,-0.624280230025758));
#48894=DIRECTION('',(-0.931242779705751,0.,0.364399348580519));
#48895=DIRECTION('',(-0.150042296859647,0.,0.988679578606275));
#48896=DIRECTION('',(0.781200482846104,0.,0.624280230025758));
#48897=DIRECTION('',(0.931242779705752,0.,-0.364399348580517));
#48898=DIRECTION('',(0.150042296859641,0.,-0.988679578606276));
#48899=DIRECTION('',(-0.781200482846105,0.,-0.624280230025758));
#48900=DIRECTION('',(-0.931242779705751,0.,0.364399348580519));
#48901=DIRECTION('',(-0.150042296859647,0.,0.988679578606275));
#48902=DIRECTION('',(0.781200482846104,0.,0.624280230025758));
#48903=DIRECTION('',(0.931242779705752,0.,-0.364399348580517));
#48904=DIRECTION('',(0.150042296859641,0.,-0.988679578606276));
#48905=DIRECTION('',(-0.781200482846105,0.,-0.624280230025758));
#48906=DIRECTION('',(-0.931242779705751,0.,0.364399348580519));
#48907=DIRECTION('',(-0.150042296859647,0.,0.988679578606275));
#48908=DIRECTION('',(0.781200482846104,0.,0.624280230025758));
#48909=DIRECTION('',(0.931242779705752,0.,-0.364399348580517));
#48910=DIRECTION('',(0.150042296859641,0.,-0.988679578606276));
#48911=DIRECTION('',(-0.781200482846105,0.,-0.624280230025758));
#48912=DIRECTION('',(-0.931242779705751,0.,0.364399348580519));
#48913=DIRECTION('',(-0.150042296859647,0.,0.988679578606275));
#48914=DIRECTION('',(0.781200482846104,0.,0.624280230025758));
#48915=DIRECTION('',(0.931242779705752,0.,-0.364399348580517));
#48916=DIRECTION('',(0.150042296859641,0.,-0.988679578606276));
#48917=DIRECTION('',(-0.781200482846105,0.,-0.624280230025758));
#48918=DIRECTION('',(-0.931242779705751,0.,0.364399348580519));
#48919=DIRECTION('',(-0.150042296859647,0.,0.988679578606275));
#48920=DIRECTION('',(0.781200482846104,0.,0.624280230025758));
#48921=DIRECTION('',(0.931242779705752,0.,-0.364399348580517));
#48922=DIRECTION('',(0.150042296859641,0.,-0.988679578606276));
#48923=DIRECTION('',(-0.781200482846105,0.,-0.624280230025758));
#48924=DIRECTION('',(-0.931242779705751,0.,0.364399348580519));
#48925=DIRECTION('',(-0.150042296859647,0.,0.988679578606275));
#48926=DIRECTION('',(0.781200482846104,0.,0.624280230025758));
#48927=DIRECTION('',(0.931242779705752,0.,-0.364399348580517));
#48928=DIRECTION('',(0.150042296859641,0.,-0.988679578606276));
#48929=DIRECTION('',(-0.781200482846105,0.,-0.624280230025758));
#48930=DIRECTION('',(-0.931242779705751,0.,0.364399348580519));
#48931=DIRECTION('',(-0.150042296859647,0.,0.988679578606275));
#48932=DIRECTION('',(0.781200482846104,0.,0.624280230025758));
#48933=DIRECTION('',(0.931242779705752,0.,-0.364399348580517));
#48934=DIRECTION('',(0.150042296859641,0.,-0.988679578606276));
#48935=DIRECTION('',(-0.781200482846105,0.,-0.624280230025758));
#48936=DIRECTION('',(-0.931242779705751,0.,0.364399348580519));
#48937=DIRECTION('',(-0.150042296859647,0.,0.988679578606275));
#48938=DIRECTION('',(0.781200482846104,0.,0.624280230025758));
#48939=DIRECTION('',(0.931242779705752,0.,-0.364399348580517));
#48940=DIRECTION('',(0.150042296859641,0.,-0.988679578606276));
#48941=DIRECTION('',(-0.781200482846105,0.,-0.624280230025758));
#48942=DIRECTION('',(-0.931242779705751,0.,0.364399348580519));
#48943=DIRECTION('',(-0.150042296859647,0.,0.988679578606275));
#48944=DIRECTION('',(0.781200482846104,0.,0.624280230025758));
#48945=DIRECTION('',(0.931242779705752,0.,-0.364399348580517));
#48946=DIRECTION('',(0.150042296859641,0.,-0.988679578606276));
#48947=DIRECTION('',(-0.781200482846105,0.,-0.624280230025758));
#48948=DIRECTION('',(-0.931242779705751,0.,0.364399348580519));
#48949=DIRECTION('',(-0.150042296859647,0.,0.988679578606275));
#48950=DIRECTION('',(0.781200482846104,0.,0.624280230025758));
#48951=DIRECTION('',(0.931242779705752,0.,-0.364399348580517));
#48952=DIRECTION('',(0.150042296859641,0.,-0.988679578606276));
#48953=DIRECTION('',(-0.781200482846105,0.,-0.624280230025758));
#48954=DIRECTION('',(-0.931242779705751,0.,0.364399348580519));
#48955=DIRECTION('',(-0.150042296859647,0.,0.988679578606275));
#48956=DIRECTION('',(0.781200482846104,0.,0.624280230025758));
#48957=DIRECTION('',(0.931242779705752,0.,-0.364399348580517));
#48958=DIRECTION('',(0.150042296859641,0.,-0.988679578606276));
#48959=DIRECTION('',(-0.781200482846105,0.,-0.624280230025758));
#48960=DIRECTION('',(-0.931242779705751,0.,0.364399348580519));
#48961=DIRECTION('',(-0.150042296859647,0.,0.988679578606275));
#48962=DIRECTION('',(0.781200482846104,0.,0.624280230025758));
#48963=DIRECTION('',(0.931242779705752,0.,-0.364399348580517));
#48964=DIRECTION('',(0.150042296859641,0.,-0.988679578606276));
#48965=DIRECTION('',(-0.781200482846105,0.,-0.624280230025758));
#48966=DIRECTION('',(-0.931242779705751,0.,0.364399348580519));
#48967=DIRECTION('',(-0.150042296859647,0.,0.988679578606275));
#48968=DIRECTION('',(0.781200482846104,0.,0.624280230025758));
#48969=DIRECTION('',(0.931242779705752,0.,-0.364399348580517));
#48970=DIRECTION('',(0.150042296859641,0.,-0.988679578606276));
#48971=DIRECTION('',(-0.781200482846105,0.,-0.624280230025758));
#48972=DIRECTION('',(-0.931242779705751,0.,0.364399348580519));
#48973=DIRECTION('',(-0.150042296859647,0.,0.988679578606275));
#48974=DIRECTION('',(0.781200482846104,0.,0.624280230025758));
#48975=DIRECTION('',(0.931242779705752,0.,-0.364399348580517));
#48976=DIRECTION('',(0.150042296859641,0.,-0.988679578606276));
#48977=DIRECTION('',(-0.781200482846105,0.,-0.624280230025758));
#48978=DIRECTION('',(-0.931242779705751,0.,0.364399348580519));
#48979=DIRECTION('',(-0.150042296859647,0.,0.988679578606275));
#48980=DIRECTION('',(0.781200482846104,0.,0.624280230025758));
#48981=DIRECTION('',(0.931242779705752,0.,-0.364399348580517));
#48982=DIRECTION('',(0.150042296859641,0.,-0.988679578606276));
#48983=DIRECTION('',(-0.781200482846105,0.,-0.624280230025758));
#48984=DIRECTION('',(-0.931242779705751,0.,0.364399348580519));
#48985=DIRECTION('',(-0.150042296859647,0.,0.988679578606275));
#48986=DIRECTION('',(0.781200482846104,0.,0.624280230025758));
#48987=DIRECTION('',(0.931242779705752,0.,-0.364399348580517));
#48988=DIRECTION('',(0.150042296859641,0.,-0.988679578606276));
#48989=DIRECTION('',(-0.781200482846105,0.,-0.624280230025758));
#48990=DIRECTION('',(-0.931242779705751,0.,0.364399348580519));
#48991=DIRECTION('',(-0.150042296859647,0.,0.988679578606275));
#48992=DIRECTION('',(0.781200482846104,0.,0.624280230025758));
#48993=DIRECTION('',(0.931242779705752,0.,-0.364399348580517));
#48994=DIRECTION('',(0.150042296859641,0.,-0.988679578606276));
#48995=DIRECTION('',(-0.781200482846105,0.,-0.624280230025758));
#48996=DIRECTION('',(-0.931242779705751,0.,0.364399348580519));
#48997=DIRECTION('',(-0.150042296859647,0.,0.988679578606275));
#48998=DIRECTION('',(0.781200482846104,0.,0.624280230025758));
#48999=DIRECTION('',(0.931242779705752,0.,-0.364399348580517));
#49000=DIRECTION('',(0.150042296859641,0.,-0.988679578606276));
#49001=DIRECTION('',(-0.781200482846105,0.,-0.624280230025758));
#49002=DIRECTION('',(-0.931242779705751,0.,0.364399348580519));
#49003=DIRECTION('',(-0.150042296859647,0.,0.988679578606275));
#49004=DIRECTION('',(0.781200482846104,0.,0.624280230025758));
#49005=DIRECTION('',(0.931242779705752,0.,-0.364399348580517));
#49006=DIRECTION('',(0.150042296859641,0.,-0.988679578606276));
#49007=DIRECTION('',(-0.781200482846105,0.,-0.624280230025758));
#49008=DIRECTION('',(-0.931242779705751,0.,0.364399348580519));
#49009=DIRECTION('',(-0.150042296859647,0.,0.988679578606275));
#49010=DIRECTION('',(0.781200482846104,0.,0.624280230025758));
#49011=DIRECTION('',(0.931242779705752,0.,-0.364399348580517));
#49012=DIRECTION('',(0.150042296859641,0.,-0.988679578606276));
#49013=DIRECTION('',(-0.781200482846105,0.,-0.624280230025758));
#49014=DIRECTION('',(-0.931242779705751,0.,0.364399348580519));
#49015=DIRECTION('',(-0.150042296859647,0.,0.988679578606275));
#49016=DIRECTION('',(0.781200482846104,0.,0.624280230025758));
#49017=DIRECTION('',(0.931242779705752,0.,-0.364399348580517));
#49018=DIRECTION('',(0.150042296859641,0.,-0.988679578606276));
#49019=DIRECTION('',(-0.781200482846105,0.,-0.624280230025758));
#49020=DIRECTION('',(-0.931242779705751,0.,0.364399348580519));
#49021=DIRECTION('',(-0.150042296859647,0.,0.988679578606275));
#49022=DIRECTION('',(0.781200482846104,0.,0.624280230025758));
#49023=DIRECTION('',(0.931242779705752,0.,-0.364399348580517));
#49024=DIRECTION('',(0.150042296859641,0.,-0.988679578606276));
#49025=DIRECTION('',(-0.781200482846105,0.,-0.624280230025758));
#49026=DIRECTION('',(-0.931242779705751,0.,0.364399348580519));
#49027=DIRECTION('',(-0.150042296859647,0.,0.988679578606275));
#49028=DIRECTION('',(0.781200482846104,0.,0.624280230025758));
#49029=DIRECTION('',(0.931242779705752,0.,-0.364399348580517));
#49030=DIRECTION('',(0.150042296859641,0.,-0.988679578606276));
#49031=DIRECTION('',(-0.781200482846105,0.,-0.624280230025758));
#49032=DIRECTION('',(-0.931242779705751,0.,0.364399348580519));
#49033=DIRECTION('',(-0.150042296859647,0.,0.988679578606275));
#49034=DIRECTION('',(0.781200482846104,0.,0.624280230025758));
#49035=DIRECTION('',(0.931242779705752,0.,-0.364399348580517));
#49036=DIRECTION('',(0.150042296859641,0.,-0.988679578606276));
#49037=DIRECTION('',(-0.781200482846105,0.,-0.624280230025758));
#49038=DIRECTION('',(-0.931242779705751,0.,0.364399348580519));
#49039=DIRECTION('',(-0.150042296859647,0.,0.988679578606275));
#49040=DIRECTION('',(0.781200482846104,0.,0.624280230025758));
#49041=DIRECTION('',(0.931242779705752,0.,-0.364399348580517));
#49042=DIRECTION('',(0.150042296859641,0.,-0.988679578606276));
#49043=DIRECTION('',(-0.781200482846105,0.,-0.624280230025758));
#49044=DIRECTION('',(-0.931242779705751,0.,0.364399348580519));
#49045=DIRECTION('',(-0.150042296859647,0.,0.988679578606275));
#49046=DIRECTION('',(0.781200482846104,0.,0.624280230025758));
#49047=DIRECTION('',(0.931242779705752,0.,-0.364399348580517));
#49048=DIRECTION('',(0.150042296859641,0.,-0.988679578606276));
#49049=DIRECTION('',(-0.781200482846105,0.,-0.624280230025758));
#49050=DIRECTION('',(-0.931242779705751,0.,0.364399348580519));
#49051=DIRECTION('',(-0.150042296859647,0.,0.988679578606275));
#49052=DIRECTION('',(0.781200482846104,0.,0.624280230025758));
#49053=DIRECTION('',(0.931242779705752,0.,-0.364399348580517));
#49054=DIRECTION('',(0.150042296859641,0.,-0.988679578606276));
#49055=DIRECTION('',(-0.781200482846105,0.,-0.624280230025758));
#49056=DIRECTION('',(-0.931242779705751,0.,0.364399348580519));
#49057=DIRECTION('',(-0.150042296859647,0.,0.988679578606275));
#49058=DIRECTION('',(0.781200482846104,0.,0.624280230025758));
#49059=DIRECTION('',(0.931242779705752,0.,-0.364399348580517));
#49060=DIRECTION('',(0.150042296859641,0.,-0.988679578606276));
#49061=DIRECTION('',(-0.781200482846105,0.,-0.624280230025758));
#49062=DIRECTION('',(-0.931242779705751,0.,0.364399348580519));
#49063=DIRECTION('',(-0.150042296859647,0.,0.988679578606275));
#49064=DIRECTION('',(0.781200482846104,0.,0.624280230025758));
#49065=DIRECTION('',(0.931242779705752,0.,-0.364399348580517));
#49066=DIRECTION('',(0.150042296859641,0.,-0.988679578606276));
#49067=DIRECTION('',(-0.781200482846105,0.,-0.624280230025758));
#49068=DIRECTION('',(-0.931242779705751,0.,0.364399348580519));
#49069=DIRECTION('',(-0.150042296859647,0.,0.988679578606275));
#49070=DIRECTION('',(0.781200482846104,0.,0.624280230025758));
#49071=DIRECTION('',(0.931242779705752,0.,-0.364399348580517));
#49072=DIRECTION('',(0.150042296859641,0.,-0.988679578606276));
#49073=DIRECTION('',(-0.781200482846105,0.,-0.624280230025758));
#49074=DIRECTION('',(-0.931242779705751,0.,0.364399348580519));
#49075=DIRECTION('',(-0.150042296859647,0.,0.988679578606275));
#49076=DIRECTION('',(0.781200482846104,0.,0.624280230025758));
#49077=DIRECTION('',(0.931242779705752,0.,-0.364399348580517));
#49078=DIRECTION('',(0.150042296859641,0.,-0.988679578606276));
#49079=DIRECTION('',(-0.781200482846105,0.,-0.624280230025758));
#49080=DIRECTION('',(-0.931242779705751,0.,0.364399348580519));
#49081=DIRECTION('',(-0.150042296859647,0.,0.988679578606275));
#49082=DIRECTION('',(0.781200482846104,0.,0.624280230025758));
#49083=DIRECTION('',(0.931242779705752,0.,-0.364399348580517));
#49084=DIRECTION('',(0.150042296859641,0.,-0.988679578606276));
#49085=DIRECTION('',(-0.781200482846105,0.,-0.624280230025758));
#49086=DIRECTION('',(-0.931242779705751,0.,0.364399348580519));
#49087=DIRECTION('',(-0.150042296859647,0.,0.988679578606275));
#49088=DIRECTION('',(0.781200482846104,0.,0.624280230025758));
#49089=DIRECTION('',(0.931242779705752,0.,-0.364399348580517));
#49090=DIRECTION('',(0.150042296859641,0.,-0.988679578606276));
#49091=DIRECTION('',(-0.781200482846105,0.,-0.624280230025758));
#49092=DIRECTION('',(-0.931242779705751,0.,0.364399348580519));
#49093=DIRECTION('',(-0.150042296859647,0.,0.988679578606275));
#49094=DIRECTION('',(0.781200482846104,0.,0.624280230025758));
#49095=DIRECTION('center_axis',(0.988679578606276,0.,0.150042296859641));
#49096=DIRECTION('ref_axis',(0.150042296859641,0.,-0.988679578606276));
#49097=DIRECTION('',(0.,1.,0.));
#49098=DIRECTION('',(0.,1.,0.));
#49099=DIRECTION('center_axis',(0.364399348580517,0.,0.931242779705752));
#49100=DIRECTION('ref_axis',(0.931242779705752,0.,-0.364399348580517));
#49101=DIRECTION('',(0.,1.,0.));
#49102=DIRECTION('center_axis',(-0.624280230025758,0.,0.781200482846104));
#49103=DIRECTION('ref_axis',(0.781200482846104,0.,0.624280230025758));
#49104=DIRECTION('',(0.,1.,0.));
#49105=DIRECTION('center_axis',(-0.988679578606275,0.,-0.150042296859647));
#49106=DIRECTION('ref_axis',(-0.150042296859647,0.,0.988679578606275));
#49107=DIRECTION('',(0.,1.,0.));
#49108=DIRECTION('center_axis',(-0.364399348580519,0.,-0.931242779705751));
#49109=DIRECTION('ref_axis',(-0.931242779705751,0.,0.364399348580519));
#49110=DIRECTION('',(0.,1.,0.));
#49111=DIRECTION('center_axis',(0.624280230025758,0.,-0.781200482846105));
#49112=DIRECTION('ref_axis',(-0.781200482846105,0.,-0.624280230025758));
#49113=DIRECTION('center_axis',(0.988679578606276,0.,0.150042296859641));
#49114=DIRECTION('ref_axis',(0.150042296859641,0.,-0.988679578606276));
#49115=DIRECTION('',(0.,1.,0.));
#49116=DIRECTION('',(0.,1.,0.));
#49117=DIRECTION('center_axis',(0.364399348580517,0.,0.931242779705752));
#49118=DIRECTION('ref_axis',(0.931242779705752,0.,-0.364399348580517));
#49119=DIRECTION('',(0.,1.,0.));
#49120=DIRECTION('center_axis',(-0.624280230025758,0.,0.781200482846104));
#49121=DIRECTION('ref_axis',(0.781200482846104,0.,0.624280230025758));
#49122=DIRECTION('',(0.,1.,0.));
#49123=DIRECTION('center_axis',(-0.988679578606275,0.,-0.150042296859647));
#49124=DIRECTION('ref_axis',(-0.150042296859647,0.,0.988679578606275));
#49125=DIRECTION('',(0.,1.,0.));
#49126=DIRECTION('center_axis',(-0.364399348580519,0.,-0.931242779705751));
#49127=DIRECTION('ref_axis',(-0.931242779705751,0.,0.364399348580519));
#49128=DIRECTION('',(0.,1.,0.));
#49129=DIRECTION('center_axis',(0.624280230025758,0.,-0.781200482846105));
#49130=DIRECTION('ref_axis',(-0.781200482846105,0.,-0.624280230025758));
#49131=DIRECTION('center_axis',(0.988679578606276,0.,0.150042296859641));
#49132=DIRECTION('ref_axis',(0.150042296859641,0.,-0.988679578606276));
#49133=DIRECTION('',(0.,1.,0.));
#49134=DIRECTION('',(0.,1.,0.));
#49135=DIRECTION('center_axis',(0.364399348580517,0.,0.931242779705752));
#49136=DIRECTION('ref_axis',(0.931242779705752,0.,-0.364399348580517));
#49137=DIRECTION('',(0.,1.,0.));
#49138=DIRECTION('center_axis',(-0.624280230025758,0.,0.781200482846104));
#49139=DIRECTION('ref_axis',(0.781200482846104,0.,0.624280230025758));
#49140=DIRECTION('',(0.,1.,0.));
#49141=DIRECTION('center_axis',(-0.988679578606275,0.,-0.150042296859647));
#49142=DIRECTION('ref_axis',(-0.150042296859647,0.,0.988679578606275));
#49143=DIRECTION('',(0.,1.,0.));
#49144=DIRECTION('center_axis',(-0.364399348580519,0.,-0.931242779705751));
#49145=DIRECTION('ref_axis',(-0.931242779705751,0.,0.364399348580519));
#49146=DIRECTION('',(0.,1.,0.));
#49147=DIRECTION('center_axis',(0.624280230025758,0.,-0.781200482846105));
#49148=DIRECTION('ref_axis',(-0.781200482846105,0.,-0.624280230025758));
#49149=DIRECTION('center_axis',(0.988679578606276,0.,0.150042296859641));
#49150=DIRECTION('ref_axis',(0.150042296859641,0.,-0.988679578606276));
#49151=DIRECTION('',(0.,1.,0.));
#49152=DIRECTION('',(0.,1.,0.));
#49153=DIRECTION('center_axis',(0.364399348580517,0.,0.931242779705752));
#49154=DIRECTION('ref_axis',(0.931242779705752,0.,-0.364399348580517));
#49155=DIRECTION('',(0.,1.,0.));
#49156=DIRECTION('center_axis',(-0.624280230025758,0.,0.781200482846104));
#49157=DIRECTION('ref_axis',(0.781200482846104,0.,0.624280230025758));
#49158=DIRECTION('',(0.,1.,0.));
#49159=DIRECTION('center_axis',(-0.988679578606275,0.,-0.150042296859647));
#49160=DIRECTION('ref_axis',(-0.150042296859647,0.,0.988679578606275));
#49161=DIRECTION('',(0.,1.,0.));
#49162=DIRECTION('center_axis',(-0.364399348580519,0.,-0.931242779705751));
#49163=DIRECTION('ref_axis',(-0.931242779705751,0.,0.364399348580519));
#49164=DIRECTION('',(0.,1.,0.));
#49165=DIRECTION('center_axis',(0.624280230025758,0.,-0.781200482846105));
#49166=DIRECTION('ref_axis',(-0.781200482846105,0.,-0.624280230025758));
#49167=DIRECTION('center_axis',(0.988679578606276,0.,0.150042296859641));
#49168=DIRECTION('ref_axis',(0.150042296859641,0.,-0.988679578606276));
#49169=DIRECTION('',(0.,1.,0.));
#49170=DIRECTION('',(0.,1.,0.));
#49171=DIRECTION('center_axis',(0.364399348580517,0.,0.931242779705752));
#49172=DIRECTION('ref_axis',(0.931242779705752,0.,-0.364399348580517));
#49173=DIRECTION('',(0.,1.,0.));
#49174=DIRECTION('center_axis',(-0.624280230025758,0.,0.781200482846104));
#49175=DIRECTION('ref_axis',(0.781200482846104,0.,0.624280230025758));
#49176=DIRECTION('',(0.,1.,0.));
#49177=DIRECTION('center_axis',(-0.988679578606275,0.,-0.150042296859647));
#49178=DIRECTION('ref_axis',(-0.150042296859647,0.,0.988679578606275));
#49179=DIRECTION('',(0.,1.,0.));
#49180=DIRECTION('center_axis',(-0.364399348580519,0.,-0.931242779705751));
#49181=DIRECTION('ref_axis',(-0.931242779705751,0.,0.364399348580519));
#49182=DIRECTION('',(0.,1.,0.));
#49183=DIRECTION('center_axis',(0.624280230025758,0.,-0.781200482846105));
#49184=DIRECTION('ref_axis',(-0.781200482846105,0.,-0.624280230025758));
#49185=DIRECTION('center_axis',(0.988679578606276,0.,0.150042296859641));
#49186=DIRECTION('ref_axis',(0.150042296859641,0.,-0.988679578606276));
#49187=DIRECTION('',(0.,1.,0.));
#49188=DIRECTION('',(0.,1.,0.));
#49189=DIRECTION('center_axis',(0.364399348580517,0.,0.931242779705752));
#49190=DIRECTION('ref_axis',(0.931242779705752,0.,-0.364399348580517));
#49191=DIRECTION('',(0.,1.,0.));
#49192=DIRECTION('center_axis',(-0.624280230025758,0.,0.781200482846104));
#49193=DIRECTION('ref_axis',(0.781200482846104,0.,0.624280230025758));
#49194=DIRECTION('',(0.,1.,0.));
#49195=DIRECTION('center_axis',(-0.988679578606275,0.,-0.150042296859647));
#49196=DIRECTION('ref_axis',(-0.150042296859647,0.,0.988679578606275));
#49197=DIRECTION('',(0.,1.,0.));
#49198=DIRECTION('center_axis',(-0.364399348580519,0.,-0.931242779705751));
#49199=DIRECTION('ref_axis',(-0.931242779705751,0.,0.364399348580519));
#49200=DIRECTION('',(0.,1.,0.));
#49201=DIRECTION('center_axis',(0.624280230025758,0.,-0.781200482846105));
#49202=DIRECTION('ref_axis',(-0.781200482846105,0.,-0.624280230025758));
#49203=DIRECTION('center_axis',(0.988679578606276,0.,0.150042296859641));
#49204=DIRECTION('ref_axis',(0.150042296859641,0.,-0.988679578606276));
#49205=DIRECTION('',(0.,1.,0.));
#49206=DIRECTION('',(0.,1.,0.));
#49207=DIRECTION('center_axis',(0.364399348580517,0.,0.931242779705752));
#49208=DIRECTION('ref_axis',(0.931242779705752,0.,-0.364399348580517));
#49209=DIRECTION('',(0.,1.,0.));
#49210=DIRECTION('center_axis',(-0.624280230025758,0.,0.781200482846104));
#49211=DIRECTION('ref_axis',(0.781200482846104,0.,0.624280230025758));
#49212=DIRECTION('',(0.,1.,0.));
#49213=DIRECTION('center_axis',(-0.988679578606275,0.,-0.150042296859647));
#49214=DIRECTION('ref_axis',(-0.150042296859647,0.,0.988679578606275));
#49215=DIRECTION('',(0.,1.,0.));
#49216=DIRECTION('center_axis',(-0.364399348580519,0.,-0.931242779705751));
#49217=DIRECTION('ref_axis',(-0.931242779705751,0.,0.364399348580519));
#49218=DIRECTION('',(0.,1.,0.));
#49219=DIRECTION('center_axis',(0.624280230025758,0.,-0.781200482846105));
#49220=DIRECTION('ref_axis',(-0.781200482846105,0.,-0.624280230025758));
#49221=DIRECTION('center_axis',(0.988679578606276,0.,0.150042296859641));
#49222=DIRECTION('ref_axis',(0.150042296859641,0.,-0.988679578606276));
#49223=DIRECTION('',(0.,1.,0.));
#49224=DIRECTION('',(0.,1.,0.));
#49225=DIRECTION('center_axis',(0.364399348580517,0.,0.931242779705752));
#49226=DIRECTION('ref_axis',(0.931242779705752,0.,-0.364399348580517));
#49227=DIRECTION('',(0.,1.,0.));
#49228=DIRECTION('center_axis',(-0.624280230025758,0.,0.781200482846104));
#49229=DIRECTION('ref_axis',(0.781200482846104,0.,0.624280230025758));
#49230=DIRECTION('',(0.,1.,0.));
#49231=DIRECTION('center_axis',(-0.988679578606275,0.,-0.150042296859647));
#49232=DIRECTION('ref_axis',(-0.150042296859647,0.,0.988679578606275));
#49233=DIRECTION('',(0.,1.,0.));
#49234=DIRECTION('center_axis',(-0.364399348580519,0.,-0.931242779705751));
#49235=DIRECTION('ref_axis',(-0.931242779705751,0.,0.364399348580519));
#49236=DIRECTION('',(0.,1.,0.));
#49237=DIRECTION('center_axis',(0.624280230025758,0.,-0.781200482846105));
#49238=DIRECTION('ref_axis',(-0.781200482846105,0.,-0.624280230025758));
#49239=DIRECTION('center_axis',(0.988679578606276,0.,0.150042296859641));
#49240=DIRECTION('ref_axis',(0.150042296859641,0.,-0.988679578606276));
#49241=DIRECTION('',(0.,1.,0.));
#49242=DIRECTION('',(0.,1.,0.));
#49243=DIRECTION('center_axis',(0.364399348580517,0.,0.931242779705752));
#49244=DIRECTION('ref_axis',(0.931242779705752,0.,-0.364399348580517));
#49245=DIRECTION('',(0.,1.,0.));
#49246=DIRECTION('center_axis',(-0.624280230025758,0.,0.781200482846104));
#49247=DIRECTION('ref_axis',(0.781200482846104,0.,0.624280230025758));
#49248=DIRECTION('',(0.,1.,0.));
#49249=DIRECTION('center_axis',(-0.988679578606275,0.,-0.150042296859647));
#49250=DIRECTION('ref_axis',(-0.150042296859647,0.,0.988679578606275));
#49251=DIRECTION('',(0.,1.,0.));
#49252=DIRECTION('center_axis',(-0.364399348580519,0.,-0.931242779705751));
#49253=DIRECTION('ref_axis',(-0.931242779705751,0.,0.364399348580519));
#49254=DIRECTION('',(0.,1.,0.));
#49255=DIRECTION('center_axis',(0.624280230025758,0.,-0.781200482846105));
#49256=DIRECTION('ref_axis',(-0.781200482846105,0.,-0.624280230025758));
#49257=DIRECTION('center_axis',(0.988679578606276,0.,0.150042296859641));
#49258=DIRECTION('ref_axis',(0.150042296859641,0.,-0.988679578606276));
#49259=DIRECTION('',(0.,1.,0.));
#49260=DIRECTION('',(0.,1.,0.));
#49261=DIRECTION('center_axis',(0.364399348580517,0.,0.931242779705752));
#49262=DIRECTION('ref_axis',(0.931242779705752,0.,-0.364399348580517));
#49263=DIRECTION('',(0.,1.,0.));
#49264=DIRECTION('center_axis',(-0.624280230025758,0.,0.781200482846104));
#49265=DIRECTION('ref_axis',(0.781200482846104,0.,0.624280230025758));
#49266=DIRECTION('',(0.,1.,0.));
#49267=DIRECTION('center_axis',(-0.988679578606275,0.,-0.150042296859647));
#49268=DIRECTION('ref_axis',(-0.150042296859647,0.,0.988679578606275));
#49269=DIRECTION('',(0.,1.,0.));
#49270=DIRECTION('center_axis',(-0.364399348580519,0.,-0.931242779705751));
#49271=DIRECTION('ref_axis',(-0.931242779705751,0.,0.364399348580519));
#49272=DIRECTION('',(0.,1.,0.));
#49273=DIRECTION('center_axis',(0.624280230025758,0.,-0.781200482846105));
#49274=DIRECTION('ref_axis',(-0.781200482846105,0.,-0.624280230025758));
#49275=DIRECTION('center_axis',(0.988679578606276,0.,0.150042296859641));
#49276=DIRECTION('ref_axis',(0.150042296859641,0.,-0.988679578606276));
#49277=DIRECTION('',(0.,1.,0.));
#49278=DIRECTION('',(0.,1.,0.));
#49279=DIRECTION('center_axis',(0.364399348580517,0.,0.931242779705752));
#49280=DIRECTION('ref_axis',(0.931242779705752,0.,-0.364399348580517));
#49281=DIRECTION('',(0.,1.,0.));
#49282=DIRECTION('center_axis',(-0.624280230025758,0.,0.781200482846104));
#49283=DIRECTION('ref_axis',(0.781200482846104,0.,0.624280230025758));
#49284=DIRECTION('',(0.,1.,0.));
#49285=DIRECTION('center_axis',(-0.988679578606275,0.,-0.150042296859647));
#49286=DIRECTION('ref_axis',(-0.150042296859647,0.,0.988679578606275));
#49287=DIRECTION('',(0.,1.,0.));
#49288=DIRECTION('center_axis',(-0.364399348580519,0.,-0.931242779705751));
#49289=DIRECTION('ref_axis',(-0.931242779705751,0.,0.364399348580519));
#49290=DIRECTION('',(0.,1.,0.));
#49291=DIRECTION('center_axis',(0.624280230025758,0.,-0.781200482846105));
#49292=DIRECTION('ref_axis',(-0.781200482846105,0.,-0.624280230025758));
#49293=DIRECTION('center_axis',(0.988679578606276,0.,0.150042296859641));
#49294=DIRECTION('ref_axis',(0.150042296859641,0.,-0.988679578606276));
#49295=DIRECTION('',(0.,1.,0.));
#49296=DIRECTION('',(0.,1.,0.));
#49297=DIRECTION('center_axis',(0.364399348580517,0.,0.931242779705752));
#49298=DIRECTION('ref_axis',(0.931242779705752,0.,-0.364399348580517));
#49299=DIRECTION('',(0.,1.,0.));
#49300=DIRECTION('center_axis',(-0.624280230025758,0.,0.781200482846104));
#49301=DIRECTION('ref_axis',(0.781200482846104,0.,0.624280230025758));
#49302=DIRECTION('',(0.,1.,0.));
#49303=DIRECTION('center_axis',(-0.988679578606275,0.,-0.150042296859647));
#49304=DIRECTION('ref_axis',(-0.150042296859647,0.,0.988679578606275));
#49305=DIRECTION('',(0.,1.,0.));
#49306=DIRECTION('center_axis',(-0.364399348580519,0.,-0.931242779705751));
#49307=DIRECTION('ref_axis',(-0.931242779705751,0.,0.364399348580519));
#49308=DIRECTION('',(0.,1.,0.));
#49309=DIRECTION('center_axis',(0.624280230025758,0.,-0.781200482846105));
#49310=DIRECTION('ref_axis',(-0.781200482846105,0.,-0.624280230025758));
#49311=DIRECTION('center_axis',(0.988679578606276,0.,0.150042296859641));
#49312=DIRECTION('ref_axis',(0.150042296859641,0.,-0.988679578606276));
#49313=DIRECTION('',(0.,1.,0.));
#49314=DIRECTION('',(0.,1.,0.));
#49315=DIRECTION('center_axis',(0.364399348580517,0.,0.931242779705752));
#49316=DIRECTION('ref_axis',(0.931242779705752,0.,-0.364399348580517));
#49317=DIRECTION('',(0.,1.,0.));
#49318=DIRECTION('center_axis',(-0.624280230025758,0.,0.781200482846104));
#49319=DIRECTION('ref_axis',(0.781200482846104,0.,0.624280230025758));
#49320=DIRECTION('',(0.,1.,0.));
#49321=DIRECTION('center_axis',(-0.988679578606275,0.,-0.150042296859647));
#49322=DIRECTION('ref_axis',(-0.150042296859647,0.,0.988679578606275));
#49323=DIRECTION('',(0.,1.,0.));
#49324=DIRECTION('center_axis',(-0.364399348580519,0.,-0.931242779705751));
#49325=DIRECTION('ref_axis',(-0.931242779705751,0.,0.364399348580519));
#49326=DIRECTION('',(0.,1.,0.));
#49327=DIRECTION('center_axis',(0.624280230025758,0.,-0.781200482846105));
#49328=DIRECTION('ref_axis',(-0.781200482846105,0.,-0.624280230025758));
#49329=DIRECTION('center_axis',(0.988679578606276,0.,0.150042296859641));
#49330=DIRECTION('ref_axis',(0.150042296859641,0.,-0.988679578606276));
#49331=DIRECTION('',(0.,1.,0.));
#49332=DIRECTION('',(0.,1.,0.));
#49333=DIRECTION('center_axis',(0.364399348580517,0.,0.931242779705752));
#49334=DIRECTION('ref_axis',(0.931242779705752,0.,-0.364399348580517));
#49335=DIRECTION('',(0.,1.,0.));
#49336=DIRECTION('center_axis',(-0.624280230025758,0.,0.781200482846104));
#49337=DIRECTION('ref_axis',(0.781200482846104,0.,0.624280230025758));
#49338=DIRECTION('',(0.,1.,0.));
#49339=DIRECTION('center_axis',(-0.988679578606275,0.,-0.150042296859647));
#49340=DIRECTION('ref_axis',(-0.150042296859647,0.,0.988679578606275));
#49341=DIRECTION('',(0.,1.,0.));
#49342=DIRECTION('center_axis',(-0.364399348580519,0.,-0.931242779705751));
#49343=DIRECTION('ref_axis',(-0.931242779705751,0.,0.364399348580519));
#49344=DIRECTION('',(0.,1.,0.));
#49345=DIRECTION('center_axis',(0.624280230025758,0.,-0.781200482846105));
#49346=DIRECTION('ref_axis',(-0.781200482846105,0.,-0.624280230025758));
#49347=DIRECTION('center_axis',(0.988679578606276,0.,0.150042296859641));
#49348=DIRECTION('ref_axis',(0.150042296859641,0.,-0.988679578606276));
#49349=DIRECTION('',(0.,1.,0.));
#49350=DIRECTION('',(0.,1.,0.));
#49351=DIRECTION('center_axis',(0.364399348580517,0.,0.931242779705752));
#49352=DIRECTION('ref_axis',(0.931242779705752,0.,-0.364399348580517));
#49353=DIRECTION('',(0.,1.,0.));
#49354=DIRECTION('center_axis',(-0.624280230025758,0.,0.781200482846104));
#49355=DIRECTION('ref_axis',(0.781200482846104,0.,0.624280230025758));
#49356=DIRECTION('',(0.,1.,0.));
#49357=DIRECTION('center_axis',(-0.988679578606275,0.,-0.150042296859647));
#49358=DIRECTION('ref_axis',(-0.150042296859647,0.,0.988679578606275));
#49359=DIRECTION('',(0.,1.,0.));
#49360=DIRECTION('center_axis',(-0.364399348580519,0.,-0.931242779705751));
#49361=DIRECTION('ref_axis',(-0.931242779705751,0.,0.364399348580519));
#49362=DIRECTION('',(0.,1.,0.));
#49363=DIRECTION('center_axis',(0.624280230025758,0.,-0.781200482846105));
#49364=DIRECTION('ref_axis',(-0.781200482846105,0.,-0.624280230025758));
#49365=DIRECTION('center_axis',(0.988679578606276,0.,0.150042296859641));
#49366=DIRECTION('ref_axis',(0.150042296859641,0.,-0.988679578606276));
#49367=DIRECTION('',(0.,1.,0.));
#49368=DIRECTION('',(0.,1.,0.));
#49369=DIRECTION('center_axis',(0.364399348580517,0.,0.931242779705752));
#49370=DIRECTION('ref_axis',(0.931242779705752,0.,-0.364399348580517));
#49371=DIRECTION('',(0.,1.,0.));
#49372=DIRECTION('center_axis',(-0.624280230025758,0.,0.781200482846104));
#49373=DIRECTION('ref_axis',(0.781200482846104,0.,0.624280230025758));
#49374=DIRECTION('',(0.,1.,0.));
#49375=DIRECTION('center_axis',(-0.988679578606275,0.,-0.150042296859647));
#49376=DIRECTION('ref_axis',(-0.150042296859647,0.,0.988679578606275));
#49377=DIRECTION('',(0.,1.,0.));
#49378=DIRECTION('center_axis',(-0.364399348580519,0.,-0.931242779705751));
#49379=DIRECTION('ref_axis',(-0.931242779705751,0.,0.364399348580519));
#49380=DIRECTION('',(0.,1.,0.));
#49381=DIRECTION('center_axis',(0.624280230025758,0.,-0.781200482846105));
#49382=DIRECTION('ref_axis',(-0.781200482846105,0.,-0.624280230025758));
#49383=DIRECTION('center_axis',(0.988679578606276,0.,0.150042296859641));
#49384=DIRECTION('ref_axis',(0.150042296859641,0.,-0.988679578606276));
#49385=DIRECTION('',(0.,1.,0.));
#49386=DIRECTION('',(0.,1.,0.));
#49387=DIRECTION('center_axis',(0.364399348580517,0.,0.931242779705752));
#49388=DIRECTION('ref_axis',(0.931242779705752,0.,-0.364399348580517));
#49389=DIRECTION('',(0.,1.,0.));
#49390=DIRECTION('center_axis',(-0.624280230025758,0.,0.781200482846104));
#49391=DIRECTION('ref_axis',(0.781200482846104,0.,0.624280230025758));
#49392=DIRECTION('',(0.,1.,0.));
#49393=DIRECTION('center_axis',(-0.988679578606275,0.,-0.150042296859647));
#49394=DIRECTION('ref_axis',(-0.150042296859647,0.,0.988679578606275));
#49395=DIRECTION('',(0.,1.,0.));
#49396=DIRECTION('center_axis',(-0.364399348580519,0.,-0.931242779705751));
#49397=DIRECTION('ref_axis',(-0.931242779705751,0.,0.364399348580519));
#49398=DIRECTION('',(0.,1.,0.));
#49399=DIRECTION('center_axis',(0.624280230025758,0.,-0.781200482846105));
#49400=DIRECTION('ref_axis',(-0.781200482846105,0.,-0.624280230025758));
#49401=DIRECTION('center_axis',(0.988679578606276,0.,0.150042296859641));
#49402=DIRECTION('ref_axis',(0.150042296859641,0.,-0.988679578606276));
#49403=DIRECTION('',(0.,1.,0.));
#49404=DIRECTION('',(0.,1.,0.));
#49405=DIRECTION('center_axis',(0.364399348580517,0.,0.931242779705752));
#49406=DIRECTION('ref_axis',(0.931242779705752,0.,-0.364399348580517));
#49407=DIRECTION('',(0.,1.,0.));
#49408=DIRECTION('center_axis',(-0.624280230025758,0.,0.781200482846104));
#49409=DIRECTION('ref_axis',(0.781200482846104,0.,0.624280230025758));
#49410=DIRECTION('',(0.,1.,0.));
#49411=DIRECTION('center_axis',(-0.988679578606275,0.,-0.150042296859647));
#49412=DIRECTION('ref_axis',(-0.150042296859647,0.,0.988679578606275));
#49413=DIRECTION('',(0.,1.,0.));
#49414=DIRECTION('center_axis',(-0.364399348580519,0.,-0.931242779705751));
#49415=DIRECTION('ref_axis',(-0.931242779705751,0.,0.364399348580519));
#49416=DIRECTION('',(0.,1.,0.));
#49417=DIRECTION('center_axis',(0.624280230025758,0.,-0.781200482846105));
#49418=DIRECTION('ref_axis',(-0.781200482846105,0.,-0.624280230025758));
#49419=DIRECTION('center_axis',(0.988679578606276,0.,0.150042296859641));
#49420=DIRECTION('ref_axis',(0.150042296859641,0.,-0.988679578606276));
#49421=DIRECTION('',(0.,1.,0.));
#49422=DIRECTION('',(0.,1.,0.));
#49423=DIRECTION('center_axis',(0.364399348580517,0.,0.931242779705752));
#49424=DIRECTION('ref_axis',(0.931242779705752,0.,-0.364399348580517));
#49425=DIRECTION('',(0.,1.,0.));
#49426=DIRECTION('center_axis',(-0.624280230025758,0.,0.781200482846104));
#49427=DIRECTION('ref_axis',(0.781200482846104,0.,0.624280230025758));
#49428=DIRECTION('',(0.,1.,0.));
#49429=DIRECTION('center_axis',(-0.988679578606275,0.,-0.150042296859647));
#49430=DIRECTION('ref_axis',(-0.150042296859647,0.,0.988679578606275));
#49431=DIRECTION('',(0.,1.,0.));
#49432=DIRECTION('center_axis',(-0.364399348580519,0.,-0.931242779705751));
#49433=DIRECTION('ref_axis',(-0.931242779705751,0.,0.364399348580519));
#49434=DIRECTION('',(0.,1.,0.));
#49435=DIRECTION('center_axis',(0.624280230025758,0.,-0.781200482846105));
#49436=DIRECTION('ref_axis',(-0.781200482846105,0.,-0.624280230025758));
#49437=DIRECTION('center_axis',(0.988679578606276,0.,0.150042296859641));
#49438=DIRECTION('ref_axis',(0.150042296859641,0.,-0.988679578606276));
#49439=DIRECTION('',(0.,1.,0.));
#49440=DIRECTION('',(0.,1.,0.));
#49441=DIRECTION('center_axis',(0.364399348580517,0.,0.931242779705752));
#49442=DIRECTION('ref_axis',(0.931242779705752,0.,-0.364399348580517));
#49443=DIRECTION('',(0.,1.,0.));
#49444=DIRECTION('center_axis',(-0.624280230025758,0.,0.781200482846104));
#49445=DIRECTION('ref_axis',(0.781200482846104,0.,0.624280230025758));
#49446=DIRECTION('',(0.,1.,0.));
#49447=DIRECTION('center_axis',(-0.988679578606275,0.,-0.150042296859647));
#49448=DIRECTION('ref_axis',(-0.150042296859647,0.,0.988679578606275));
#49449=DIRECTION('',(0.,1.,0.));
#49450=DIRECTION('center_axis',(-0.364399348580519,0.,-0.931242779705751));
#49451=DIRECTION('ref_axis',(-0.931242779705751,0.,0.364399348580519));
#49452=DIRECTION('',(0.,1.,0.));
#49453=DIRECTION('center_axis',(0.624280230025758,0.,-0.781200482846105));
#49454=DIRECTION('ref_axis',(-0.781200482846105,0.,-0.624280230025758));
#49455=DIRECTION('center_axis',(0.988679578606276,0.,0.150042296859641));
#49456=DIRECTION('ref_axis',(0.150042296859641,0.,-0.988679578606276));
#49457=DIRECTION('',(0.,1.,0.));
#49458=DIRECTION('',(0.,1.,0.));
#49459=DIRECTION('center_axis',(0.364399348580517,0.,0.931242779705752));
#49460=DIRECTION('ref_axis',(0.931242779705752,0.,-0.364399348580517));
#49461=DIRECTION('',(0.,1.,0.));
#49462=DIRECTION('center_axis',(-0.624280230025758,0.,0.781200482846104));
#49463=DIRECTION('ref_axis',(0.781200482846104,0.,0.624280230025758));
#49464=DIRECTION('',(0.,1.,0.));
#49465=DIRECTION('center_axis',(-0.988679578606275,0.,-0.150042296859647));
#49466=DIRECTION('ref_axis',(-0.150042296859647,0.,0.988679578606275));
#49467=DIRECTION('',(0.,1.,0.));
#49468=DIRECTION('center_axis',(-0.364399348580519,0.,-0.931242779705751));
#49469=DIRECTION('ref_axis',(-0.931242779705751,0.,0.364399348580519));
#49470=DIRECTION('',(0.,1.,0.));
#49471=DIRECTION('center_axis',(0.624280230025758,0.,-0.781200482846105));
#49472=DIRECTION('ref_axis',(-0.781200482846105,0.,-0.624280230025758));
#49473=DIRECTION('center_axis',(0.988679578606276,0.,0.150042296859641));
#49474=DIRECTION('ref_axis',(0.150042296859641,0.,-0.988679578606276));
#49475=DIRECTION('',(0.,1.,0.));
#49476=DIRECTION('',(0.,1.,0.));
#49477=DIRECTION('center_axis',(0.364399348580517,0.,0.931242779705752));
#49478=DIRECTION('ref_axis',(0.931242779705752,0.,-0.364399348580517));
#49479=DIRECTION('',(0.,1.,0.));
#49480=DIRECTION('center_axis',(-0.624280230025758,0.,0.781200482846104));
#49481=DIRECTION('ref_axis',(0.781200482846104,0.,0.624280230025758));
#49482=DIRECTION('',(0.,1.,0.));
#49483=DIRECTION('center_axis',(-0.988679578606275,0.,-0.150042296859647));
#49484=DIRECTION('ref_axis',(-0.150042296859647,0.,0.988679578606275));
#49485=DIRECTION('',(0.,1.,0.));
#49486=DIRECTION('center_axis',(-0.364399348580519,0.,-0.931242779705751));
#49487=DIRECTION('ref_axis',(-0.931242779705751,0.,0.364399348580519));
#49488=DIRECTION('',(0.,1.,0.));
#49489=DIRECTION('center_axis',(0.624280230025758,0.,-0.781200482846105));
#49490=DIRECTION('ref_axis',(-0.781200482846105,0.,-0.624280230025758));
#49491=DIRECTION('center_axis',(0.988679578606276,0.,0.150042296859641));
#49492=DIRECTION('ref_axis',(0.150042296859641,0.,-0.988679578606276));
#49493=DIRECTION('',(0.,1.,0.));
#49494=DIRECTION('',(0.,1.,0.));
#49495=DIRECTION('center_axis',(0.364399348580517,0.,0.931242779705752));
#49496=DIRECTION('ref_axis',(0.931242779705752,0.,-0.364399348580517));
#49497=DIRECTION('',(0.,1.,0.));
#49498=DIRECTION('center_axis',(-0.624280230025758,0.,0.781200482846104));
#49499=DIRECTION('ref_axis',(0.781200482846104,0.,0.624280230025758));
#49500=DIRECTION('',(0.,1.,0.));
#49501=DIRECTION('center_axis',(-0.988679578606275,0.,-0.150042296859647));
#49502=DIRECTION('ref_axis',(-0.150042296859647,0.,0.988679578606275));
#49503=DIRECTION('',(0.,1.,0.));
#49504=DIRECTION('center_axis',(-0.364399348580519,0.,-0.931242779705751));
#49505=DIRECTION('ref_axis',(-0.931242779705751,0.,0.364399348580519));
#49506=DIRECTION('',(0.,1.,0.));
#49507=DIRECTION('center_axis',(0.624280230025758,0.,-0.781200482846105));
#49508=DIRECTION('ref_axis',(-0.781200482846105,0.,-0.624280230025758));
#49509=DIRECTION('center_axis',(0.988679578606276,0.,0.150042296859641));
#49510=DIRECTION('ref_axis',(0.150042296859641,0.,-0.988679578606276));
#49511=DIRECTION('',(0.,1.,0.));
#49512=DIRECTION('',(0.,1.,0.));
#49513=DIRECTION('center_axis',(0.364399348580517,0.,0.931242779705752));
#49514=DIRECTION('ref_axis',(0.931242779705752,0.,-0.364399348580517));
#49515=DIRECTION('',(0.,1.,0.));
#49516=DIRECTION('center_axis',(-0.624280230025758,0.,0.781200482846104));
#49517=DIRECTION('ref_axis',(0.781200482846104,0.,0.624280230025758));
#49518=DIRECTION('',(0.,1.,0.));
#49519=DIRECTION('center_axis',(-0.988679578606275,0.,-0.150042296859647));
#49520=DIRECTION('ref_axis',(-0.150042296859647,0.,0.988679578606275));
#49521=DIRECTION('',(0.,1.,0.));
#49522=DIRECTION('center_axis',(-0.364399348580519,0.,-0.931242779705751));
#49523=DIRECTION('ref_axis',(-0.931242779705751,0.,0.364399348580519));
#49524=DIRECTION('',(0.,1.,0.));
#49525=DIRECTION('center_axis',(0.624280230025758,0.,-0.781200482846105));
#49526=DIRECTION('ref_axis',(-0.781200482846105,0.,-0.624280230025758));
#49527=DIRECTION('center_axis',(0.988679578606276,0.,0.150042296859641));
#49528=DIRECTION('ref_axis',(0.150042296859641,0.,-0.988679578606276));
#49529=DIRECTION('',(0.,1.,0.));
#49530=DIRECTION('',(0.,1.,0.));
#49531=DIRECTION('center_axis',(0.364399348580517,0.,0.931242779705752));
#49532=DIRECTION('ref_axis',(0.931242779705752,0.,-0.364399348580517));
#49533=DIRECTION('',(0.,1.,0.));
#49534=DIRECTION('center_axis',(-0.624280230025758,0.,0.781200482846104));
#49535=DIRECTION('ref_axis',(0.781200482846104,0.,0.624280230025758));
#49536=DIRECTION('',(0.,1.,0.));
#49537=DIRECTION('center_axis',(-0.988679578606275,0.,-0.150042296859647));
#49538=DIRECTION('ref_axis',(-0.150042296859647,0.,0.988679578606275));
#49539=DIRECTION('',(0.,1.,0.));
#49540=DIRECTION('center_axis',(-0.364399348580519,0.,-0.931242779705751));
#49541=DIRECTION('ref_axis',(-0.931242779705751,0.,0.364399348580519));
#49542=DIRECTION('',(0.,1.,0.));
#49543=DIRECTION('center_axis',(0.624280230025758,0.,-0.781200482846105));
#49544=DIRECTION('ref_axis',(-0.781200482846105,0.,-0.624280230025758));
#49545=DIRECTION('center_axis',(0.988679578606276,0.,0.150042296859641));
#49546=DIRECTION('ref_axis',(0.150042296859641,0.,-0.988679578606276));
#49547=DIRECTION('',(0.,1.,0.));
#49548=DIRECTION('',(0.,1.,0.));
#49549=DIRECTION('center_axis',(0.364399348580517,0.,0.931242779705752));
#49550=DIRECTION('ref_axis',(0.931242779705752,0.,-0.364399348580517));
#49551=DIRECTION('',(0.,1.,0.));
#49552=DIRECTION('center_axis',(-0.624280230025758,0.,0.781200482846104));
#49553=DIRECTION('ref_axis',(0.781200482846104,0.,0.624280230025758));
#49554=DIRECTION('',(0.,1.,0.));
#49555=DIRECTION('center_axis',(-0.988679578606275,0.,-0.150042296859647));
#49556=DIRECTION('ref_axis',(-0.150042296859647,0.,0.988679578606275));
#49557=DIRECTION('',(0.,1.,0.));
#49558=DIRECTION('center_axis',(-0.364399348580519,0.,-0.931242779705751));
#49559=DIRECTION('ref_axis',(-0.931242779705751,0.,0.364399348580519));
#49560=DIRECTION('',(0.,1.,0.));
#49561=DIRECTION('center_axis',(0.624280230025758,0.,-0.781200482846105));
#49562=DIRECTION('ref_axis',(-0.781200482846105,0.,-0.624280230025758));
#49563=DIRECTION('center_axis',(0.988679578606276,0.,0.150042296859641));
#49564=DIRECTION('ref_axis',(0.150042296859641,0.,-0.988679578606276));
#49565=DIRECTION('',(0.,1.,0.));
#49566=DIRECTION('',(0.,1.,0.));
#49567=DIRECTION('center_axis',(0.364399348580517,0.,0.931242779705752));
#49568=DIRECTION('ref_axis',(0.931242779705752,0.,-0.364399348580517));
#49569=DIRECTION('',(0.,1.,0.));
#49570=DIRECTION('center_axis',(-0.624280230025758,0.,0.781200482846104));
#49571=DIRECTION('ref_axis',(0.781200482846104,0.,0.624280230025758));
#49572=DIRECTION('',(0.,1.,0.));
#49573=DIRECTION('center_axis',(-0.988679578606275,0.,-0.150042296859647));
#49574=DIRECTION('ref_axis',(-0.150042296859647,0.,0.988679578606275));
#49575=DIRECTION('',(0.,1.,0.));
#49576=DIRECTION('center_axis',(-0.364399348580519,0.,-0.931242779705751));
#49577=DIRECTION('ref_axis',(-0.931242779705751,0.,0.364399348580519));
#49578=DIRECTION('',(0.,1.,0.));
#49579=DIRECTION('center_axis',(0.624280230025758,0.,-0.781200482846105));
#49580=DIRECTION('ref_axis',(-0.781200482846105,0.,-0.624280230025758));
#49581=DIRECTION('center_axis',(0.988679578606276,0.,0.150042296859641));
#49582=DIRECTION('ref_axis',(0.150042296859641,0.,-0.988679578606276));
#49583=DIRECTION('',(0.,1.,0.));
#49584=DIRECTION('',(0.,1.,0.));
#49585=DIRECTION('center_axis',(0.364399348580517,0.,0.931242779705752));
#49586=DIRECTION('ref_axis',(0.931242779705752,0.,-0.364399348580517));
#49587=DIRECTION('',(0.,1.,0.));
#49588=DIRECTION('center_axis',(-0.624280230025758,0.,0.781200482846104));
#49589=DIRECTION('ref_axis',(0.781200482846104,0.,0.624280230025758));
#49590=DIRECTION('',(0.,1.,0.));
#49591=DIRECTION('center_axis',(-0.988679578606275,0.,-0.150042296859647));
#49592=DIRECTION('ref_axis',(-0.150042296859647,0.,0.988679578606275));
#49593=DIRECTION('',(0.,1.,0.));
#49594=DIRECTION('center_axis',(-0.364399348580519,0.,-0.931242779705751));
#49595=DIRECTION('ref_axis',(-0.931242779705751,0.,0.364399348580519));
#49596=DIRECTION('',(0.,1.,0.));
#49597=DIRECTION('center_axis',(0.624280230025758,0.,-0.781200482846105));
#49598=DIRECTION('ref_axis',(-0.781200482846105,0.,-0.624280230025758));
#49599=DIRECTION('center_axis',(0.988679578606276,0.,0.150042296859641));
#49600=DIRECTION('ref_axis',(0.150042296859641,0.,-0.988679578606276));
#49601=DIRECTION('',(0.,1.,0.));
#49602=DIRECTION('',(0.,1.,0.));
#49603=DIRECTION('center_axis',(0.364399348580517,0.,0.931242779705752));
#49604=DIRECTION('ref_axis',(0.931242779705752,0.,-0.364399348580517));
#49605=DIRECTION('',(0.,1.,0.));
#49606=DIRECTION('center_axis',(-0.624280230025758,0.,0.781200482846104));
#49607=DIRECTION('ref_axis',(0.781200482846104,0.,0.624280230025758));
#49608=DIRECTION('',(0.,1.,0.));
#49609=DIRECTION('center_axis',(-0.988679578606275,0.,-0.150042296859647));
#49610=DIRECTION('ref_axis',(-0.150042296859647,0.,0.988679578606275));
#49611=DIRECTION('',(0.,1.,0.));
#49612=DIRECTION('center_axis',(-0.364399348580519,0.,-0.931242779705751));
#49613=DIRECTION('ref_axis',(-0.931242779705751,0.,0.364399348580519));
#49614=DIRECTION('',(0.,1.,0.));
#49615=DIRECTION('center_axis',(0.624280230025758,0.,-0.781200482846105));
#49616=DIRECTION('ref_axis',(-0.781200482846105,0.,-0.624280230025758));
#49617=DIRECTION('center_axis',(0.988679578606276,0.,0.150042296859641));
#49618=DIRECTION('ref_axis',(0.150042296859641,0.,-0.988679578606276));
#49619=DIRECTION('',(0.,1.,0.));
#49620=DIRECTION('',(0.,1.,0.));
#49621=DIRECTION('center_axis',(0.364399348580517,0.,0.931242779705752));
#49622=DIRECTION('ref_axis',(0.931242779705752,0.,-0.364399348580517));
#49623=DIRECTION('',(0.,1.,0.));
#49624=DIRECTION('center_axis',(-0.624280230025758,0.,0.781200482846104));
#49625=DIRECTION('ref_axis',(0.781200482846104,0.,0.624280230025758));
#49626=DIRECTION('',(0.,1.,0.));
#49627=DIRECTION('center_axis',(-0.988679578606275,0.,-0.150042296859647));
#49628=DIRECTION('ref_axis',(-0.150042296859647,0.,0.988679578606275));
#49629=DIRECTION('',(0.,1.,0.));
#49630=DIRECTION('center_axis',(-0.364399348580519,0.,-0.931242779705751));
#49631=DIRECTION('ref_axis',(-0.931242779705751,0.,0.364399348580519));
#49632=DIRECTION('',(0.,1.,0.));
#49633=DIRECTION('center_axis',(0.624280230025758,0.,-0.781200482846105));
#49634=DIRECTION('ref_axis',(-0.781200482846105,0.,-0.624280230025758));
#49635=DIRECTION('center_axis',(0.988679578606276,0.,0.150042296859641));
#49636=DIRECTION('ref_axis',(0.150042296859641,0.,-0.988679578606276));
#49637=DIRECTION('',(0.,1.,0.));
#49638=DIRECTION('',(0.,1.,0.));
#49639=DIRECTION('center_axis',(0.364399348580517,0.,0.931242779705752));
#49640=DIRECTION('ref_axis',(0.931242779705752,0.,-0.364399348580517));
#49641=DIRECTION('',(0.,1.,0.));
#49642=DIRECTION('center_axis',(-0.624280230025758,0.,0.781200482846104));
#49643=DIRECTION('ref_axis',(0.781200482846104,0.,0.624280230025758));
#49644=DIRECTION('',(0.,1.,0.));
#49645=DIRECTION('center_axis',(-0.988679578606275,0.,-0.150042296859647));
#49646=DIRECTION('ref_axis',(-0.150042296859647,0.,0.988679578606275));
#49647=DIRECTION('',(0.,1.,0.));
#49648=DIRECTION('center_axis',(-0.364399348580519,0.,-0.931242779705751));
#49649=DIRECTION('ref_axis',(-0.931242779705751,0.,0.364399348580519));
#49650=DIRECTION('',(0.,1.,0.));
#49651=DIRECTION('center_axis',(0.624280230025758,0.,-0.781200482846105));
#49652=DIRECTION('ref_axis',(-0.781200482846105,0.,-0.624280230025758));
#49653=DIRECTION('center_axis',(0.988679578606276,0.,0.150042296859641));
#49654=DIRECTION('ref_axis',(0.150042296859641,0.,-0.988679578606276));
#49655=DIRECTION('',(0.,1.,0.));
#49656=DIRECTION('',(0.,1.,0.));
#49657=DIRECTION('center_axis',(0.364399348580517,0.,0.931242779705752));
#49658=DIRECTION('ref_axis',(0.931242779705752,0.,-0.364399348580517));
#49659=DIRECTION('',(0.,1.,0.));
#49660=DIRECTION('center_axis',(-0.624280230025758,0.,0.781200482846104));
#49661=DIRECTION('ref_axis',(0.781200482846104,0.,0.624280230025758));
#49662=DIRECTION('',(0.,1.,0.));
#49663=DIRECTION('center_axis',(-0.988679578606275,0.,-0.150042296859647));
#49664=DIRECTION('ref_axis',(-0.150042296859647,0.,0.988679578606275));
#49665=DIRECTION('',(0.,1.,0.));
#49666=DIRECTION('center_axis',(-0.364399348580519,0.,-0.931242779705751));
#49667=DIRECTION('ref_axis',(-0.931242779705751,0.,0.364399348580519));
#49668=DIRECTION('',(0.,1.,0.));
#49669=DIRECTION('center_axis',(0.624280230025758,0.,-0.781200482846105));
#49670=DIRECTION('ref_axis',(-0.781200482846105,0.,-0.624280230025758));
#49671=DIRECTION('center_axis',(0.988679578606276,0.,0.150042296859641));
#49672=DIRECTION('ref_axis',(0.150042296859641,0.,-0.988679578606276));
#49673=DIRECTION('',(0.,1.,0.));
#49674=DIRECTION('',(0.,1.,0.));
#49675=DIRECTION('center_axis',(0.364399348580517,0.,0.931242779705752));
#49676=DIRECTION('ref_axis',(0.931242779705752,0.,-0.364399348580517));
#49677=DIRECTION('',(0.,1.,0.));
#49678=DIRECTION('center_axis',(-0.624280230025758,0.,0.781200482846104));
#49679=DIRECTION('ref_axis',(0.781200482846104,0.,0.624280230025758));
#49680=DIRECTION('',(0.,1.,0.));
#49681=DIRECTION('center_axis',(-0.988679578606275,0.,-0.150042296859647));
#49682=DIRECTION('ref_axis',(-0.150042296859647,0.,0.988679578606275));
#49683=DIRECTION('',(0.,1.,0.));
#49684=DIRECTION('center_axis',(-0.364399348580519,0.,-0.931242779705751));
#49685=DIRECTION('ref_axis',(-0.931242779705751,0.,0.364399348580519));
#49686=DIRECTION('',(0.,1.,0.));
#49687=DIRECTION('center_axis',(0.624280230025758,0.,-0.781200482846105));
#49688=DIRECTION('ref_axis',(-0.781200482846105,0.,-0.624280230025758));
#49689=DIRECTION('center_axis',(0.988679578606276,0.,0.150042296859641));
#49690=DIRECTION('ref_axis',(0.150042296859641,0.,-0.988679578606276));
#49691=DIRECTION('',(0.,1.,0.));
#49692=DIRECTION('',(0.,1.,0.));
#49693=DIRECTION('center_axis',(0.364399348580517,0.,0.931242779705752));
#49694=DIRECTION('ref_axis',(0.931242779705752,0.,-0.364399348580517));
#49695=DIRECTION('',(0.,1.,0.));
#49696=DIRECTION('center_axis',(-0.624280230025758,0.,0.781200482846104));
#49697=DIRECTION('ref_axis',(0.781200482846104,0.,0.624280230025758));
#49698=DIRECTION('',(0.,1.,0.));
#49699=DIRECTION('center_axis',(-0.988679578606275,0.,-0.150042296859647));
#49700=DIRECTION('ref_axis',(-0.150042296859647,0.,0.988679578606275));
#49701=DIRECTION('',(0.,1.,0.));
#49702=DIRECTION('center_axis',(-0.364399348580519,0.,-0.931242779705751));
#49703=DIRECTION('ref_axis',(-0.931242779705751,0.,0.364399348580519));
#49704=DIRECTION('',(0.,1.,0.));
#49705=DIRECTION('center_axis',(0.624280230025758,0.,-0.781200482846105));
#49706=DIRECTION('ref_axis',(-0.781200482846105,0.,-0.624280230025758));
#49707=DIRECTION('center_axis',(0.988679578606276,0.,0.150042296859641));
#49708=DIRECTION('ref_axis',(0.150042296859641,0.,-0.988679578606276));
#49709=DIRECTION('',(0.,1.,0.));
#49710=DIRECTION('',(0.,1.,0.));
#49711=DIRECTION('center_axis',(0.364399348580517,0.,0.931242779705752));
#49712=DIRECTION('ref_axis',(0.931242779705752,0.,-0.364399348580517));
#49713=DIRECTION('',(0.,1.,0.));
#49714=DIRECTION('center_axis',(-0.624280230025758,0.,0.781200482846104));
#49715=DIRECTION('ref_axis',(0.781200482846104,0.,0.624280230025758));
#49716=DIRECTION('',(0.,1.,0.));
#49717=DIRECTION('center_axis',(-0.988679578606275,0.,-0.150042296859647));
#49718=DIRECTION('ref_axis',(-0.150042296859647,0.,0.988679578606275));
#49719=DIRECTION('',(0.,1.,0.));
#49720=DIRECTION('center_axis',(-0.364399348580519,0.,-0.931242779705751));
#49721=DIRECTION('ref_axis',(-0.931242779705751,0.,0.364399348580519));
#49722=DIRECTION('',(0.,1.,0.));
#49723=DIRECTION('center_axis',(0.624280230025758,0.,-0.781200482846105));
#49724=DIRECTION('ref_axis',(-0.781200482846105,0.,-0.624280230025758));
#49725=DIRECTION('center_axis',(0.988679578606276,0.,0.150042296859641));
#49726=DIRECTION('ref_axis',(0.150042296859641,0.,-0.988679578606276));
#49727=DIRECTION('',(0.,1.,0.));
#49728=DIRECTION('',(0.,1.,0.));
#49729=DIRECTION('center_axis',(0.364399348580517,0.,0.931242779705752));
#49730=DIRECTION('ref_axis',(0.931242779705752,0.,-0.364399348580517));
#49731=DIRECTION('',(0.,1.,0.));
#49732=DIRECTION('center_axis',(-0.624280230025758,0.,0.781200482846104));
#49733=DIRECTION('ref_axis',(0.781200482846104,0.,0.624280230025758));
#49734=DIRECTION('',(0.,1.,0.));
#49735=DIRECTION('center_axis',(-0.988679578606275,0.,-0.150042296859647));
#49736=DIRECTION('ref_axis',(-0.150042296859647,0.,0.988679578606275));
#49737=DIRECTION('',(0.,1.,0.));
#49738=DIRECTION('center_axis',(-0.364399348580519,0.,-0.931242779705751));
#49739=DIRECTION('ref_axis',(-0.931242779705751,0.,0.364399348580519));
#49740=DIRECTION('',(0.,1.,0.));
#49741=DIRECTION('center_axis',(0.624280230025758,0.,-0.781200482846105));
#49742=DIRECTION('ref_axis',(-0.781200482846105,0.,-0.624280230025758));
#49743=DIRECTION('center_axis',(0.988679578606276,0.,0.150042296859641));
#49744=DIRECTION('ref_axis',(0.150042296859641,0.,-0.988679578606276));
#49745=DIRECTION('',(0.,1.,0.));
#49746=DIRECTION('',(0.,1.,0.));
#49747=DIRECTION('center_axis',(0.364399348580517,0.,0.931242779705752));
#49748=DIRECTION('ref_axis',(0.931242779705752,0.,-0.364399348580517));
#49749=DIRECTION('',(0.,1.,0.));
#49750=DIRECTION('center_axis',(-0.624280230025758,0.,0.781200482846104));
#49751=DIRECTION('ref_axis',(0.781200482846104,0.,0.624280230025758));
#49752=DIRECTION('',(0.,1.,0.));
#49753=DIRECTION('center_axis',(-0.988679578606275,0.,-0.150042296859647));
#49754=DIRECTION('ref_axis',(-0.150042296859647,0.,0.988679578606275));
#49755=DIRECTION('',(0.,1.,0.));
#49756=DIRECTION('center_axis',(-0.364399348580519,0.,-0.931242779705751));
#49757=DIRECTION('ref_axis',(-0.931242779705751,0.,0.364399348580519));
#49758=DIRECTION('',(0.,1.,0.));
#49759=DIRECTION('center_axis',(0.624280230025758,0.,-0.781200482846105));
#49760=DIRECTION('ref_axis',(-0.781200482846105,0.,-0.624280230025758));
#49761=DIRECTION('center_axis',(0.988679578606276,0.,0.150042296859641));
#49762=DIRECTION('ref_axis',(0.150042296859641,0.,-0.988679578606276));
#49763=DIRECTION('',(0.,1.,0.));
#49764=DIRECTION('',(0.,1.,0.));
#49765=DIRECTION('center_axis',(0.364399348580517,0.,0.931242779705752));
#49766=DIRECTION('ref_axis',(0.931242779705752,0.,-0.364399348580517));
#49767=DIRECTION('',(0.,1.,0.));
#49768=DIRECTION('center_axis',(-0.624280230025758,0.,0.781200482846104));
#49769=DIRECTION('ref_axis',(0.781200482846104,0.,0.624280230025758));
#49770=DIRECTION('',(0.,1.,0.));
#49771=DIRECTION('center_axis',(-0.988679578606275,0.,-0.150042296859647));
#49772=DIRECTION('ref_axis',(-0.150042296859647,0.,0.988679578606275));
#49773=DIRECTION('',(0.,1.,0.));
#49774=DIRECTION('center_axis',(-0.364399348580519,0.,-0.931242779705751));
#49775=DIRECTION('ref_axis',(-0.931242779705751,0.,0.364399348580519));
#49776=DIRECTION('',(0.,1.,0.));
#49777=DIRECTION('center_axis',(0.624280230025758,0.,-0.781200482846105));
#49778=DIRECTION('ref_axis',(-0.781200482846105,0.,-0.624280230025758));
#49779=DIRECTION('center_axis',(0.988679578606276,0.,0.150042296859641));
#49780=DIRECTION('ref_axis',(0.150042296859641,0.,-0.988679578606276));
#49781=DIRECTION('',(0.,1.,0.));
#49782=DIRECTION('',(0.,1.,0.));
#49783=DIRECTION('center_axis',(0.364399348580517,0.,0.931242779705752));
#49784=DIRECTION('ref_axis',(0.931242779705752,0.,-0.364399348580517));
#49785=DIRECTION('',(0.,1.,0.));
#49786=DIRECTION('center_axis',(-0.624280230025758,0.,0.781200482846104));
#49787=DIRECTION('ref_axis',(0.781200482846104,0.,0.624280230025758));
#49788=DIRECTION('',(0.,1.,0.));
#49789=DIRECTION('center_axis',(-0.988679578606275,0.,-0.150042296859647));
#49790=DIRECTION('ref_axis',(-0.150042296859647,0.,0.988679578606275));
#49791=DIRECTION('',(0.,1.,0.));
#49792=DIRECTION('center_axis',(-0.364399348580519,0.,-0.931242779705751));
#49793=DIRECTION('ref_axis',(-0.931242779705751,0.,0.364399348580519));
#49794=DIRECTION('',(0.,1.,0.));
#49795=DIRECTION('center_axis',(0.624280230025758,0.,-0.781200482846105));
#49796=DIRECTION('ref_axis',(-0.781200482846105,0.,-0.624280230025758));
#49797=DIRECTION('center_axis',(0.988679578606276,0.,0.150042296859641));
#49798=DIRECTION('ref_axis',(0.150042296859641,0.,-0.988679578606276));
#49799=DIRECTION('',(0.,1.,0.));
#49800=DIRECTION('',(0.,1.,0.));
#49801=DIRECTION('center_axis',(0.364399348580517,0.,0.931242779705752));
#49802=DIRECTION('ref_axis',(0.931242779705752,0.,-0.364399348580517));
#49803=DIRECTION('',(0.,1.,0.));
#49804=DIRECTION('center_axis',(-0.624280230025758,0.,0.781200482846104));
#49805=DIRECTION('ref_axis',(0.781200482846104,0.,0.624280230025758));
#49806=DIRECTION('',(0.,1.,0.));
#49807=DIRECTION('center_axis',(-0.988679578606275,0.,-0.150042296859647));
#49808=DIRECTION('ref_axis',(-0.150042296859647,0.,0.988679578606275));
#49809=DIRECTION('',(0.,1.,0.));
#49810=DIRECTION('center_axis',(-0.364399348580519,0.,-0.931242779705751));
#49811=DIRECTION('ref_axis',(-0.931242779705751,0.,0.364399348580519));
#49812=DIRECTION('',(0.,1.,0.));
#49813=DIRECTION('center_axis',(0.624280230025758,0.,-0.781200482846105));
#49814=DIRECTION('ref_axis',(-0.781200482846105,0.,-0.624280230025758));
#49815=DIRECTION('center_axis',(0.988679578606276,0.,0.150042296859641));
#49816=DIRECTION('ref_axis',(0.150042296859641,0.,-0.988679578606276));
#49817=DIRECTION('',(0.,1.,0.));
#49818=DIRECTION('',(0.,1.,0.));
#49819=DIRECTION('center_axis',(0.364399348580517,0.,0.931242779705752));
#49820=DIRECTION('ref_axis',(0.931242779705752,0.,-0.364399348580517));
#49821=DIRECTION('',(0.,1.,0.));
#49822=DIRECTION('center_axis',(-0.624280230025758,0.,0.781200482846104));
#49823=DIRECTION('ref_axis',(0.781200482846104,0.,0.624280230025758));
#49824=DIRECTION('',(0.,1.,0.));
#49825=DIRECTION('center_axis',(-0.988679578606275,0.,-0.150042296859647));
#49826=DIRECTION('ref_axis',(-0.150042296859647,0.,0.988679578606275));
#49827=DIRECTION('',(0.,1.,0.));
#49828=DIRECTION('center_axis',(-0.364399348580519,0.,-0.931242779705751));
#49829=DIRECTION('ref_axis',(-0.931242779705751,0.,0.364399348580519));
#49830=DIRECTION('',(0.,1.,0.));
#49831=DIRECTION('center_axis',(0.624280230025758,0.,-0.781200482846105));
#49832=DIRECTION('ref_axis',(-0.781200482846105,0.,-0.624280230025758));
#49833=DIRECTION('center_axis',(0.988679578606276,0.,0.150042296859641));
#49834=DIRECTION('ref_axis',(0.150042296859641,0.,-0.988679578606276));
#49835=DIRECTION('',(0.,1.,0.));
#49836=DIRECTION('',(0.,1.,0.));
#49837=DIRECTION('center_axis',(0.364399348580517,0.,0.931242779705752));
#49838=DIRECTION('ref_axis',(0.931242779705752,0.,-0.364399348580517));
#49839=DIRECTION('',(0.,1.,0.));
#49840=DIRECTION('center_axis',(-0.624280230025758,0.,0.781200482846104));
#49841=DIRECTION('ref_axis',(0.781200482846104,0.,0.624280230025758));
#49842=DIRECTION('',(0.,1.,0.));
#49843=DIRECTION('center_axis',(-0.988679578606275,0.,-0.150042296859647));
#49844=DIRECTION('ref_axis',(-0.150042296859647,0.,0.988679578606275));
#49845=DIRECTION('',(0.,1.,0.));
#49846=DIRECTION('center_axis',(-0.364399348580519,0.,-0.931242779705751));
#49847=DIRECTION('ref_axis',(-0.931242779705751,0.,0.364399348580519));
#49848=DIRECTION('',(0.,1.,0.));
#49849=DIRECTION('center_axis',(0.624280230025758,0.,-0.781200482846105));
#49850=DIRECTION('ref_axis',(-0.781200482846105,0.,-0.624280230025758));
#49851=DIRECTION('center_axis',(0.988679578606276,0.,0.150042296859641));
#49852=DIRECTION('ref_axis',(0.150042296859641,0.,-0.988679578606276));
#49853=DIRECTION('',(0.,1.,0.));
#49854=DIRECTION('',(0.,1.,0.));
#49855=DIRECTION('center_axis',(0.364399348580517,0.,0.931242779705752));
#49856=DIRECTION('ref_axis',(0.931242779705752,0.,-0.364399348580517));
#49857=DIRECTION('',(0.,1.,0.));
#49858=DIRECTION('center_axis',(-0.624280230025758,0.,0.781200482846104));
#49859=DIRECTION('ref_axis',(0.781200482846104,0.,0.624280230025758));
#49860=DIRECTION('',(0.,1.,0.));
#49861=DIRECTION('center_axis',(-0.988679578606275,0.,-0.150042296859647));
#49862=DIRECTION('ref_axis',(-0.150042296859647,0.,0.988679578606275));
#49863=DIRECTION('',(0.,1.,0.));
#49864=DIRECTION('center_axis',(-0.364399348580519,0.,-0.931242779705751));
#49865=DIRECTION('ref_axis',(-0.931242779705751,0.,0.364399348580519));
#49866=DIRECTION('',(0.,1.,0.));
#49867=DIRECTION('center_axis',(0.624280230025758,0.,-0.781200482846105));
#49868=DIRECTION('ref_axis',(-0.781200482846105,0.,-0.624280230025758));
#49869=DIRECTION('center_axis',(0.988679578606276,0.,0.150042296859641));
#49870=DIRECTION('ref_axis',(0.150042296859641,0.,-0.988679578606276));
#49871=DIRECTION('',(0.,1.,0.));
#49872=DIRECTION('',(0.,1.,0.));
#49873=DIRECTION('center_axis',(0.364399348580517,0.,0.931242779705752));
#49874=DIRECTION('ref_axis',(0.931242779705752,0.,-0.364399348580517));
#49875=DIRECTION('',(0.,1.,0.));
#49876=DIRECTION('center_axis',(-0.624280230025758,0.,0.781200482846104));
#49877=DIRECTION('ref_axis',(0.781200482846104,0.,0.624280230025758));
#49878=DIRECTION('',(0.,1.,0.));
#49879=DIRECTION('center_axis',(-0.988679578606275,0.,-0.150042296859647));
#49880=DIRECTION('ref_axis',(-0.150042296859647,0.,0.988679578606275));
#49881=DIRECTION('',(0.,1.,0.));
#49882=DIRECTION('center_axis',(-0.364399348580519,0.,-0.931242779705751));
#49883=DIRECTION('ref_axis',(-0.931242779705751,0.,0.364399348580519));
#49884=DIRECTION('',(0.,1.,0.));
#49885=DIRECTION('center_axis',(0.624280230025758,0.,-0.781200482846105));
#49886=DIRECTION('ref_axis',(-0.781200482846105,0.,-0.624280230025758));
#49887=DIRECTION('center_axis',(0.988679578606276,0.,0.150042296859641));
#49888=DIRECTION('ref_axis',(0.150042296859641,0.,-0.988679578606276));
#49889=DIRECTION('',(0.,1.,0.));
#49890=DIRECTION('',(0.,1.,0.));
#49891=DIRECTION('center_axis',(0.364399348580517,0.,0.931242779705752));
#49892=DIRECTION('ref_axis',(0.931242779705752,0.,-0.364399348580517));
#49893=DIRECTION('',(0.,1.,0.));
#49894=DIRECTION('center_axis',(-0.624280230025758,0.,0.781200482846104));
#49895=DIRECTION('ref_axis',(0.781200482846104,0.,0.624280230025758));
#49896=DIRECTION('',(0.,1.,0.));
#49897=DIRECTION('center_axis',(-0.988679578606275,0.,-0.150042296859647));
#49898=DIRECTION('ref_axis',(-0.150042296859647,0.,0.988679578606275));
#49899=DIRECTION('',(0.,1.,0.));
#49900=DIRECTION('center_axis',(-0.364399348580519,0.,-0.931242779705751));
#49901=DIRECTION('ref_axis',(-0.931242779705751,0.,0.364399348580519));
#49902=DIRECTION('',(0.,1.,0.));
#49903=DIRECTION('center_axis',(0.624280230025758,0.,-0.781200482846105));
#49904=DIRECTION('ref_axis',(-0.781200482846105,0.,-0.624280230025758));
#49905=DIRECTION('center_axis',(0.988679578606276,0.,0.150042296859641));
#49906=DIRECTION('ref_axis',(0.150042296859641,0.,-0.988679578606276));
#49907=DIRECTION('',(0.,1.,0.));
#49908=DIRECTION('',(0.,1.,0.));
#49909=DIRECTION('center_axis',(0.364399348580517,0.,0.931242779705752));
#49910=DIRECTION('ref_axis',(0.931242779705752,0.,-0.364399348580517));
#49911=DIRECTION('',(0.,1.,0.));
#49912=DIRECTION('center_axis',(-0.624280230025758,0.,0.781200482846104));
#49913=DIRECTION('ref_axis',(0.781200482846104,0.,0.624280230025758));
#49914=DIRECTION('',(0.,1.,0.));
#49915=DIRECTION('center_axis',(-0.988679578606275,0.,-0.150042296859647));
#49916=DIRECTION('ref_axis',(-0.150042296859647,0.,0.988679578606275));
#49917=DIRECTION('',(0.,1.,0.));
#49918=DIRECTION('center_axis',(-0.364399348580519,0.,-0.931242779705751));
#49919=DIRECTION('ref_axis',(-0.931242779705751,0.,0.364399348580519));
#49920=DIRECTION('',(0.,1.,0.));
#49921=DIRECTION('center_axis',(0.624280230025758,0.,-0.781200482846105));
#49922=DIRECTION('ref_axis',(-0.781200482846105,0.,-0.624280230025758));
#49923=DIRECTION('center_axis',(0.988679578606276,0.,0.150042296859641));
#49924=DIRECTION('ref_axis',(0.150042296859641,0.,-0.988679578606276));
#49925=DIRECTION('',(0.,1.,0.));
#49926=DIRECTION('',(0.,1.,0.));
#49927=DIRECTION('center_axis',(0.364399348580517,0.,0.931242779705752));
#49928=DIRECTION('ref_axis',(0.931242779705752,0.,-0.364399348580517));
#49929=DIRECTION('',(0.,1.,0.));
#49930=DIRECTION('center_axis',(-0.624280230025758,0.,0.781200482846104));
#49931=DIRECTION('ref_axis',(0.781200482846104,0.,0.624280230025758));
#49932=DIRECTION('',(0.,1.,0.));
#49933=DIRECTION('center_axis',(-0.988679578606275,0.,-0.150042296859647));
#49934=DIRECTION('ref_axis',(-0.150042296859647,0.,0.988679578606275));
#49935=DIRECTION('',(0.,1.,0.));
#49936=DIRECTION('center_axis',(-0.364399348580519,0.,-0.931242779705751));
#49937=DIRECTION('ref_axis',(-0.931242779705751,0.,0.364399348580519));
#49938=DIRECTION('',(0.,1.,0.));
#49939=DIRECTION('center_axis',(0.624280230025758,0.,-0.781200482846105));
#49940=DIRECTION('ref_axis',(-0.781200482846105,0.,-0.624280230025758));
#49941=DIRECTION('center_axis',(0.988679578606276,0.,0.150042296859641));
#49942=DIRECTION('ref_axis',(0.150042296859641,0.,-0.988679578606276));
#49943=DIRECTION('',(0.,1.,0.));
#49944=DIRECTION('',(0.,1.,0.));
#49945=DIRECTION('center_axis',(0.364399348580517,0.,0.931242779705752));
#49946=DIRECTION('ref_axis',(0.931242779705752,0.,-0.364399348580517));
#49947=DIRECTION('',(0.,1.,0.));
#49948=DIRECTION('center_axis',(-0.624280230025758,0.,0.781200482846104));
#49949=DIRECTION('ref_axis',(0.781200482846104,0.,0.624280230025758));
#49950=DIRECTION('',(0.,1.,0.));
#49951=DIRECTION('center_axis',(-0.988679578606275,0.,-0.150042296859647));
#49952=DIRECTION('ref_axis',(-0.150042296859647,0.,0.988679578606275));
#49953=DIRECTION('',(0.,1.,0.));
#49954=DIRECTION('center_axis',(-0.364399348580519,0.,-0.931242779705751));
#49955=DIRECTION('ref_axis',(-0.931242779705751,0.,0.364399348580519));
#49956=DIRECTION('',(0.,1.,0.));
#49957=DIRECTION('center_axis',(0.624280230025758,0.,-0.781200482846105));
#49958=DIRECTION('ref_axis',(-0.781200482846105,0.,-0.624280230025758));
#49959=DIRECTION('center_axis',(0.988679578606276,0.,0.150042296859641));
#49960=DIRECTION('ref_axis',(0.150042296859641,0.,-0.988679578606276));
#49961=DIRECTION('',(0.,1.,0.));
#49962=DIRECTION('',(0.,1.,0.));
#49963=DIRECTION('center_axis',(0.364399348580517,0.,0.931242779705752));
#49964=DIRECTION('ref_axis',(0.931242779705752,0.,-0.364399348580517));
#49965=DIRECTION('',(0.,1.,0.));
#49966=DIRECTION('center_axis',(-0.624280230025758,0.,0.781200482846104));
#49967=DIRECTION('ref_axis',(0.781200482846104,0.,0.624280230025758));
#49968=DIRECTION('',(0.,1.,0.));
#49969=DIRECTION('center_axis',(-0.988679578606275,0.,-0.150042296859647));
#49970=DIRECTION('ref_axis',(-0.150042296859647,0.,0.988679578606275));
#49971=DIRECTION('',(0.,1.,0.));
#49972=DIRECTION('center_axis',(-0.364399348580519,0.,-0.931242779705751));
#49973=DIRECTION('ref_axis',(-0.931242779705751,0.,0.364399348580519));
#49974=DIRECTION('',(0.,1.,0.));
#49975=DIRECTION('center_axis',(0.624280230025758,0.,-0.781200482846105));
#49976=DIRECTION('ref_axis',(-0.781200482846105,0.,-0.624280230025758));
#49977=DIRECTION('center_axis',(0.988679578606276,0.,0.150042296859641));
#49978=DIRECTION('ref_axis',(0.150042296859641,0.,-0.988679578606276));
#49979=DIRECTION('',(0.,1.,0.));
#49980=DIRECTION('',(0.,1.,0.));
#49981=DIRECTION('center_axis',(0.364399348580517,0.,0.931242779705752));
#49982=DIRECTION('ref_axis',(0.931242779705752,0.,-0.364399348580517));
#49983=DIRECTION('',(0.,1.,0.));
#49984=DIRECTION('center_axis',(-0.624280230025758,0.,0.781200482846104));
#49985=DIRECTION('ref_axis',(0.781200482846104,0.,0.624280230025758));
#49986=DIRECTION('',(0.,1.,0.));
#49987=DIRECTION('center_axis',(-0.988679578606275,0.,-0.150042296859647));
#49988=DIRECTION('ref_axis',(-0.150042296859647,0.,0.988679578606275));
#49989=DIRECTION('',(0.,1.,0.));
#49990=DIRECTION('center_axis',(-0.364399348580519,0.,-0.931242779705751));
#49991=DIRECTION('ref_axis',(-0.931242779705751,0.,0.364399348580519));
#49992=DIRECTION('',(0.,1.,0.));
#49993=DIRECTION('center_axis',(0.624280230025758,0.,-0.781200482846105));
#49994=DIRECTION('ref_axis',(-0.781200482846105,0.,-0.624280230025758));
#49995=DIRECTION('center_axis',(0.988679578606276,0.,0.150042296859641));
#49996=DIRECTION('ref_axis',(0.150042296859641,0.,-0.988679578606276));
#49997=DIRECTION('',(0.,1.,0.));
#49998=DIRECTION('',(0.,1.,0.));
#49999=DIRECTION('center_axis',(0.364399348580517,0.,0.931242779705752));
#50000=DIRECTION('ref_axis',(0.931242779705752,0.,-0.364399348580517));
#50001=DIRECTION('',(0.,1.,0.));
#50002=DIRECTION('center_axis',(-0.624280230025758,0.,0.781200482846104));
#50003=DIRECTION('ref_axis',(0.781200482846104,0.,0.624280230025758));
#50004=DIRECTION('',(0.,1.,0.));
#50005=DIRECTION('center_axis',(-0.988679578606275,0.,-0.150042296859647));
#50006=DIRECTION('ref_axis',(-0.150042296859647,0.,0.988679578606275));
#50007=DIRECTION('',(0.,1.,0.));
#50008=DIRECTION('center_axis',(-0.364399348580519,0.,-0.931242779705751));
#50009=DIRECTION('ref_axis',(-0.931242779705751,0.,0.364399348580519));
#50010=DIRECTION('',(0.,1.,0.));
#50011=DIRECTION('center_axis',(0.624280230025758,0.,-0.781200482846105));
#50012=DIRECTION('ref_axis',(-0.781200482846105,0.,-0.624280230025758));
#50013=DIRECTION('center_axis',(0.988679578606276,0.,0.150042296859641));
#50014=DIRECTION('ref_axis',(0.150042296859641,0.,-0.988679578606276));
#50015=DIRECTION('',(0.,1.,0.));
#50016=DIRECTION('',(0.,1.,0.));
#50017=DIRECTION('center_axis',(0.364399348580517,0.,0.931242779705752));
#50018=DIRECTION('ref_axis',(0.931242779705752,0.,-0.364399348580517));
#50019=DIRECTION('',(0.,1.,0.));
#50020=DIRECTION('center_axis',(-0.624280230025758,0.,0.781200482846104));
#50021=DIRECTION('ref_axis',(0.781200482846104,0.,0.624280230025758));
#50022=DIRECTION('',(0.,1.,0.));
#50023=DIRECTION('center_axis',(-0.988679578606275,0.,-0.150042296859647));
#50024=DIRECTION('ref_axis',(-0.150042296859647,0.,0.988679578606275));
#50025=DIRECTION('',(0.,1.,0.));
#50026=DIRECTION('center_axis',(-0.364399348580519,0.,-0.931242779705751));
#50027=DIRECTION('ref_axis',(-0.931242779705751,0.,0.364399348580519));
#50028=DIRECTION('',(0.,1.,0.));
#50029=DIRECTION('center_axis',(0.624280230025758,0.,-0.781200482846105));
#50030=DIRECTION('ref_axis',(-0.781200482846105,0.,-0.624280230025758));
#50031=DIRECTION('center_axis',(0.988679578606276,0.,0.150042296859641));
#50032=DIRECTION('ref_axis',(0.150042296859641,0.,-0.988679578606276));
#50033=DIRECTION('',(0.,1.,0.));
#50034=DIRECTION('',(0.,1.,0.));
#50035=DIRECTION('center_axis',(0.364399348580517,0.,0.931242779705752));
#50036=DIRECTION('ref_axis',(0.931242779705752,0.,-0.364399348580517));
#50037=DIRECTION('',(0.,1.,0.));
#50038=DIRECTION('center_axis',(-0.624280230025758,0.,0.781200482846104));
#50039=DIRECTION('ref_axis',(0.781200482846104,0.,0.624280230025758));
#50040=DIRECTION('',(0.,1.,0.));
#50041=DIRECTION('center_axis',(-0.988679578606275,0.,-0.150042296859647));
#50042=DIRECTION('ref_axis',(-0.150042296859647,0.,0.988679578606275));
#50043=DIRECTION('',(0.,1.,0.));
#50044=DIRECTION('center_axis',(-0.364399348580519,0.,-0.931242779705751));
#50045=DIRECTION('ref_axis',(-0.931242779705751,0.,0.364399348580519));
#50046=DIRECTION('',(0.,1.,0.));
#50047=DIRECTION('center_axis',(0.624280230025758,0.,-0.781200482846105));
#50048=DIRECTION('ref_axis',(-0.781200482846105,0.,-0.624280230025758));
#50049=DIRECTION('center_axis',(0.988679578606276,0.,0.150042296859641));
#50050=DIRECTION('ref_axis',(0.150042296859641,0.,-0.988679578606276));
#50051=DIRECTION('',(0.,1.,0.));
#50052=DIRECTION('',(0.,1.,0.));
#50053=DIRECTION('center_axis',(0.364399348580517,0.,0.931242779705752));
#50054=DIRECTION('ref_axis',(0.931242779705752,0.,-0.364399348580517));
#50055=DIRECTION('',(0.,1.,0.));
#50056=DIRECTION('center_axis',(-0.624280230025758,0.,0.781200482846104));
#50057=DIRECTION('ref_axis',(0.781200482846104,0.,0.624280230025758));
#50058=DIRECTION('',(0.,1.,0.));
#50059=DIRECTION('center_axis',(-0.988679578606275,0.,-0.150042296859647));
#50060=DIRECTION('ref_axis',(-0.150042296859647,0.,0.988679578606275));
#50061=DIRECTION('',(0.,1.,0.));
#50062=DIRECTION('center_axis',(-0.364399348580519,0.,-0.931242779705751));
#50063=DIRECTION('ref_axis',(-0.931242779705751,0.,0.364399348580519));
#50064=DIRECTION('',(0.,1.,0.));
#50065=DIRECTION('center_axis',(0.624280230025758,0.,-0.781200482846105));
#50066=DIRECTION('ref_axis',(-0.781200482846105,0.,-0.624280230025758));
#50067=DIRECTION('center_axis',(0.988679578606276,0.,0.150042296859641));
#50068=DIRECTION('ref_axis',(0.150042296859641,0.,-0.988679578606276));
#50069=DIRECTION('',(0.,1.,0.));
#50070=DIRECTION('',(0.,1.,0.));
#50071=DIRECTION('center_axis',(0.364399348580517,0.,0.931242779705752));
#50072=DIRECTION('ref_axis',(0.931242779705752,0.,-0.364399348580517));
#50073=DIRECTION('',(0.,1.,0.));
#50074=DIRECTION('center_axis',(-0.624280230025758,0.,0.781200482846104));
#50075=DIRECTION('ref_axis',(0.781200482846104,0.,0.624280230025758));
#50076=DIRECTION('',(0.,1.,0.));
#50077=DIRECTION('center_axis',(-0.988679578606275,0.,-0.150042296859647));
#50078=DIRECTION('ref_axis',(-0.150042296859647,0.,0.988679578606275));
#50079=DIRECTION('',(0.,1.,0.));
#50080=DIRECTION('center_axis',(-0.364399348580519,0.,-0.931242779705751));
#50081=DIRECTION('ref_axis',(-0.931242779705751,0.,0.364399348580519));
#50082=DIRECTION('',(0.,1.,0.));
#50083=DIRECTION('center_axis',(0.624280230025758,0.,-0.781200482846105));
#50084=DIRECTION('ref_axis',(-0.781200482846105,0.,-0.624280230025758));
#50085=DIRECTION('center_axis',(0.988679578606276,0.,0.150042296859641));
#50086=DIRECTION('ref_axis',(0.150042296859641,0.,-0.988679578606276));
#50087=DIRECTION('',(0.,1.,0.));
#50088=DIRECTION('',(0.,1.,0.));
#50089=DIRECTION('center_axis',(0.364399348580517,0.,0.931242779705752));
#50090=DIRECTION('ref_axis',(0.931242779705752,0.,-0.364399348580517));
#50091=DIRECTION('',(0.,1.,0.));
#50092=DIRECTION('center_axis',(-0.624280230025758,0.,0.781200482846104));
#50093=DIRECTION('ref_axis',(0.781200482846104,0.,0.624280230025758));
#50094=DIRECTION('',(0.,1.,0.));
#50095=DIRECTION('center_axis',(-0.988679578606275,0.,-0.150042296859647));
#50096=DIRECTION('ref_axis',(-0.150042296859647,0.,0.988679578606275));
#50097=DIRECTION('',(0.,1.,0.));
#50098=DIRECTION('center_axis',(-0.364399348580519,0.,-0.931242779705751));
#50099=DIRECTION('ref_axis',(-0.931242779705751,0.,0.364399348580519));
#50100=DIRECTION('',(0.,1.,0.));
#50101=DIRECTION('center_axis',(0.624280230025758,0.,-0.781200482846105));
#50102=DIRECTION('ref_axis',(-0.781200482846105,0.,-0.624280230025758));
#50103=DIRECTION('center_axis',(0.988679578606276,0.,0.150042296859641));
#50104=DIRECTION('ref_axis',(0.150042296859641,0.,-0.988679578606276));
#50105=DIRECTION('',(0.,1.,0.));
#50106=DIRECTION('',(0.,1.,0.));
#50107=DIRECTION('center_axis',(0.364399348580517,0.,0.931242779705752));
#50108=DIRECTION('ref_axis',(0.931242779705752,0.,-0.364399348580517));
#50109=DIRECTION('',(0.,1.,0.));
#50110=DIRECTION('center_axis',(-0.624280230025758,0.,0.781200482846104));
#50111=DIRECTION('ref_axis',(0.781200482846104,0.,0.624280230025758));
#50112=DIRECTION('',(0.,1.,0.));
#50113=DIRECTION('center_axis',(-0.988679578606275,0.,-0.150042296859647));
#50114=DIRECTION('ref_axis',(-0.150042296859647,0.,0.988679578606275));
#50115=DIRECTION('',(0.,1.,0.));
#50116=DIRECTION('center_axis',(-0.364399348580519,0.,-0.931242779705751));
#50117=DIRECTION('ref_axis',(-0.931242779705751,0.,0.364399348580519));
#50118=DIRECTION('',(0.,1.,0.));
#50119=DIRECTION('center_axis',(0.624280230025758,0.,-0.781200482846105));
#50120=DIRECTION('ref_axis',(-0.781200482846105,0.,-0.624280230025758));
#50121=DIRECTION('center_axis',(0.988679578606276,0.,0.150042296859641));
#50122=DIRECTION('ref_axis',(0.150042296859641,0.,-0.988679578606276));
#50123=DIRECTION('',(0.,1.,0.));
#50124=DIRECTION('',(0.,1.,0.));
#50125=DIRECTION('center_axis',(0.364399348580517,0.,0.931242779705752));
#50126=DIRECTION('ref_axis',(0.931242779705752,0.,-0.364399348580517));
#50127=DIRECTION('',(0.,1.,0.));
#50128=DIRECTION('center_axis',(-0.624280230025758,0.,0.781200482846104));
#50129=DIRECTION('ref_axis',(0.781200482846104,0.,0.624280230025758));
#50130=DIRECTION('',(0.,1.,0.));
#50131=DIRECTION('center_axis',(-0.988679578606275,0.,-0.150042296859647));
#50132=DIRECTION('ref_axis',(-0.150042296859647,0.,0.988679578606275));
#50133=DIRECTION('',(0.,1.,0.));
#50134=DIRECTION('center_axis',(-0.364399348580519,0.,-0.931242779705751));
#50135=DIRECTION('ref_axis',(-0.931242779705751,0.,0.364399348580519));
#50136=DIRECTION('',(0.,1.,0.));
#50137=DIRECTION('center_axis',(0.624280230025758,0.,-0.781200482846105));
#50138=DIRECTION('ref_axis',(-0.781200482846105,0.,-0.624280230025758));
#50139=DIRECTION('center_axis',(0.988679578606276,0.,0.150042296859641));
#50140=DIRECTION('ref_axis',(0.150042296859641,0.,-0.988679578606276));
#50141=DIRECTION('',(0.,1.,0.));
#50142=DIRECTION('',(0.,1.,0.));
#50143=DIRECTION('center_axis',(0.364399348580517,0.,0.931242779705752));
#50144=DIRECTION('ref_axis',(0.931242779705752,0.,-0.364399348580517));
#50145=DIRECTION('',(0.,1.,0.));
#50146=DIRECTION('center_axis',(-0.624280230025758,0.,0.781200482846104));
#50147=DIRECTION('ref_axis',(0.781200482846104,0.,0.624280230025758));
#50148=DIRECTION('',(0.,1.,0.));
#50149=DIRECTION('center_axis',(-0.988679578606275,0.,-0.150042296859647));
#50150=DIRECTION('ref_axis',(-0.150042296859647,0.,0.988679578606275));
#50151=DIRECTION('',(0.,1.,0.));
#50152=DIRECTION('center_axis',(-0.364399348580519,0.,-0.931242779705751));
#50153=DIRECTION('ref_axis',(-0.931242779705751,0.,0.364399348580519));
#50154=DIRECTION('',(0.,1.,0.));
#50155=DIRECTION('center_axis',(0.624280230025758,0.,-0.781200482846105));
#50156=DIRECTION('ref_axis',(-0.781200482846105,0.,-0.624280230025758));
#50157=DIRECTION('center_axis',(0.988679578606276,0.,0.150042296859641));
#50158=DIRECTION('ref_axis',(0.150042296859641,0.,-0.988679578606276));
#50159=DIRECTION('',(0.,1.,0.));
#50160=DIRECTION('',(0.,1.,0.));
#50161=DIRECTION('center_axis',(0.364399348580517,0.,0.931242779705752));
#50162=DIRECTION('ref_axis',(0.931242779705752,0.,-0.364399348580517));
#50163=DIRECTION('',(0.,1.,0.));
#50164=DIRECTION('center_axis',(-0.624280230025758,0.,0.781200482846104));
#50165=DIRECTION('ref_axis',(0.781200482846104,0.,0.624280230025758));
#50166=DIRECTION('',(0.,1.,0.));
#50167=DIRECTION('center_axis',(-0.988679578606275,0.,-0.150042296859647));
#50168=DIRECTION('ref_axis',(-0.150042296859647,0.,0.988679578606275));
#50169=DIRECTION('',(0.,1.,0.));
#50170=DIRECTION('center_axis',(-0.364399348580519,0.,-0.931242779705751));
#50171=DIRECTION('ref_axis',(-0.931242779705751,0.,0.364399348580519));
#50172=DIRECTION('',(0.,1.,0.));
#50173=DIRECTION('center_axis',(0.624280230025758,0.,-0.781200482846105));
#50174=DIRECTION('ref_axis',(-0.781200482846105,0.,-0.624280230025758));
#50175=DIRECTION('center_axis',(0.988679578606276,0.,0.150042296859641));
#50176=DIRECTION('ref_axis',(0.150042296859641,0.,-0.988679578606276));
#50177=DIRECTION('',(0.,1.,0.));
#50178=DIRECTION('',(0.,1.,0.));
#50179=DIRECTION('center_axis',(0.364399348580517,0.,0.931242779705752));
#50180=DIRECTION('ref_axis',(0.931242779705752,0.,-0.364399348580517));
#50181=DIRECTION('',(0.,1.,0.));
#50182=DIRECTION('center_axis',(-0.624280230025758,0.,0.781200482846104));
#50183=DIRECTION('ref_axis',(0.781200482846104,0.,0.624280230025758));
#50184=DIRECTION('',(0.,1.,0.));
#50185=DIRECTION('center_axis',(-0.988679578606275,0.,-0.150042296859647));
#50186=DIRECTION('ref_axis',(-0.150042296859647,0.,0.988679578606275));
#50187=DIRECTION('',(0.,1.,0.));
#50188=DIRECTION('center_axis',(-0.364399348580519,0.,-0.931242779705751));
#50189=DIRECTION('ref_axis',(-0.931242779705751,0.,0.364399348580519));
#50190=DIRECTION('',(0.,1.,0.));
#50191=DIRECTION('center_axis',(0.624280230025758,0.,-0.781200482846105));
#50192=DIRECTION('ref_axis',(-0.781200482846105,0.,-0.624280230025758));
#50193=DIRECTION('center_axis',(0.988679578606276,0.,0.150042296859641));
#50194=DIRECTION('ref_axis',(0.150042296859641,0.,-0.988679578606276));
#50195=DIRECTION('',(0.,1.,0.));
#50196=DIRECTION('',(0.,1.,0.));
#50197=DIRECTION('center_axis',(0.364399348580517,0.,0.931242779705752));
#50198=DIRECTION('ref_axis',(0.931242779705752,0.,-0.364399348580517));
#50199=DIRECTION('',(0.,1.,0.));
#50200=DIRECTION('center_axis',(-0.624280230025758,0.,0.781200482846104));
#50201=DIRECTION('ref_axis',(0.781200482846104,0.,0.624280230025758));
#50202=DIRECTION('',(0.,1.,0.));
#50203=DIRECTION('center_axis',(-0.988679578606275,0.,-0.150042296859647));
#50204=DIRECTION('ref_axis',(-0.150042296859647,0.,0.988679578606275));
#50205=DIRECTION('',(0.,1.,0.));
#50206=DIRECTION('center_axis',(-0.364399348580519,0.,-0.931242779705751));
#50207=DIRECTION('ref_axis',(-0.931242779705751,0.,0.364399348580519));
#50208=DIRECTION('',(0.,1.,0.));
#50209=DIRECTION('center_axis',(0.624280230025758,0.,-0.781200482846105));
#50210=DIRECTION('ref_axis',(-0.781200482846105,0.,-0.624280230025758));
#50211=DIRECTION('center_axis',(0.988679578606276,0.,0.150042296859641));
#50212=DIRECTION('ref_axis',(0.150042296859641,0.,-0.988679578606276));
#50213=DIRECTION('',(0.,1.,0.));
#50214=DIRECTION('',(0.,1.,0.));
#50215=DIRECTION('center_axis',(0.364399348580517,0.,0.931242779705752));
#50216=DIRECTION('ref_axis',(0.931242779705752,0.,-0.364399348580517));
#50217=DIRECTION('',(0.,1.,0.));
#50218=DIRECTION('center_axis',(-0.624280230025758,0.,0.781200482846104));
#50219=DIRECTION('ref_axis',(0.781200482846104,0.,0.624280230025758));
#50220=DIRECTION('',(0.,1.,0.));
#50221=DIRECTION('center_axis',(-0.988679578606275,0.,-0.150042296859647));
#50222=DIRECTION('ref_axis',(-0.150042296859647,0.,0.988679578606275));
#50223=DIRECTION('',(0.,1.,0.));
#50224=DIRECTION('center_axis',(-0.364399348580519,0.,-0.931242779705751));
#50225=DIRECTION('ref_axis',(-0.931242779705751,0.,0.364399348580519));
#50226=DIRECTION('',(0.,1.,0.));
#50227=DIRECTION('center_axis',(0.624280230025758,0.,-0.781200482846105));
#50228=DIRECTION('ref_axis',(-0.781200482846105,0.,-0.624280230025758));
#50229=DIRECTION('center_axis',(0.988679578606276,0.,0.150042296859641));
#50230=DIRECTION('ref_axis',(0.150042296859641,0.,-0.988679578606276));
#50231=DIRECTION('',(0.,1.,0.));
#50232=DIRECTION('',(0.,1.,0.));
#50233=DIRECTION('center_axis',(0.364399348580517,0.,0.931242779705752));
#50234=DIRECTION('ref_axis',(0.931242779705752,0.,-0.364399348580517));
#50235=DIRECTION('',(0.,1.,0.));
#50236=DIRECTION('center_axis',(-0.624280230025758,0.,0.781200482846104));
#50237=DIRECTION('ref_axis',(0.781200482846104,0.,0.624280230025758));
#50238=DIRECTION('',(0.,1.,0.));
#50239=DIRECTION('center_axis',(-0.988679578606275,0.,-0.150042296859647));
#50240=DIRECTION('ref_axis',(-0.150042296859647,0.,0.988679578606275));
#50241=DIRECTION('',(0.,1.,0.));
#50242=DIRECTION('center_axis',(-0.364399348580519,0.,-0.931242779705751));
#50243=DIRECTION('ref_axis',(-0.931242779705751,0.,0.364399348580519));
#50244=DIRECTION('',(0.,1.,0.));
#50245=DIRECTION('center_axis',(0.624280230025758,0.,-0.781200482846105));
#50246=DIRECTION('ref_axis',(-0.781200482846105,0.,-0.624280230025758));
#50247=DIRECTION('center_axis',(0.988679578606276,0.,0.150042296859641));
#50248=DIRECTION('ref_axis',(0.150042296859641,0.,-0.988679578606276));
#50249=DIRECTION('',(0.,1.,0.));
#50250=DIRECTION('',(0.,1.,0.));
#50251=DIRECTION('center_axis',(0.364399348580517,0.,0.931242779705752));
#50252=DIRECTION('ref_axis',(0.931242779705752,0.,-0.364399348580517));
#50253=DIRECTION('',(0.,1.,0.));
#50254=DIRECTION('center_axis',(-0.624280230025758,0.,0.781200482846104));
#50255=DIRECTION('ref_axis',(0.781200482846104,0.,0.624280230025758));
#50256=DIRECTION('',(0.,1.,0.));
#50257=DIRECTION('center_axis',(-0.988679578606275,0.,-0.150042296859647));
#50258=DIRECTION('ref_axis',(-0.150042296859647,0.,0.988679578606275));
#50259=DIRECTION('',(0.,1.,0.));
#50260=DIRECTION('center_axis',(-0.364399348580519,0.,-0.931242779705751));
#50261=DIRECTION('ref_axis',(-0.931242779705751,0.,0.364399348580519));
#50262=DIRECTION('',(0.,1.,0.));
#50263=DIRECTION('center_axis',(0.624280230025758,0.,-0.781200482846105));
#50264=DIRECTION('ref_axis',(-0.781200482846105,0.,-0.624280230025758));
#50265=DIRECTION('center_axis',(0.988679578606276,0.,0.150042296859641));
#50266=DIRECTION('ref_axis',(0.150042296859641,0.,-0.988679578606276));
#50267=DIRECTION('',(0.,1.,0.));
#50268=DIRECTION('',(0.,1.,0.));
#50269=DIRECTION('center_axis',(0.364399348580517,0.,0.931242779705752));
#50270=DIRECTION('ref_axis',(0.931242779705752,0.,-0.364399348580517));
#50271=DIRECTION('',(0.,1.,0.));
#50272=DIRECTION('center_axis',(-0.624280230025758,0.,0.781200482846104));
#50273=DIRECTION('ref_axis',(0.781200482846104,0.,0.624280230025758));
#50274=DIRECTION('',(0.,1.,0.));
#50275=DIRECTION('center_axis',(-0.988679578606275,0.,-0.150042296859647));
#50276=DIRECTION('ref_axis',(-0.150042296859647,0.,0.988679578606275));
#50277=DIRECTION('',(0.,1.,0.));
#50278=DIRECTION('center_axis',(-0.364399348580519,0.,-0.931242779705751));
#50279=DIRECTION('ref_axis',(-0.931242779705751,0.,0.364399348580519));
#50280=DIRECTION('',(0.,1.,0.));
#50281=DIRECTION('center_axis',(0.624280230025758,0.,-0.781200482846105));
#50282=DIRECTION('ref_axis',(-0.781200482846105,0.,-0.624280230025758));
#50283=DIRECTION('center_axis',(0.988679578606276,0.,0.150042296859641));
#50284=DIRECTION('ref_axis',(0.150042296859641,0.,-0.988679578606276));
#50285=DIRECTION('',(0.,1.,0.));
#50286=DIRECTION('',(0.,1.,0.));
#50287=DIRECTION('center_axis',(0.364399348580517,0.,0.931242779705752));
#50288=DIRECTION('ref_axis',(0.931242779705752,0.,-0.364399348580517));
#50289=DIRECTION('',(0.,1.,0.));
#50290=DIRECTION('center_axis',(-0.624280230025758,0.,0.781200482846104));
#50291=DIRECTION('ref_axis',(0.781200482846104,0.,0.624280230025758));
#50292=DIRECTION('',(0.,1.,0.));
#50293=DIRECTION('center_axis',(-0.988679578606275,0.,-0.150042296859647));
#50294=DIRECTION('ref_axis',(-0.150042296859647,0.,0.988679578606275));
#50295=DIRECTION('',(0.,1.,0.));
#50296=DIRECTION('center_axis',(-0.364399348580519,0.,-0.931242779705751));
#50297=DIRECTION('ref_axis',(-0.931242779705751,0.,0.364399348580519));
#50298=DIRECTION('',(0.,1.,0.));
#50299=DIRECTION('center_axis',(0.624280230025758,0.,-0.781200482846105));
#50300=DIRECTION('ref_axis',(-0.781200482846105,0.,-0.624280230025758));
#50301=DIRECTION('center_axis',(0.988679578606276,0.,0.150042296859641));
#50302=DIRECTION('ref_axis',(0.150042296859641,0.,-0.988679578606276));
#50303=DIRECTION('',(0.,1.,0.));
#50304=DIRECTION('',(0.,1.,0.));
#50305=DIRECTION('center_axis',(0.364399348580517,0.,0.931242779705752));
#50306=DIRECTION('ref_axis',(0.931242779705752,0.,-0.364399348580517));
#50307=DIRECTION('',(0.,1.,0.));
#50308=DIRECTION('center_axis',(-0.624280230025758,0.,0.781200482846104));
#50309=DIRECTION('ref_axis',(0.781200482846104,0.,0.624280230025758));
#50310=DIRECTION('',(0.,1.,0.));
#50311=DIRECTION('center_axis',(-0.988679578606275,0.,-0.150042296859647));
#50312=DIRECTION('ref_axis',(-0.150042296859647,0.,0.988679578606275));
#50313=DIRECTION('',(0.,1.,0.));
#50314=DIRECTION('center_axis',(-0.364399348580519,0.,-0.931242779705751));
#50315=DIRECTION('ref_axis',(-0.931242779705751,0.,0.364399348580519));
#50316=DIRECTION('',(0.,1.,0.));
#50317=DIRECTION('center_axis',(0.624280230025758,0.,-0.781200482846105));
#50318=DIRECTION('ref_axis',(-0.781200482846105,0.,-0.624280230025758));
#50319=DIRECTION('center_axis',(0.988679578606276,0.,0.150042296859641));
#50320=DIRECTION('ref_axis',(0.150042296859641,0.,-0.988679578606276));
#50321=DIRECTION('',(0.,1.,0.));
#50322=DIRECTION('',(0.,1.,0.));
#50323=DIRECTION('center_axis',(0.364399348580517,0.,0.931242779705752));
#50324=DIRECTION('ref_axis',(0.931242779705752,0.,-0.364399348580517));
#50325=DIRECTION('',(0.,1.,0.));
#50326=DIRECTION('center_axis',(-0.624280230025758,0.,0.781200482846104));
#50327=DIRECTION('ref_axis',(0.781200482846104,0.,0.624280230025758));
#50328=DIRECTION('',(0.,1.,0.));
#50329=DIRECTION('center_axis',(-0.988679578606275,0.,-0.150042296859647));
#50330=DIRECTION('ref_axis',(-0.150042296859647,0.,0.988679578606275));
#50331=DIRECTION('',(0.,1.,0.));
#50332=DIRECTION('center_axis',(-0.364399348580519,0.,-0.931242779705751));
#50333=DIRECTION('ref_axis',(-0.931242779705751,0.,0.364399348580519));
#50334=DIRECTION('',(0.,1.,0.));
#50335=DIRECTION('center_axis',(0.624280230025758,0.,-0.781200482846105));
#50336=DIRECTION('ref_axis',(-0.781200482846105,0.,-0.624280230025758));
#50337=DIRECTION('center_axis',(0.988679578606276,0.,0.150042296859641));
#50338=DIRECTION('ref_axis',(0.150042296859641,0.,-0.988679578606276));
#50339=DIRECTION('',(0.,1.,0.));
#50340=DIRECTION('',(0.,1.,0.));
#50341=DIRECTION('center_axis',(0.364399348580517,0.,0.931242779705752));
#50342=DIRECTION('ref_axis',(0.931242779705752,0.,-0.364399348580517));
#50343=DIRECTION('',(0.,1.,0.));
#50344=DIRECTION('center_axis',(-0.624280230025758,0.,0.781200482846104));
#50345=DIRECTION('ref_axis',(0.781200482846104,0.,0.624280230025758));
#50346=DIRECTION('',(0.,1.,0.));
#50347=DIRECTION('center_axis',(-0.988679578606275,0.,-0.150042296859647));
#50348=DIRECTION('ref_axis',(-0.150042296859647,0.,0.988679578606275));
#50349=DIRECTION('',(0.,1.,0.));
#50350=DIRECTION('center_axis',(-0.364399348580519,0.,-0.931242779705751));
#50351=DIRECTION('ref_axis',(-0.931242779705751,0.,0.364399348580519));
#50352=DIRECTION('',(0.,1.,0.));
#50353=DIRECTION('center_axis',(0.624280230025758,0.,-0.781200482846105));
#50354=DIRECTION('ref_axis',(-0.781200482846105,0.,-0.624280230025758));
#50355=DIRECTION('center_axis',(0.988679578606276,0.,0.150042296859641));
#50356=DIRECTION('ref_axis',(0.150042296859641,0.,-0.988679578606276));
#50357=DIRECTION('',(0.,1.,0.));
#50358=DIRECTION('',(0.,1.,0.));
#50359=DIRECTION('center_axis',(0.364399348580517,0.,0.931242779705752));
#50360=DIRECTION('ref_axis',(0.931242779705752,0.,-0.364399348580517));
#50361=DIRECTION('',(0.,1.,0.));
#50362=DIRECTION('center_axis',(-0.624280230025758,0.,0.781200482846104));
#50363=DIRECTION('ref_axis',(0.781200482846104,0.,0.624280230025758));
#50364=DIRECTION('',(0.,1.,0.));
#50365=DIRECTION('center_axis',(-0.988679578606275,0.,-0.150042296859647));
#50366=DIRECTION('ref_axis',(-0.150042296859647,0.,0.988679578606275));
#50367=DIRECTION('',(0.,1.,0.));
#50368=DIRECTION('center_axis',(-0.364399348580519,0.,-0.931242779705751));
#50369=DIRECTION('ref_axis',(-0.931242779705751,0.,0.364399348580519));
#50370=DIRECTION('',(0.,1.,0.));
#50371=DIRECTION('center_axis',(0.624280230025758,0.,-0.781200482846105));
#50372=DIRECTION('ref_axis',(-0.781200482846105,0.,-0.624280230025758));
#50373=DIRECTION('center_axis',(0.988679578606276,0.,0.150042296859641));
#50374=DIRECTION('ref_axis',(0.150042296859641,0.,-0.988679578606276));
#50375=DIRECTION('',(0.,1.,0.));
#50376=DIRECTION('',(0.,1.,0.));
#50377=DIRECTION('center_axis',(0.364399348580517,0.,0.931242779705752));
#50378=DIRECTION('ref_axis',(0.931242779705752,0.,-0.364399348580517));
#50379=DIRECTION('',(0.,1.,0.));
#50380=DIRECTION('center_axis',(-0.624280230025758,0.,0.781200482846104));
#50381=DIRECTION('ref_axis',(0.781200482846104,0.,0.624280230025758));
#50382=DIRECTION('',(0.,1.,0.));
#50383=DIRECTION('center_axis',(-0.988679578606275,0.,-0.150042296859647));
#50384=DIRECTION('ref_axis',(-0.150042296859647,0.,0.988679578606275));
#50385=DIRECTION('',(0.,1.,0.));
#50386=DIRECTION('center_axis',(-0.364399348580519,0.,-0.931242779705751));
#50387=DIRECTION('ref_axis',(-0.931242779705751,0.,0.364399348580519));
#50388=DIRECTION('',(0.,1.,0.));
#50389=DIRECTION('center_axis',(0.624280230025758,0.,-0.781200482846105));
#50390=DIRECTION('ref_axis',(-0.781200482846105,0.,-0.624280230025758));
#50391=DIRECTION('center_axis',(0.988679578606276,0.,0.150042296859641));
#50392=DIRECTION('ref_axis',(0.150042296859641,0.,-0.988679578606276));
#50393=DIRECTION('',(0.,1.,0.));
#50394=DIRECTION('',(0.,1.,0.));
#50395=DIRECTION('center_axis',(0.364399348580517,0.,0.931242779705752));
#50396=DIRECTION('ref_axis',(0.931242779705752,0.,-0.364399348580517));
#50397=DIRECTION('',(0.,1.,0.));
#50398=DIRECTION('center_axis',(-0.624280230025758,0.,0.781200482846104));
#50399=DIRECTION('ref_axis',(0.781200482846104,0.,0.624280230025758));
#50400=DIRECTION('',(0.,1.,0.));
#50401=DIRECTION('center_axis',(-0.988679578606275,0.,-0.150042296859647));
#50402=DIRECTION('ref_axis',(-0.150042296859647,0.,0.988679578606275));
#50403=DIRECTION('',(0.,1.,0.));
#50404=DIRECTION('center_axis',(-0.364399348580519,0.,-0.931242779705751));
#50405=DIRECTION('ref_axis',(-0.931242779705751,0.,0.364399348580519));
#50406=DIRECTION('',(0.,1.,0.));
#50407=DIRECTION('center_axis',(0.624280230025758,0.,-0.781200482846105));
#50408=DIRECTION('ref_axis',(-0.781200482846105,0.,-0.624280230025758));
#50409=DIRECTION('center_axis',(0.988679578606276,0.,0.150042296859641));
#50410=DIRECTION('ref_axis',(0.150042296859641,0.,-0.988679578606276));
#50411=DIRECTION('',(0.,1.,0.));
#50412=DIRECTION('',(0.,1.,0.));
#50413=DIRECTION('center_axis',(0.364399348580517,0.,0.931242779705752));
#50414=DIRECTION('ref_axis',(0.931242779705752,0.,-0.364399348580517));
#50415=DIRECTION('',(0.,1.,0.));
#50416=DIRECTION('center_axis',(-0.624280230025758,0.,0.781200482846104));
#50417=DIRECTION('ref_axis',(0.781200482846104,0.,0.624280230025758));
#50418=DIRECTION('',(0.,1.,0.));
#50419=DIRECTION('center_axis',(-0.988679578606275,0.,-0.150042296859647));
#50420=DIRECTION('ref_axis',(-0.150042296859647,0.,0.988679578606275));
#50421=DIRECTION('',(0.,1.,0.));
#50422=DIRECTION('center_axis',(-0.364399348580519,0.,-0.931242779705751));
#50423=DIRECTION('ref_axis',(-0.931242779705751,0.,0.364399348580519));
#50424=DIRECTION('',(0.,1.,0.));
#50425=DIRECTION('center_axis',(0.624280230025758,0.,-0.781200482846105));
#50426=DIRECTION('ref_axis',(-0.781200482846105,0.,-0.624280230025758));
#50427=DIRECTION('center_axis',(0.988679578606276,0.,0.150042296859641));
#50428=DIRECTION('ref_axis',(0.150042296859641,0.,-0.988679578606276));
#50429=DIRECTION('',(0.,1.,0.));
#50430=DIRECTION('',(0.,1.,0.));
#50431=DIRECTION('center_axis',(0.364399348580517,0.,0.931242779705752));
#50432=DIRECTION('ref_axis',(0.931242779705752,0.,-0.364399348580517));
#50433=DIRECTION('',(0.,1.,0.));
#50434=DIRECTION('center_axis',(-0.624280230025758,0.,0.781200482846104));
#50435=DIRECTION('ref_axis',(0.781200482846104,0.,0.624280230025758));
#50436=DIRECTION('',(0.,1.,0.));
#50437=DIRECTION('center_axis',(-0.988679578606275,0.,-0.150042296859647));
#50438=DIRECTION('ref_axis',(-0.150042296859647,0.,0.988679578606275));
#50439=DIRECTION('',(0.,1.,0.));
#50440=DIRECTION('center_axis',(-0.364399348580519,0.,-0.931242779705751));
#50441=DIRECTION('ref_axis',(-0.931242779705751,0.,0.364399348580519));
#50442=DIRECTION('',(0.,1.,0.));
#50443=DIRECTION('center_axis',(0.624280230025758,0.,-0.781200482846105));
#50444=DIRECTION('ref_axis',(-0.781200482846105,0.,-0.624280230025758));
#50445=DIRECTION('center_axis',(0.988679578606276,0.,0.150042296859641));
#50446=DIRECTION('ref_axis',(0.150042296859641,0.,-0.988679578606276));
#50447=DIRECTION('',(0.,1.,0.));
#50448=DIRECTION('',(0.,1.,0.));
#50449=DIRECTION('center_axis',(0.364399348580517,0.,0.931242779705752));
#50450=DIRECTION('ref_axis',(0.931242779705752,0.,-0.364399348580517));
#50451=DIRECTION('',(0.,1.,0.));
#50452=DIRECTION('center_axis',(-0.624280230025758,0.,0.781200482846104));
#50453=DIRECTION('ref_axis',(0.781200482846104,0.,0.624280230025758));
#50454=DIRECTION('',(0.,1.,0.));
#50455=DIRECTION('center_axis',(-0.988679578606275,0.,-0.150042296859647));
#50456=DIRECTION('ref_axis',(-0.150042296859647,0.,0.988679578606275));
#50457=DIRECTION('',(0.,1.,0.));
#50458=DIRECTION('center_axis',(-0.364399348580519,0.,-0.931242779705751));
#50459=DIRECTION('ref_axis',(-0.931242779705751,0.,0.364399348580519));
#50460=DIRECTION('',(0.,1.,0.));
#50461=DIRECTION('center_axis',(0.624280230025758,0.,-0.781200482846105));
#50462=DIRECTION('ref_axis',(-0.781200482846105,0.,-0.624280230025758));
#50463=DIRECTION('center_axis',(0.988679578606276,0.,0.150042296859641));
#50464=DIRECTION('ref_axis',(0.150042296859641,0.,-0.988679578606276));
#50465=DIRECTION('',(0.,1.,0.));
#50466=DIRECTION('',(0.,1.,0.));
#50467=DIRECTION('center_axis',(0.364399348580517,0.,0.931242779705752));
#50468=DIRECTION('ref_axis',(0.931242779705752,0.,-0.364399348580517));
#50469=DIRECTION('',(0.,1.,0.));
#50470=DIRECTION('center_axis',(-0.624280230025758,0.,0.781200482846104));
#50471=DIRECTION('ref_axis',(0.781200482846104,0.,0.624280230025758));
#50472=DIRECTION('',(0.,1.,0.));
#50473=DIRECTION('center_axis',(-0.988679578606275,0.,-0.150042296859647));
#50474=DIRECTION('ref_axis',(-0.150042296859647,0.,0.988679578606275));
#50475=DIRECTION('',(0.,1.,0.));
#50476=DIRECTION('center_axis',(-0.364399348580519,0.,-0.931242779705751));
#50477=DIRECTION('ref_axis',(-0.931242779705751,0.,0.364399348580519));
#50478=DIRECTION('',(0.,1.,0.));
#50479=DIRECTION('center_axis',(0.624280230025758,0.,-0.781200482846105));
#50480=DIRECTION('ref_axis',(-0.781200482846105,0.,-0.624280230025758));
#50481=DIRECTION('center_axis',(0.988679578606276,0.,0.150042296859641));
#50482=DIRECTION('ref_axis',(0.150042296859641,0.,-0.988679578606276));
#50483=DIRECTION('',(0.,1.,0.));
#50484=DIRECTION('',(0.,1.,0.));
#50485=DIRECTION('center_axis',(0.364399348580517,0.,0.931242779705752));
#50486=DIRECTION('ref_axis',(0.931242779705752,0.,-0.364399348580517));
#50487=DIRECTION('',(0.,1.,0.));
#50488=DIRECTION('center_axis',(-0.624280230025758,0.,0.781200482846104));
#50489=DIRECTION('ref_axis',(0.781200482846104,0.,0.624280230025758));
#50490=DIRECTION('',(0.,1.,0.));
#50491=DIRECTION('center_axis',(-0.988679578606275,0.,-0.150042296859647));
#50492=DIRECTION('ref_axis',(-0.150042296859647,0.,0.988679578606275));
#50493=DIRECTION('',(0.,1.,0.));
#50494=DIRECTION('center_axis',(-0.364399348580519,0.,-0.931242779705751));
#50495=DIRECTION('ref_axis',(-0.931242779705751,0.,0.364399348580519));
#50496=DIRECTION('',(0.,1.,0.));
#50497=DIRECTION('center_axis',(0.624280230025758,0.,-0.781200482846105));
#50498=DIRECTION('ref_axis',(-0.781200482846105,0.,-0.624280230025758));
#50499=DIRECTION('center_axis',(0.988679578606276,0.,0.150042296859641));
#50500=DIRECTION('ref_axis',(0.150042296859641,0.,-0.988679578606276));
#50501=DIRECTION('',(0.,1.,0.));
#50502=DIRECTION('',(0.,1.,0.));
#50503=DIRECTION('center_axis',(0.364399348580517,0.,0.931242779705752));
#50504=DIRECTION('ref_axis',(0.931242779705752,0.,-0.364399348580517));
#50505=DIRECTION('',(0.,1.,0.));
#50506=DIRECTION('center_axis',(-0.624280230025758,0.,0.781200482846104));
#50507=DIRECTION('ref_axis',(0.781200482846104,0.,0.624280230025758));
#50508=DIRECTION('',(0.,1.,0.));
#50509=DIRECTION('center_axis',(-0.988679578606275,0.,-0.150042296859647));
#50510=DIRECTION('ref_axis',(-0.150042296859647,0.,0.988679578606275));
#50511=DIRECTION('',(0.,1.,0.));
#50512=DIRECTION('center_axis',(-0.364399348580519,0.,-0.931242779705751));
#50513=DIRECTION('ref_axis',(-0.931242779705751,0.,0.364399348580519));
#50514=DIRECTION('',(0.,1.,0.));
#50515=DIRECTION('center_axis',(0.624280230025758,0.,-0.781200482846105));
#50516=DIRECTION('ref_axis',(-0.781200482846105,0.,-0.624280230025758));
#50517=DIRECTION('center_axis',(0.988679578606276,0.,0.150042296859641));
#50518=DIRECTION('ref_axis',(0.150042296859641,0.,-0.988679578606276));
#50519=DIRECTION('',(0.,1.,0.));
#50520=DIRECTION('',(0.,1.,0.));
#50521=DIRECTION('center_axis',(0.364399348580517,0.,0.931242779705752));
#50522=DIRECTION('ref_axis',(0.931242779705752,0.,-0.364399348580517));
#50523=DIRECTION('',(0.,1.,0.));
#50524=DIRECTION('center_axis',(-0.624280230025758,0.,0.781200482846104));
#50525=DIRECTION('ref_axis',(0.781200482846104,0.,0.624280230025758));
#50526=DIRECTION('',(0.,1.,0.));
#50527=DIRECTION('center_axis',(-0.988679578606275,0.,-0.150042296859647));
#50528=DIRECTION('ref_axis',(-0.150042296859647,0.,0.988679578606275));
#50529=DIRECTION('',(0.,1.,0.));
#50530=DIRECTION('center_axis',(-0.364399348580519,0.,-0.931242779705751));
#50531=DIRECTION('ref_axis',(-0.931242779705751,0.,0.364399348580519));
#50532=DIRECTION('',(0.,1.,0.));
#50533=DIRECTION('center_axis',(0.624280230025758,0.,-0.781200482846105));
#50534=DIRECTION('ref_axis',(-0.781200482846105,0.,-0.624280230025758));
#50535=DIRECTION('center_axis',(0.988679578606276,0.,0.150042296859641));
#50536=DIRECTION('ref_axis',(0.150042296859641,0.,-0.988679578606276));
#50537=DIRECTION('',(0.,1.,0.));
#50538=DIRECTION('',(0.,1.,0.));
#50539=DIRECTION('center_axis',(0.364399348580517,0.,0.931242779705752));
#50540=DIRECTION('ref_axis',(0.931242779705752,0.,-0.364399348580517));
#50541=DIRECTION('',(0.,1.,0.));
#50542=DIRECTION('center_axis',(-0.624280230025758,0.,0.781200482846104));
#50543=DIRECTION('ref_axis',(0.781200482846104,0.,0.624280230025758));
#50544=DIRECTION('',(0.,1.,0.));
#50545=DIRECTION('center_axis',(-0.988679578606275,0.,-0.150042296859647));
#50546=DIRECTION('ref_axis',(-0.150042296859647,0.,0.988679578606275));
#50547=DIRECTION('',(0.,1.,0.));
#50548=DIRECTION('center_axis',(-0.364399348580519,0.,-0.931242779705751));
#50549=DIRECTION('ref_axis',(-0.931242779705751,0.,0.364399348580519));
#50550=DIRECTION('',(0.,1.,0.));
#50551=DIRECTION('center_axis',(0.624280230025758,0.,-0.781200482846105));
#50552=DIRECTION('ref_axis',(-0.781200482846105,0.,-0.624280230025758));
#50553=DIRECTION('center_axis',(0.988679578606276,0.,0.150042296859641));
#50554=DIRECTION('ref_axis',(0.150042296859641,0.,-0.988679578606276));
#50555=DIRECTION('',(0.,1.,0.));
#50556=DIRECTION('',(0.,1.,0.));
#50557=DIRECTION('center_axis',(0.364399348580517,0.,0.931242779705752));
#50558=DIRECTION('ref_axis',(0.931242779705752,0.,-0.364399348580517));
#50559=DIRECTION('',(0.,1.,0.));
#50560=DIRECTION('center_axis',(-0.624280230025758,0.,0.781200482846104));
#50561=DIRECTION('ref_axis',(0.781200482846104,0.,0.624280230025758));
#50562=DIRECTION('',(0.,1.,0.));
#50563=DIRECTION('center_axis',(-0.988679578606275,0.,-0.150042296859647));
#50564=DIRECTION('ref_axis',(-0.150042296859647,0.,0.988679578606275));
#50565=DIRECTION('',(0.,1.,0.));
#50566=DIRECTION('center_axis',(-0.364399348580519,0.,-0.931242779705751));
#50567=DIRECTION('ref_axis',(-0.931242779705751,0.,0.364399348580519));
#50568=DIRECTION('',(0.,1.,0.));
#50569=DIRECTION('center_axis',(0.624280230025758,0.,-0.781200482846105));
#50570=DIRECTION('ref_axis',(-0.781200482846105,0.,-0.624280230025758));
#50571=DIRECTION('center_axis',(0.988679578606276,0.,0.150042296859641));
#50572=DIRECTION('ref_axis',(0.150042296859641,0.,-0.988679578606276));
#50573=DIRECTION('',(0.,1.,0.));
#50574=DIRECTION('',(0.,1.,0.));
#50575=DIRECTION('center_axis',(0.364399348580517,0.,0.931242779705752));
#50576=DIRECTION('ref_axis',(0.931242779705752,0.,-0.364399348580517));
#50577=DIRECTION('',(0.,1.,0.));
#50578=DIRECTION('center_axis',(-0.624280230025758,0.,0.781200482846104));
#50579=DIRECTION('ref_axis',(0.781200482846104,0.,0.624280230025758));
#50580=DIRECTION('',(0.,1.,0.));
#50581=DIRECTION('center_axis',(-0.988679578606275,0.,-0.150042296859647));
#50582=DIRECTION('ref_axis',(-0.150042296859647,0.,0.988679578606275));
#50583=DIRECTION('',(0.,1.,0.));
#50584=DIRECTION('center_axis',(-0.364399348580519,0.,-0.931242779705751));
#50585=DIRECTION('ref_axis',(-0.931242779705751,0.,0.364399348580519));
#50586=DIRECTION('',(0.,1.,0.));
#50587=DIRECTION('center_axis',(0.624280230025758,0.,-0.781200482846105));
#50588=DIRECTION('ref_axis',(-0.781200482846105,0.,-0.624280230025758));
#50589=DIRECTION('center_axis',(0.988679578606276,0.,0.150042296859641));
#50590=DIRECTION('ref_axis',(0.150042296859641,0.,-0.988679578606276));
#50591=DIRECTION('',(0.,1.,0.));
#50592=DIRECTION('',(0.,1.,0.));
#50593=DIRECTION('center_axis',(0.364399348580517,0.,0.931242779705752));
#50594=DIRECTION('ref_axis',(0.931242779705752,0.,-0.364399348580517));
#50595=DIRECTION('',(0.,1.,0.));
#50596=DIRECTION('center_axis',(-0.624280230025758,0.,0.781200482846104));
#50597=DIRECTION('ref_axis',(0.781200482846104,0.,0.624280230025758));
#50598=DIRECTION('',(0.,1.,0.));
#50599=DIRECTION('center_axis',(-0.988679578606275,0.,-0.150042296859647));
#50600=DIRECTION('ref_axis',(-0.150042296859647,0.,0.988679578606275));
#50601=DIRECTION('',(0.,1.,0.));
#50602=DIRECTION('center_axis',(-0.364399348580519,0.,-0.931242779705751));
#50603=DIRECTION('ref_axis',(-0.931242779705751,0.,0.364399348580519));
#50604=DIRECTION('',(0.,1.,0.));
#50605=DIRECTION('center_axis',(0.624280230025758,0.,-0.781200482846105));
#50606=DIRECTION('ref_axis',(-0.781200482846105,0.,-0.624280230025758));
#50607=DIRECTION('center_axis',(0.988679578606276,0.,0.150042296859641));
#50608=DIRECTION('ref_axis',(0.150042296859641,0.,-0.988679578606276));
#50609=DIRECTION('',(0.,1.,0.));
#50610=DIRECTION('',(0.,1.,0.));
#50611=DIRECTION('center_axis',(0.364399348580517,0.,0.931242779705752));
#50612=DIRECTION('ref_axis',(0.931242779705752,0.,-0.364399348580517));
#50613=DIRECTION('',(0.,1.,0.));
#50614=DIRECTION('center_axis',(-0.624280230025758,0.,0.781200482846104));
#50615=DIRECTION('ref_axis',(0.781200482846104,0.,0.624280230025758));
#50616=DIRECTION('',(0.,1.,0.));
#50617=DIRECTION('center_axis',(-0.988679578606275,0.,-0.150042296859647));
#50618=DIRECTION('ref_axis',(-0.150042296859647,0.,0.988679578606275));
#50619=DIRECTION('',(0.,1.,0.));
#50620=DIRECTION('center_axis',(-0.364399348580519,0.,-0.931242779705751));
#50621=DIRECTION('ref_axis',(-0.931242779705751,0.,0.364399348580519));
#50622=DIRECTION('',(0.,1.,0.));
#50623=DIRECTION('center_axis',(0.624280230025758,0.,-0.781200482846105));
#50624=DIRECTION('ref_axis',(-0.781200482846105,0.,-0.624280230025758));
#50625=DIRECTION('center_axis',(0.988679578606276,0.,0.150042296859641));
#50626=DIRECTION('ref_axis',(0.150042296859641,0.,-0.988679578606276));
#50627=DIRECTION('',(0.,1.,0.));
#50628=DIRECTION('',(0.,1.,0.));
#50629=DIRECTION('center_axis',(0.364399348580517,0.,0.931242779705752));
#50630=DIRECTION('ref_axis',(0.931242779705752,0.,-0.364399348580517));
#50631=DIRECTION('',(0.,1.,0.));
#50632=DIRECTION('center_axis',(-0.624280230025758,0.,0.781200482846104));
#50633=DIRECTION('ref_axis',(0.781200482846104,0.,0.624280230025758));
#50634=DIRECTION('',(0.,1.,0.));
#50635=DIRECTION('center_axis',(-0.988679578606275,0.,-0.150042296859647));
#50636=DIRECTION('ref_axis',(-0.150042296859647,0.,0.988679578606275));
#50637=DIRECTION('',(0.,1.,0.));
#50638=DIRECTION('center_axis',(-0.364399348580519,0.,-0.931242779705751));
#50639=DIRECTION('ref_axis',(-0.931242779705751,0.,0.364399348580519));
#50640=DIRECTION('',(0.,1.,0.));
#50641=DIRECTION('center_axis',(0.624280230025758,0.,-0.781200482846105));
#50642=DIRECTION('ref_axis',(-0.781200482846105,0.,-0.624280230025758));
#50643=DIRECTION('center_axis',(0.988679578606276,0.,0.150042296859641));
#50644=DIRECTION('ref_axis',(0.150042296859641,0.,-0.988679578606276));
#50645=DIRECTION('',(0.,1.,0.));
#50646=DIRECTION('',(0.,1.,0.));
#50647=DIRECTION('center_axis',(0.364399348580517,0.,0.931242779705752));
#50648=DIRECTION('ref_axis',(0.931242779705752,0.,-0.364399348580517));
#50649=DIRECTION('',(0.,1.,0.));
#50650=DIRECTION('center_axis',(-0.624280230025758,0.,0.781200482846104));
#50651=DIRECTION('ref_axis',(0.781200482846104,0.,0.624280230025758));
#50652=DIRECTION('',(0.,1.,0.));
#50653=DIRECTION('center_axis',(-0.988679578606275,0.,-0.150042296859647));
#50654=DIRECTION('ref_axis',(-0.150042296859647,0.,0.988679578606275));
#50655=DIRECTION('',(0.,1.,0.));
#50656=DIRECTION('center_axis',(-0.364399348580519,0.,-0.931242779705751));
#50657=DIRECTION('ref_axis',(-0.931242779705751,0.,0.364399348580519));
#50658=DIRECTION('',(0.,1.,0.));
#50659=DIRECTION('center_axis',(0.624280230025758,0.,-0.781200482846105));
#50660=DIRECTION('ref_axis',(-0.781200482846105,0.,-0.624280230025758));
#50661=DIRECTION('center_axis',(0.988679578606276,0.,0.150042296859641));
#50662=DIRECTION('ref_axis',(0.150042296859641,0.,-0.988679578606276));
#50663=DIRECTION('',(0.,1.,0.));
#50664=DIRECTION('',(0.,1.,0.));
#50665=DIRECTION('center_axis',(0.364399348580517,0.,0.931242779705752));
#50666=DIRECTION('ref_axis',(0.931242779705752,0.,-0.364399348580517));
#50667=DIRECTION('',(0.,1.,0.));
#50668=DIRECTION('center_axis',(-0.624280230025758,0.,0.781200482846104));
#50669=DIRECTION('ref_axis',(0.781200482846104,0.,0.624280230025758));
#50670=DIRECTION('',(0.,1.,0.));
#50671=DIRECTION('center_axis',(-0.988679578606275,0.,-0.150042296859647));
#50672=DIRECTION('ref_axis',(-0.150042296859647,0.,0.988679578606275));
#50673=DIRECTION('',(0.,1.,0.));
#50674=DIRECTION('center_axis',(-0.364399348580519,0.,-0.931242779705751));
#50675=DIRECTION('ref_axis',(-0.931242779705751,0.,0.364399348580519));
#50676=DIRECTION('',(0.,1.,0.));
#50677=DIRECTION('center_axis',(0.624280230025758,0.,-0.781200482846105));
#50678=DIRECTION('ref_axis',(-0.781200482846105,0.,-0.624280230025758));
#50679=DIRECTION('center_axis',(0.988679578606276,0.,0.150042296859641));
#50680=DIRECTION('ref_axis',(0.150042296859641,0.,-0.988679578606276));
#50681=DIRECTION('',(0.,1.,0.));
#50682=DIRECTION('',(0.,1.,0.));
#50683=DIRECTION('center_axis',(0.364399348580517,0.,0.931242779705752));
#50684=DIRECTION('ref_axis',(0.931242779705752,0.,-0.364399348580517));
#50685=DIRECTION('',(0.,1.,0.));
#50686=DIRECTION('center_axis',(-0.624280230025758,0.,0.781200482846104));
#50687=DIRECTION('ref_axis',(0.781200482846104,0.,0.624280230025758));
#50688=DIRECTION('',(0.,1.,0.));
#50689=DIRECTION('center_axis',(-0.988679578606275,0.,-0.150042296859647));
#50690=DIRECTION('ref_axis',(-0.150042296859647,0.,0.988679578606275));
#50691=DIRECTION('',(0.,1.,0.));
#50692=DIRECTION('center_axis',(-0.364399348580519,0.,-0.931242779705751));
#50693=DIRECTION('ref_axis',(-0.931242779705751,0.,0.364399348580519));
#50694=DIRECTION('',(0.,1.,0.));
#50695=DIRECTION('center_axis',(0.624280230025758,0.,-0.781200482846105));
#50696=DIRECTION('ref_axis',(-0.781200482846105,0.,-0.624280230025758));
#50697=DIRECTION('center_axis',(0.988679578606276,0.,0.150042296859641));
#50698=DIRECTION('ref_axis',(0.150042296859641,0.,-0.988679578606276));
#50699=DIRECTION('',(0.,1.,0.));
#50700=DIRECTION('',(0.,1.,0.));
#50701=DIRECTION('center_axis',(0.364399348580517,0.,0.931242779705752));
#50702=DIRECTION('ref_axis',(0.931242779705752,0.,-0.364399348580517));
#50703=DIRECTION('',(0.,1.,0.));
#50704=DIRECTION('center_axis',(-0.624280230025758,0.,0.781200482846104));
#50705=DIRECTION('ref_axis',(0.781200482846104,0.,0.624280230025758));
#50706=DIRECTION('',(0.,1.,0.));
#50707=DIRECTION('center_axis',(-0.988679578606275,0.,-0.150042296859647));
#50708=DIRECTION('ref_axis',(-0.150042296859647,0.,0.988679578606275));
#50709=DIRECTION('',(0.,1.,0.));
#50710=DIRECTION('center_axis',(-0.364399348580519,0.,-0.931242779705751));
#50711=DIRECTION('ref_axis',(-0.931242779705751,0.,0.364399348580519));
#50712=DIRECTION('',(0.,1.,0.));
#50713=DIRECTION('center_axis',(0.624280230025758,0.,-0.781200482846105));
#50714=DIRECTION('ref_axis',(-0.781200482846105,0.,-0.624280230025758));
#50715=DIRECTION('center_axis',(0.988679578606276,0.,0.150042296859641));
#50716=DIRECTION('ref_axis',(0.150042296859641,0.,-0.988679578606276));
#50717=DIRECTION('',(0.,1.,0.));
#50718=DIRECTION('',(0.,1.,0.));
#50719=DIRECTION('center_axis',(0.364399348580517,0.,0.931242779705752));
#50720=DIRECTION('ref_axis',(0.931242779705752,0.,-0.364399348580517));
#50721=DIRECTION('',(0.,1.,0.));
#50722=DIRECTION('center_axis',(-0.624280230025758,0.,0.781200482846104));
#50723=DIRECTION('ref_axis',(0.781200482846104,0.,0.624280230025758));
#50724=DIRECTION('',(0.,1.,0.));
#50725=DIRECTION('center_axis',(-0.988679578606275,0.,-0.150042296859647));
#50726=DIRECTION('ref_axis',(-0.150042296859647,0.,0.988679578606275));
#50727=DIRECTION('',(0.,1.,0.));
#50728=DIRECTION('center_axis',(-0.364399348580519,0.,-0.931242779705751));
#50729=DIRECTION('ref_axis',(-0.931242779705751,0.,0.364399348580519));
#50730=DIRECTION('',(0.,1.,0.));
#50731=DIRECTION('center_axis',(0.624280230025758,0.,-0.781200482846105));
#50732=DIRECTION('ref_axis',(-0.781200482846105,0.,-0.624280230025758));
#50733=DIRECTION('center_axis',(0.988679578606276,0.,0.150042296859641));
#50734=DIRECTION('ref_axis',(0.150042296859641,0.,-0.988679578606276));
#50735=DIRECTION('',(0.,1.,0.));
#50736=DIRECTION('',(0.,1.,0.));
#50737=DIRECTION('center_axis',(0.364399348580517,0.,0.931242779705752));
#50738=DIRECTION('ref_axis',(0.931242779705752,0.,-0.364399348580517));
#50739=DIRECTION('',(0.,1.,0.));
#50740=DIRECTION('center_axis',(-0.624280230025758,0.,0.781200482846104));
#50741=DIRECTION('ref_axis',(0.781200482846104,0.,0.624280230025758));
#50742=DIRECTION('',(0.,1.,0.));
#50743=DIRECTION('center_axis',(-0.988679578606275,0.,-0.150042296859647));
#50744=DIRECTION('ref_axis',(-0.150042296859647,0.,0.988679578606275));
#50745=DIRECTION('',(0.,1.,0.));
#50746=DIRECTION('center_axis',(-0.364399348580519,0.,-0.931242779705751));
#50747=DIRECTION('ref_axis',(-0.931242779705751,0.,0.364399348580519));
#50748=DIRECTION('',(0.,1.,0.));
#50749=DIRECTION('center_axis',(0.624280230025758,0.,-0.781200482846105));
#50750=DIRECTION('ref_axis',(-0.781200482846105,0.,-0.624280230025758));
#50751=DIRECTION('center_axis',(0.988679578606276,0.,0.150042296859641));
#50752=DIRECTION('ref_axis',(0.150042296859641,0.,-0.988679578606276));
#50753=DIRECTION('',(0.,1.,0.));
#50754=DIRECTION('',(0.,1.,0.));
#50755=DIRECTION('center_axis',(0.364399348580517,0.,0.931242779705752));
#50756=DIRECTION('ref_axis',(0.931242779705752,0.,-0.364399348580517));
#50757=DIRECTION('',(0.,1.,0.));
#50758=DIRECTION('center_axis',(-0.624280230025758,0.,0.781200482846104));
#50759=DIRECTION('ref_axis',(0.781200482846104,0.,0.624280230025758));
#50760=DIRECTION('',(0.,1.,0.));
#50761=DIRECTION('center_axis',(-0.988679578606275,0.,-0.150042296859647));
#50762=DIRECTION('ref_axis',(-0.150042296859647,0.,0.988679578606275));
#50763=DIRECTION('',(0.,1.,0.));
#50764=DIRECTION('center_axis',(-0.364399348580519,0.,-0.931242779705751));
#50765=DIRECTION('ref_axis',(-0.931242779705751,0.,0.364399348580519));
#50766=DIRECTION('',(0.,1.,0.));
#50767=DIRECTION('center_axis',(0.624280230025758,0.,-0.781200482846105));
#50768=DIRECTION('ref_axis',(-0.781200482846105,0.,-0.624280230025758));
#50769=DIRECTION('center_axis',(0.988679578606276,0.,0.150042296859641));
#50770=DIRECTION('ref_axis',(0.150042296859641,0.,-0.988679578606276));
#50771=DIRECTION('',(0.,1.,0.));
#50772=DIRECTION('',(0.,1.,0.));
#50773=DIRECTION('center_axis',(0.364399348580517,0.,0.931242779705752));
#50774=DIRECTION('ref_axis',(0.931242779705752,0.,-0.364399348580517));
#50775=DIRECTION('',(0.,1.,0.));
#50776=DIRECTION('center_axis',(-0.624280230025758,0.,0.781200482846104));
#50777=DIRECTION('ref_axis',(0.781200482846104,0.,0.624280230025758));
#50778=DIRECTION('',(0.,1.,0.));
#50779=DIRECTION('center_axis',(-0.988679578606275,0.,-0.150042296859647));
#50780=DIRECTION('ref_axis',(-0.150042296859647,0.,0.988679578606275));
#50781=DIRECTION('',(0.,1.,0.));
#50782=DIRECTION('center_axis',(-0.364399348580519,0.,-0.931242779705751));
#50783=DIRECTION('ref_axis',(-0.931242779705751,0.,0.364399348580519));
#50784=DIRECTION('',(0.,1.,0.));
#50785=DIRECTION('center_axis',(0.624280230025758,0.,-0.781200482846105));
#50786=DIRECTION('ref_axis',(-0.781200482846105,0.,-0.624280230025758));
#50787=DIRECTION('center_axis',(0.988679578606276,0.,0.150042296859641));
#50788=DIRECTION('ref_axis',(0.150042296859641,0.,-0.988679578606276));
#50789=DIRECTION('',(0.,1.,0.));
#50790=DIRECTION('',(0.,1.,0.));
#50791=DIRECTION('center_axis',(0.364399348580517,0.,0.931242779705752));
#50792=DIRECTION('ref_axis',(0.931242779705752,0.,-0.364399348580517));
#50793=DIRECTION('',(0.,1.,0.));
#50794=DIRECTION('center_axis',(-0.624280230025758,0.,0.781200482846104));
#50795=DIRECTION('ref_axis',(0.781200482846104,0.,0.624280230025758));
#50796=DIRECTION('',(0.,1.,0.));
#50797=DIRECTION('center_axis',(-0.988679578606275,0.,-0.150042296859647));
#50798=DIRECTION('ref_axis',(-0.150042296859647,0.,0.988679578606275));
#50799=DIRECTION('',(0.,1.,0.));
#50800=DIRECTION('center_axis',(-0.364399348580519,0.,-0.931242779705751));
#50801=DIRECTION('ref_axis',(-0.931242779705751,0.,0.364399348580519));
#50802=DIRECTION('',(0.,1.,0.));
#50803=DIRECTION('center_axis',(0.624280230025758,0.,-0.781200482846105));
#50804=DIRECTION('ref_axis',(-0.781200482846105,0.,-0.624280230025758));
#50805=DIRECTION('center_axis',(0.988679578606276,0.,0.150042296859641));
#50806=DIRECTION('ref_axis',(0.150042296859641,0.,-0.988679578606276));
#50807=DIRECTION('',(0.,1.,0.));
#50808=DIRECTION('',(0.,1.,0.));
#50809=DIRECTION('center_axis',(0.364399348580517,0.,0.931242779705752));
#50810=DIRECTION('ref_axis',(0.931242779705752,0.,-0.364399348580517));
#50811=DIRECTION('',(0.,1.,0.));
#50812=DIRECTION('center_axis',(-0.624280230025758,0.,0.781200482846104));
#50813=DIRECTION('ref_axis',(0.781200482846104,0.,0.624280230025758));
#50814=DIRECTION('',(0.,1.,0.));
#50815=DIRECTION('center_axis',(-0.988679578606275,0.,-0.150042296859647));
#50816=DIRECTION('ref_axis',(-0.150042296859647,0.,0.988679578606275));
#50817=DIRECTION('',(0.,1.,0.));
#50818=DIRECTION('center_axis',(-0.364399348580519,0.,-0.931242779705751));
#50819=DIRECTION('ref_axis',(-0.931242779705751,0.,0.364399348580519));
#50820=DIRECTION('',(0.,1.,0.));
#50821=DIRECTION('center_axis',(0.624280230025758,0.,-0.781200482846105));
#50822=DIRECTION('ref_axis',(-0.781200482846105,0.,-0.624280230025758));
#50823=DIRECTION('center_axis',(0.988679578606276,0.,0.150042296859641));
#50824=DIRECTION('ref_axis',(0.150042296859641,0.,-0.988679578606276));
#50825=DIRECTION('',(0.,1.,0.));
#50826=DIRECTION('',(0.,1.,0.));
#50827=DIRECTION('center_axis',(0.364399348580517,0.,0.931242779705752));
#50828=DIRECTION('ref_axis',(0.931242779705752,0.,-0.364399348580517));
#50829=DIRECTION('',(0.,1.,0.));
#50830=DIRECTION('center_axis',(-0.624280230025758,0.,0.781200482846104));
#50831=DIRECTION('ref_axis',(0.781200482846104,0.,0.624280230025758));
#50832=DIRECTION('',(0.,1.,0.));
#50833=DIRECTION('center_axis',(-0.988679578606275,0.,-0.150042296859647));
#50834=DIRECTION('ref_axis',(-0.150042296859647,0.,0.988679578606275));
#50835=DIRECTION('',(0.,1.,0.));
#50836=DIRECTION('center_axis',(-0.364399348580519,0.,-0.931242779705751));
#50837=DIRECTION('ref_axis',(-0.931242779705751,0.,0.364399348580519));
#50838=DIRECTION('',(0.,1.,0.));
#50839=DIRECTION('center_axis',(0.624280230025758,0.,-0.781200482846105));
#50840=DIRECTION('ref_axis',(-0.781200482846105,0.,-0.624280230025758));
#50841=DIRECTION('center_axis',(0.988679578606276,0.,0.150042296859641));
#50842=DIRECTION('ref_axis',(0.150042296859641,0.,-0.988679578606276));
#50843=DIRECTION('',(0.,1.,0.));
#50844=DIRECTION('',(0.,1.,0.));
#50845=DIRECTION('center_axis',(0.364399348580517,0.,0.931242779705752));
#50846=DIRECTION('ref_axis',(0.931242779705752,0.,-0.364399348580517));
#50847=DIRECTION('',(0.,1.,0.));
#50848=DIRECTION('center_axis',(-0.624280230025758,0.,0.781200482846104));
#50849=DIRECTION('ref_axis',(0.781200482846104,0.,0.624280230025758));
#50850=DIRECTION('',(0.,1.,0.));
#50851=DIRECTION('center_axis',(-0.988679578606275,0.,-0.150042296859647));
#50852=DIRECTION('ref_axis',(-0.150042296859647,0.,0.988679578606275));
#50853=DIRECTION('',(0.,1.,0.));
#50854=DIRECTION('center_axis',(-0.364399348580519,0.,-0.931242779705751));
#50855=DIRECTION('ref_axis',(-0.931242779705751,0.,0.364399348580519));
#50856=DIRECTION('',(0.,1.,0.));
#50857=DIRECTION('center_axis',(0.624280230025758,0.,-0.781200482846105));
#50858=DIRECTION('ref_axis',(-0.781200482846105,0.,-0.624280230025758));
#50859=DIRECTION('center_axis',(0.988679578606276,0.,0.150042296859641));
#50860=DIRECTION('ref_axis',(0.150042296859641,0.,-0.988679578606276));
#50861=DIRECTION('',(0.,1.,0.));
#50862=DIRECTION('',(0.,1.,0.));
#50863=DIRECTION('center_axis',(0.364399348580517,0.,0.931242779705752));
#50864=DIRECTION('ref_axis',(0.931242779705752,0.,-0.364399348580517));
#50865=DIRECTION('',(0.,1.,0.));
#50866=DIRECTION('center_axis',(-0.624280230025758,0.,0.781200482846104));
#50867=DIRECTION('ref_axis',(0.781200482846104,0.,0.624280230025758));
#50868=DIRECTION('',(0.,1.,0.));
#50869=DIRECTION('center_axis',(-0.988679578606275,0.,-0.150042296859647));
#50870=DIRECTION('ref_axis',(-0.150042296859647,0.,0.988679578606275));
#50871=DIRECTION('',(0.,1.,0.));
#50872=DIRECTION('center_axis',(-0.364399348580519,0.,-0.931242779705751));
#50873=DIRECTION('ref_axis',(-0.931242779705751,0.,0.364399348580519));
#50874=DIRECTION('',(0.,1.,0.));
#50875=DIRECTION('center_axis',(0.624280230025758,0.,-0.781200482846105));
#50876=DIRECTION('ref_axis',(-0.781200482846105,0.,-0.624280230025758));
#50877=DIRECTION('center_axis',(0.988679578606276,0.,0.150042296859641));
#50878=DIRECTION('ref_axis',(0.150042296859641,0.,-0.988679578606276));
#50879=DIRECTION('',(0.,1.,0.));
#50880=DIRECTION('',(0.,1.,0.));
#50881=DIRECTION('center_axis',(0.364399348580517,0.,0.931242779705752));
#50882=DIRECTION('ref_axis',(0.931242779705752,0.,-0.364399348580517));
#50883=DIRECTION('',(0.,1.,0.));
#50884=DIRECTION('center_axis',(-0.624280230025758,0.,0.781200482846104));
#50885=DIRECTION('ref_axis',(0.781200482846104,0.,0.624280230025758));
#50886=DIRECTION('',(0.,1.,0.));
#50887=DIRECTION('center_axis',(-0.988679578606275,0.,-0.150042296859647));
#50888=DIRECTION('ref_axis',(-0.150042296859647,0.,0.988679578606275));
#50889=DIRECTION('',(0.,1.,0.));
#50890=DIRECTION('center_axis',(-0.364399348580519,0.,-0.931242779705751));
#50891=DIRECTION('ref_axis',(-0.931242779705751,0.,0.364399348580519));
#50892=DIRECTION('',(0.,1.,0.));
#50893=DIRECTION('center_axis',(0.624280230025758,0.,-0.781200482846105));
#50894=DIRECTION('ref_axis',(-0.781200482846105,0.,-0.624280230025758));
#50895=DIRECTION('center_axis',(0.988679578606276,0.,0.150042296859641));
#50896=DIRECTION('ref_axis',(0.150042296859641,0.,-0.988679578606276));
#50897=DIRECTION('',(0.,1.,0.));
#50898=DIRECTION('',(0.,1.,0.));
#50899=DIRECTION('center_axis',(0.364399348580517,0.,0.931242779705752));
#50900=DIRECTION('ref_axis',(0.931242779705752,0.,-0.364399348580517));
#50901=DIRECTION('',(0.,1.,0.));
#50902=DIRECTION('center_axis',(-0.624280230025758,0.,0.781200482846104));
#50903=DIRECTION('ref_axis',(0.781200482846104,0.,0.624280230025758));
#50904=DIRECTION('',(0.,1.,0.));
#50905=DIRECTION('center_axis',(-0.988679578606275,0.,-0.150042296859647));
#50906=DIRECTION('ref_axis',(-0.150042296859647,0.,0.988679578606275));
#50907=DIRECTION('',(0.,1.,0.));
#50908=DIRECTION('center_axis',(-0.364399348580519,0.,-0.931242779705751));
#50909=DIRECTION('ref_axis',(-0.931242779705751,0.,0.364399348580519));
#50910=DIRECTION('',(0.,1.,0.));
#50911=DIRECTION('center_axis',(0.624280230025758,0.,-0.781200482846105));
#50912=DIRECTION('ref_axis',(-0.781200482846105,0.,-0.624280230025758));
#50913=DIRECTION('center_axis',(0.988679578606276,0.,0.150042296859641));
#50914=DIRECTION('ref_axis',(0.150042296859641,0.,-0.988679578606276));
#50915=DIRECTION('',(0.,1.,0.));
#50916=DIRECTION('',(0.,1.,0.));
#50917=DIRECTION('center_axis',(0.364399348580517,0.,0.931242779705752));
#50918=DIRECTION('ref_axis',(0.931242779705752,0.,-0.364399348580517));
#50919=DIRECTION('',(0.,1.,0.));
#50920=DIRECTION('center_axis',(-0.624280230025758,0.,0.781200482846104));
#50921=DIRECTION('ref_axis',(0.781200482846104,0.,0.624280230025758));
#50922=DIRECTION('',(0.,1.,0.));
#50923=DIRECTION('center_axis',(-0.988679578606275,0.,-0.150042296859647));
#50924=DIRECTION('ref_axis',(-0.150042296859647,0.,0.988679578606275));
#50925=DIRECTION('',(0.,1.,0.));
#50926=DIRECTION('center_axis',(-0.364399348580519,0.,-0.931242779705751));
#50927=DIRECTION('ref_axis',(-0.931242779705751,0.,0.364399348580519));
#50928=DIRECTION('',(0.,1.,0.));
#50929=DIRECTION('center_axis',(0.624280230025758,0.,-0.781200482846105));
#50930=DIRECTION('ref_axis',(-0.781200482846105,0.,-0.624280230025758));
#50931=DIRECTION('center_axis',(0.988679578606276,0.,0.150042296859641));
#50932=DIRECTION('ref_axis',(0.150042296859641,0.,-0.988679578606276));
#50933=DIRECTION('',(0.,1.,0.));
#50934=DIRECTION('',(0.,1.,0.));
#50935=DIRECTION('center_axis',(0.364399348580517,0.,0.931242779705752));
#50936=DIRECTION('ref_axis',(0.931242779705752,0.,-0.364399348580517));
#50937=DIRECTION('',(0.,1.,0.));
#50938=DIRECTION('center_axis',(-0.624280230025758,0.,0.781200482846104));
#50939=DIRECTION('ref_axis',(0.781200482846104,0.,0.624280230025758));
#50940=DIRECTION('',(0.,1.,0.));
#50941=DIRECTION('center_axis',(-0.988679578606275,0.,-0.150042296859647));
#50942=DIRECTION('ref_axis',(-0.150042296859647,0.,0.988679578606275));
#50943=DIRECTION('',(0.,1.,0.));
#50944=DIRECTION('center_axis',(-0.364399348580519,0.,-0.931242779705751));
#50945=DIRECTION('ref_axis',(-0.931242779705751,0.,0.364399348580519));
#50946=DIRECTION('',(0.,1.,0.));
#50947=DIRECTION('center_axis',(0.624280230025758,0.,-0.781200482846105));
#50948=DIRECTION('ref_axis',(-0.781200482846105,0.,-0.624280230025758));
#50949=DIRECTION('center_axis',(0.988679578606276,0.,0.150042296859641));
#50950=DIRECTION('ref_axis',(0.150042296859641,0.,-0.988679578606276));
#50951=DIRECTION('',(0.,1.,0.));
#50952=DIRECTION('',(0.,1.,0.));
#50953=DIRECTION('center_axis',(0.364399348580517,0.,0.931242779705752));
#50954=DIRECTION('ref_axis',(0.931242779705752,0.,-0.364399348580517));
#50955=DIRECTION('',(0.,1.,0.));
#50956=DIRECTION('center_axis',(-0.624280230025758,0.,0.781200482846104));
#50957=DIRECTION('ref_axis',(0.781200482846104,0.,0.624280230025758));
#50958=DIRECTION('',(0.,1.,0.));
#50959=DIRECTION('center_axis',(-0.988679578606275,0.,-0.150042296859647));
#50960=DIRECTION('ref_axis',(-0.150042296859647,0.,0.988679578606275));
#50961=DIRECTION('',(0.,1.,0.));
#50962=DIRECTION('center_axis',(-0.364399348580519,0.,-0.931242779705751));
#50963=DIRECTION('ref_axis',(-0.931242779705751,0.,0.364399348580519));
#50964=DIRECTION('',(0.,1.,0.));
#50965=DIRECTION('center_axis',(0.624280230025758,0.,-0.781200482846105));
#50966=DIRECTION('ref_axis',(-0.781200482846105,0.,-0.624280230025758));
#50967=DIRECTION('center_axis',(0.988679578606276,0.,0.150042296859641));
#50968=DIRECTION('ref_axis',(0.150042296859641,0.,-0.988679578606276));
#50969=DIRECTION('',(0.,1.,0.));
#50970=DIRECTION('',(0.,1.,0.));
#50971=DIRECTION('center_axis',(0.364399348580517,0.,0.931242779705752));
#50972=DIRECTION('ref_axis',(0.931242779705752,0.,-0.364399348580517));
#50973=DIRECTION('',(0.,1.,0.));
#50974=DIRECTION('center_axis',(-0.624280230025758,0.,0.781200482846104));
#50975=DIRECTION('ref_axis',(0.781200482846104,0.,0.624280230025758));
#50976=DIRECTION('',(0.,1.,0.));
#50977=DIRECTION('center_axis',(-0.988679578606275,0.,-0.150042296859647));
#50978=DIRECTION('ref_axis',(-0.150042296859647,0.,0.988679578606275));
#50979=DIRECTION('',(0.,1.,0.));
#50980=DIRECTION('center_axis',(-0.364399348580519,0.,-0.931242779705751));
#50981=DIRECTION('ref_axis',(-0.931242779705751,0.,0.364399348580519));
#50982=DIRECTION('',(0.,1.,0.));
#50983=DIRECTION('center_axis',(0.624280230025758,0.,-0.781200482846105));
#50984=DIRECTION('ref_axis',(-0.781200482846105,0.,-0.624280230025758));
#50985=DIRECTION('center_axis',(0.988679578606276,0.,0.150042296859641));
#50986=DIRECTION('ref_axis',(0.150042296859641,0.,-0.988679578606276));
#50987=DIRECTION('',(0.,1.,0.));
#50988=DIRECTION('',(0.,1.,0.));
#50989=DIRECTION('center_axis',(0.364399348580517,0.,0.931242779705752));
#50990=DIRECTION('ref_axis',(0.931242779705752,0.,-0.364399348580517));
#50991=DIRECTION('',(0.,1.,0.));
#50992=DIRECTION('center_axis',(-0.624280230025758,0.,0.781200482846104));
#50993=DIRECTION('ref_axis',(0.781200482846104,0.,0.624280230025758));
#50994=DIRECTION('',(0.,1.,0.));
#50995=DIRECTION('center_axis',(-0.988679578606275,0.,-0.150042296859647));
#50996=DIRECTION('ref_axis',(-0.150042296859647,0.,0.988679578606275));
#50997=DIRECTION('',(0.,1.,0.));
#50998=DIRECTION('center_axis',(-0.364399348580519,0.,-0.931242779705751));
#50999=DIRECTION('ref_axis',(-0.931242779705751,0.,0.364399348580519));
#51000=DIRECTION('',(0.,1.,0.));
#51001=DIRECTION('center_axis',(0.624280230025758,0.,-0.781200482846105));
#51002=DIRECTION('ref_axis',(-0.781200482846105,0.,-0.624280230025758));
#51003=DIRECTION('center_axis',(0.988679578606276,0.,0.150042296859641));
#51004=DIRECTION('ref_axis',(0.150042296859641,0.,-0.988679578606276));
#51005=DIRECTION('',(0.,1.,0.));
#51006=DIRECTION('',(0.,1.,0.));
#51007=DIRECTION('center_axis',(0.364399348580517,0.,0.931242779705752));
#51008=DIRECTION('ref_axis',(0.931242779705752,0.,-0.364399348580517));
#51009=DIRECTION('',(0.,1.,0.));
#51010=DIRECTION('center_axis',(-0.624280230025758,0.,0.781200482846104));
#51011=DIRECTION('ref_axis',(0.781200482846104,0.,0.624280230025758));
#51012=DIRECTION('',(0.,1.,0.));
#51013=DIRECTION('center_axis',(-0.988679578606275,0.,-0.150042296859647));
#51014=DIRECTION('ref_axis',(-0.150042296859647,0.,0.988679578606275));
#51015=DIRECTION('',(0.,1.,0.));
#51016=DIRECTION('center_axis',(-0.364399348580519,0.,-0.931242779705751));
#51017=DIRECTION('ref_axis',(-0.931242779705751,0.,0.364399348580519));
#51018=DIRECTION('',(0.,1.,0.));
#51019=DIRECTION('center_axis',(0.624280230025758,0.,-0.781200482846105));
#51020=DIRECTION('ref_axis',(-0.781200482846105,0.,-0.624280230025758));
#51021=DIRECTION('center_axis',(0.988679578606276,0.,0.150042296859641));
#51022=DIRECTION('ref_axis',(0.150042296859641,0.,-0.988679578606276));
#51023=DIRECTION('',(0.,1.,0.));
#51024=DIRECTION('',(0.,1.,0.));
#51025=DIRECTION('center_axis',(0.364399348580517,0.,0.931242779705752));
#51026=DIRECTION('ref_axis',(0.931242779705752,0.,-0.364399348580517));
#51027=DIRECTION('',(0.,1.,0.));
#51028=DIRECTION('center_axis',(-0.624280230025758,0.,0.781200482846104));
#51029=DIRECTION('ref_axis',(0.781200482846104,0.,0.624280230025758));
#51030=DIRECTION('',(0.,1.,0.));
#51031=DIRECTION('center_axis',(-0.988679578606275,0.,-0.150042296859647));
#51032=DIRECTION('ref_axis',(-0.150042296859647,0.,0.988679578606275));
#51033=DIRECTION('',(0.,1.,0.));
#51034=DIRECTION('center_axis',(-0.364399348580519,0.,-0.931242779705751));
#51035=DIRECTION('ref_axis',(-0.931242779705751,0.,0.364399348580519));
#51036=DIRECTION('',(0.,1.,0.));
#51037=DIRECTION('center_axis',(0.624280230025758,0.,-0.781200482846105));
#51038=DIRECTION('ref_axis',(-0.781200482846105,0.,-0.624280230025758));
#51039=DIRECTION('center_axis',(0.988679578606276,0.,0.150042296859641));
#51040=DIRECTION('ref_axis',(0.150042296859641,0.,-0.988679578606276));
#51041=DIRECTION('',(0.,1.,0.));
#51042=DIRECTION('',(0.,1.,0.));
#51043=DIRECTION('center_axis',(0.364399348580517,0.,0.931242779705752));
#51044=DIRECTION('ref_axis',(0.931242779705752,0.,-0.364399348580517));
#51045=DIRECTION('',(0.,1.,0.));
#51046=DIRECTION('center_axis',(-0.624280230025758,0.,0.781200482846104));
#51047=DIRECTION('ref_axis',(0.781200482846104,0.,0.624280230025758));
#51048=DIRECTION('',(0.,1.,0.));
#51049=DIRECTION('center_axis',(-0.988679578606275,0.,-0.150042296859647));
#51050=DIRECTION('ref_axis',(-0.150042296859647,0.,0.988679578606275));
#51051=DIRECTION('',(0.,1.,0.));
#51052=DIRECTION('center_axis',(-0.364399348580519,0.,-0.931242779705751));
#51053=DIRECTION('ref_axis',(-0.931242779705751,0.,0.364399348580519));
#51054=DIRECTION('',(0.,1.,0.));
#51055=DIRECTION('center_axis',(0.624280230025758,0.,-0.781200482846105));
#51056=DIRECTION('ref_axis',(-0.781200482846105,0.,-0.624280230025758));
#51057=DIRECTION('center_axis',(0.988679578606276,0.,0.150042296859641));
#51058=DIRECTION('ref_axis',(0.150042296859641,0.,-0.988679578606276));
#51059=DIRECTION('',(0.,1.,0.));
#51060=DIRECTION('',(0.,1.,0.));
#51061=DIRECTION('center_axis',(0.364399348580517,0.,0.931242779705752));
#51062=DIRECTION('ref_axis',(0.931242779705752,0.,-0.364399348580517));
#51063=DIRECTION('',(0.,1.,0.));
#51064=DIRECTION('center_axis',(-0.624280230025758,0.,0.781200482846104));
#51065=DIRECTION('ref_axis',(0.781200482846104,0.,0.624280230025758));
#51066=DIRECTION('',(0.,1.,0.));
#51067=DIRECTION('center_axis',(-0.988679578606275,0.,-0.150042296859647));
#51068=DIRECTION('ref_axis',(-0.150042296859647,0.,0.988679578606275));
#51069=DIRECTION('',(0.,1.,0.));
#51070=DIRECTION('center_axis',(-0.364399348580519,0.,-0.931242779705751));
#51071=DIRECTION('ref_axis',(-0.931242779705751,0.,0.364399348580519));
#51072=DIRECTION('',(0.,1.,0.));
#51073=DIRECTION('center_axis',(0.624280230025758,0.,-0.781200482846105));
#51074=DIRECTION('ref_axis',(-0.781200482846105,0.,-0.624280230025758));
#51075=DIRECTION('center_axis',(0.988679578606276,0.,0.150042296859641));
#51076=DIRECTION('ref_axis',(0.150042296859641,0.,-0.988679578606276));
#51077=DIRECTION('',(0.,1.,0.));
#51078=DIRECTION('',(0.,1.,0.));
#51079=DIRECTION('center_axis',(0.364399348580517,0.,0.931242779705752));
#51080=DIRECTION('ref_axis',(0.931242779705752,0.,-0.364399348580517));
#51081=DIRECTION('',(0.,1.,0.));
#51082=DIRECTION('center_axis',(-0.624280230025758,0.,0.781200482846104));
#51083=DIRECTION('ref_axis',(0.781200482846104,0.,0.624280230025758));
#51084=DIRECTION('',(0.,1.,0.));
#51085=DIRECTION('center_axis',(-0.988679578606275,0.,-0.150042296859647));
#51086=DIRECTION('ref_axis',(-0.150042296859647,0.,0.988679578606275));
#51087=DIRECTION('',(0.,1.,0.));
#51088=DIRECTION('center_axis',(-0.364399348580519,0.,-0.931242779705751));
#51089=DIRECTION('ref_axis',(-0.931242779705751,0.,0.364399348580519));
#51090=DIRECTION('',(0.,1.,0.));
#51091=DIRECTION('center_axis',(0.624280230025758,0.,-0.781200482846105));
#51092=DIRECTION('ref_axis',(-0.781200482846105,0.,-0.624280230025758));
#51093=DIRECTION('center_axis',(0.988679578606276,0.,0.150042296859641));
#51094=DIRECTION('ref_axis',(0.150042296859641,0.,-0.988679578606276));
#51095=DIRECTION('',(0.,1.,0.));
#51096=DIRECTION('',(0.,1.,0.));
#51097=DIRECTION('center_axis',(0.364399348580517,0.,0.931242779705752));
#51098=DIRECTION('ref_axis',(0.931242779705752,0.,-0.364399348580517));
#51099=DIRECTION('',(0.,1.,0.));
#51100=DIRECTION('center_axis',(-0.624280230025758,0.,0.781200482846104));
#51101=DIRECTION('ref_axis',(0.781200482846104,0.,0.624280230025758));
#51102=DIRECTION('',(0.,1.,0.));
#51103=DIRECTION('center_axis',(-0.988679578606275,0.,-0.150042296859647));
#51104=DIRECTION('ref_axis',(-0.150042296859647,0.,0.988679578606275));
#51105=DIRECTION('',(0.,1.,0.));
#51106=DIRECTION('center_axis',(-0.364399348580519,0.,-0.931242779705751));
#51107=DIRECTION('ref_axis',(-0.931242779705751,0.,0.364399348580519));
#51108=DIRECTION('',(0.,1.,0.));
#51109=DIRECTION('center_axis',(0.624280230025758,0.,-0.781200482846105));
#51110=DIRECTION('ref_axis',(-0.781200482846105,0.,-0.624280230025758));
#51111=DIRECTION('center_axis',(0.988679578606276,0.,0.150042296859641));
#51112=DIRECTION('ref_axis',(0.150042296859641,0.,-0.988679578606276));
#51113=DIRECTION('',(0.,1.,0.));
#51114=DIRECTION('',(0.,1.,0.));
#51115=DIRECTION('center_axis',(0.364399348580517,0.,0.931242779705752));
#51116=DIRECTION('ref_axis',(0.931242779705752,0.,-0.364399348580517));
#51117=DIRECTION('',(0.,1.,0.));
#51118=DIRECTION('center_axis',(-0.624280230025758,0.,0.781200482846104));
#51119=DIRECTION('ref_axis',(0.781200482846104,0.,0.624280230025758));
#51120=DIRECTION('',(0.,1.,0.));
#51121=DIRECTION('center_axis',(-0.988679578606275,0.,-0.150042296859647));
#51122=DIRECTION('ref_axis',(-0.150042296859647,0.,0.988679578606275));
#51123=DIRECTION('',(0.,1.,0.));
#51124=DIRECTION('center_axis',(-0.364399348580519,0.,-0.931242779705751));
#51125=DIRECTION('ref_axis',(-0.931242779705751,0.,0.364399348580519));
#51126=DIRECTION('',(0.,1.,0.));
#51127=DIRECTION('center_axis',(0.624280230025758,0.,-0.781200482846105));
#51128=DIRECTION('ref_axis',(-0.781200482846105,0.,-0.624280230025758));
#51129=DIRECTION('center_axis',(0.988679578606276,0.,0.150042296859641));
#51130=DIRECTION('ref_axis',(0.150042296859641,0.,-0.988679578606276));
#51131=DIRECTION('',(0.,1.,0.));
#51132=DIRECTION('',(0.,1.,0.));
#51133=DIRECTION('center_axis',(0.364399348580517,0.,0.931242779705752));
#51134=DIRECTION('ref_axis',(0.931242779705752,0.,-0.364399348580517));
#51135=DIRECTION('',(0.,1.,0.));
#51136=DIRECTION('center_axis',(-0.624280230025758,0.,0.781200482846104));
#51137=DIRECTION('ref_axis',(0.781200482846104,0.,0.624280230025758));
#51138=DIRECTION('',(0.,1.,0.));
#51139=DIRECTION('center_axis',(-0.988679578606275,0.,-0.150042296859647));
#51140=DIRECTION('ref_axis',(-0.150042296859647,0.,0.988679578606275));
#51141=DIRECTION('',(0.,1.,0.));
#51142=DIRECTION('center_axis',(-0.364399348580519,0.,-0.931242779705751));
#51143=DIRECTION('ref_axis',(-0.931242779705751,0.,0.364399348580519));
#51144=DIRECTION('',(0.,1.,0.));
#51145=DIRECTION('center_axis',(0.624280230025758,0.,-0.781200482846105));
#51146=DIRECTION('ref_axis',(-0.781200482846105,0.,-0.624280230025758));
#51147=DIRECTION('center_axis',(0.988679578606276,0.,0.150042296859641));
#51148=DIRECTION('ref_axis',(0.150042296859641,0.,-0.988679578606276));
#51149=DIRECTION('',(0.,1.,0.));
#51150=DIRECTION('',(0.,1.,0.));
#51151=DIRECTION('center_axis',(0.364399348580517,0.,0.931242779705752));
#51152=DIRECTION('ref_axis',(0.931242779705752,0.,-0.364399348580517));
#51153=DIRECTION('',(0.,1.,0.));
#51154=DIRECTION('center_axis',(-0.624280230025758,0.,0.781200482846104));
#51155=DIRECTION('ref_axis',(0.781200482846104,0.,0.624280230025758));
#51156=DIRECTION('',(0.,1.,0.));
#51157=DIRECTION('center_axis',(-0.988679578606275,0.,-0.150042296859647));
#51158=DIRECTION('ref_axis',(-0.150042296859647,0.,0.988679578606275));
#51159=DIRECTION('',(0.,1.,0.));
#51160=DIRECTION('center_axis',(-0.364399348580519,0.,-0.931242779705751));
#51161=DIRECTION('ref_axis',(-0.931242779705751,0.,0.364399348580519));
#51162=DIRECTION('',(0.,1.,0.));
#51163=DIRECTION('center_axis',(0.624280230025758,0.,-0.781200482846105));
#51164=DIRECTION('ref_axis',(-0.781200482846105,0.,-0.624280230025758));
#51165=DIRECTION('center_axis',(0.988679578606276,0.,0.150042296859641));
#51166=DIRECTION('ref_axis',(0.150042296859641,0.,-0.988679578606276));
#51167=DIRECTION('',(0.,1.,0.));
#51168=DIRECTION('',(0.,1.,0.));
#51169=DIRECTION('center_axis',(0.364399348580517,0.,0.931242779705752));
#51170=DIRECTION('ref_axis',(0.931242779705752,0.,-0.364399348580517));
#51171=DIRECTION('',(0.,1.,0.));
#51172=DIRECTION('center_axis',(-0.624280230025758,0.,0.781200482846104));
#51173=DIRECTION('ref_axis',(0.781200482846104,0.,0.624280230025758));
#51174=DIRECTION('',(0.,1.,0.));
#51175=DIRECTION('center_axis',(-0.988679578606275,0.,-0.150042296859647));
#51176=DIRECTION('ref_axis',(-0.150042296859647,0.,0.988679578606275));
#51177=DIRECTION('',(0.,1.,0.));
#51178=DIRECTION('center_axis',(-0.364399348580519,0.,-0.931242779705751));
#51179=DIRECTION('ref_axis',(-0.931242779705751,0.,0.364399348580519));
#51180=DIRECTION('',(0.,1.,0.));
#51181=DIRECTION('center_axis',(0.624280230025758,0.,-0.781200482846105));
#51182=DIRECTION('ref_axis',(-0.781200482846105,0.,-0.624280230025758));
#51183=DIRECTION('center_axis',(0.988679578606276,0.,0.150042296859641));
#51184=DIRECTION('ref_axis',(0.150042296859641,0.,-0.988679578606276));
#51185=DIRECTION('',(0.,1.,0.));
#51186=DIRECTION('',(0.,1.,0.));
#51187=DIRECTION('center_axis',(0.364399348580517,0.,0.931242779705752));
#51188=DIRECTION('ref_axis',(0.931242779705752,0.,-0.364399348580517));
#51189=DIRECTION('',(0.,1.,0.));
#51190=DIRECTION('center_axis',(-0.624280230025758,0.,0.781200482846104));
#51191=DIRECTION('ref_axis',(0.781200482846104,0.,0.624280230025758));
#51192=DIRECTION('',(0.,1.,0.));
#51193=DIRECTION('center_axis',(-0.988679578606275,0.,-0.150042296859647));
#51194=DIRECTION('ref_axis',(-0.150042296859647,0.,0.988679578606275));
#51195=DIRECTION('',(0.,1.,0.));
#51196=DIRECTION('center_axis',(-0.364399348580519,0.,-0.931242779705751));
#51197=DIRECTION('ref_axis',(-0.931242779705751,0.,0.364399348580519));
#51198=DIRECTION('',(0.,1.,0.));
#51199=DIRECTION('center_axis',(0.624280230025758,0.,-0.781200482846105));
#51200=DIRECTION('ref_axis',(-0.781200482846105,0.,-0.624280230025758));
#51201=DIRECTION('center_axis',(0.988679578606276,0.,0.150042296859641));
#51202=DIRECTION('ref_axis',(0.150042296859641,0.,-0.988679578606276));
#51203=DIRECTION('',(0.,1.,0.));
#51204=DIRECTION('',(0.,1.,0.));
#51205=DIRECTION('center_axis',(0.364399348580517,0.,0.931242779705752));
#51206=DIRECTION('ref_axis',(0.931242779705752,0.,-0.364399348580517));
#51207=DIRECTION('',(0.,1.,0.));
#51208=DIRECTION('center_axis',(-0.624280230025758,0.,0.781200482846104));
#51209=DIRECTION('ref_axis',(0.781200482846104,0.,0.624280230025758));
#51210=DIRECTION('',(0.,1.,0.));
#51211=DIRECTION('center_axis',(-0.988679578606275,0.,-0.150042296859647));
#51212=DIRECTION('ref_axis',(-0.150042296859647,0.,0.988679578606275));
#51213=DIRECTION('',(0.,1.,0.));
#51214=DIRECTION('center_axis',(-0.364399348580519,0.,-0.931242779705751));
#51215=DIRECTION('ref_axis',(-0.931242779705751,0.,0.364399348580519));
#51216=DIRECTION('',(0.,1.,0.));
#51217=DIRECTION('center_axis',(0.624280230025758,0.,-0.781200482846105));
#51218=DIRECTION('ref_axis',(-0.781200482846105,0.,-0.624280230025758));
#51219=DIRECTION('center_axis',(0.988679578606276,0.,0.150042296859641));
#51220=DIRECTION('ref_axis',(0.150042296859641,0.,-0.988679578606276));
#51221=DIRECTION('',(0.,1.,0.));
#51222=DIRECTION('',(0.,1.,0.));
#51223=DIRECTION('center_axis',(0.364399348580517,0.,0.931242779705752));
#51224=DIRECTION('ref_axis',(0.931242779705752,0.,-0.364399348580517));
#51225=DIRECTION('',(0.,1.,0.));
#51226=DIRECTION('center_axis',(-0.624280230025758,0.,0.781200482846104));
#51227=DIRECTION('ref_axis',(0.781200482846104,0.,0.624280230025758));
#51228=DIRECTION('',(0.,1.,0.));
#51229=DIRECTION('center_axis',(-0.988679578606275,0.,-0.150042296859647));
#51230=DIRECTION('ref_axis',(-0.150042296859647,0.,0.988679578606275));
#51231=DIRECTION('',(0.,1.,0.));
#51232=DIRECTION('center_axis',(-0.364399348580519,0.,-0.931242779705751));
#51233=DIRECTION('ref_axis',(-0.931242779705751,0.,0.364399348580519));
#51234=DIRECTION('',(0.,1.,0.));
#51235=DIRECTION('center_axis',(0.624280230025758,0.,-0.781200482846105));
#51236=DIRECTION('ref_axis',(-0.781200482846105,0.,-0.624280230025758));
#51237=DIRECTION('center_axis',(0.988679578606276,0.,0.150042296859641));
#51238=DIRECTION('ref_axis',(0.150042296859641,0.,-0.988679578606276));
#51239=DIRECTION('',(0.,1.,0.));
#51240=DIRECTION('',(0.,1.,0.));
#51241=DIRECTION('center_axis',(0.364399348580517,0.,0.931242779705752));
#51242=DIRECTION('ref_axis',(0.931242779705752,0.,-0.364399348580517));
#51243=DIRECTION('',(0.,1.,0.));
#51244=DIRECTION('center_axis',(-0.624280230025758,0.,0.781200482846104));
#51245=DIRECTION('ref_axis',(0.781200482846104,0.,0.624280230025758));
#51246=DIRECTION('',(0.,1.,0.));
#51247=DIRECTION('center_axis',(-0.988679578606275,0.,-0.150042296859647));
#51248=DIRECTION('ref_axis',(-0.150042296859647,0.,0.988679578606275));
#51249=DIRECTION('',(0.,1.,0.));
#51250=DIRECTION('center_axis',(-0.364399348580519,0.,-0.931242779705751));
#51251=DIRECTION('ref_axis',(-0.931242779705751,0.,0.364399348580519));
#51252=DIRECTION('',(0.,1.,0.));
#51253=DIRECTION('center_axis',(0.624280230025758,0.,-0.781200482846105));
#51254=DIRECTION('ref_axis',(-0.781200482846105,0.,-0.624280230025758));
#51255=DIRECTION('center_axis',(0.988679578606276,0.,0.150042296859641));
#51256=DIRECTION('ref_axis',(0.150042296859641,0.,-0.988679578606276));
#51257=DIRECTION('',(0.,1.,0.));
#51258=DIRECTION('',(0.,1.,0.));
#51259=DIRECTION('center_axis',(0.364399348580517,0.,0.931242779705752));
#51260=DIRECTION('ref_axis',(0.931242779705752,0.,-0.364399348580517));
#51261=DIRECTION('',(0.,1.,0.));
#51262=DIRECTION('center_axis',(-0.624280230025758,0.,0.781200482846104));
#51263=DIRECTION('ref_axis',(0.781200482846104,0.,0.624280230025758));
#51264=DIRECTION('',(0.,1.,0.));
#51265=DIRECTION('center_axis',(-0.988679578606275,0.,-0.150042296859647));
#51266=DIRECTION('ref_axis',(-0.150042296859647,0.,0.988679578606275));
#51267=DIRECTION('',(0.,1.,0.));
#51268=DIRECTION('center_axis',(-0.364399348580519,0.,-0.931242779705751));
#51269=DIRECTION('ref_axis',(-0.931242779705751,0.,0.364399348580519));
#51270=DIRECTION('',(0.,1.,0.));
#51271=DIRECTION('center_axis',(0.624280230025758,0.,-0.781200482846105));
#51272=DIRECTION('ref_axis',(-0.781200482846105,0.,-0.624280230025758));
#51273=DIRECTION('center_axis',(0.988679578606276,0.,0.150042296859641));
#51274=DIRECTION('ref_axis',(0.150042296859641,0.,-0.988679578606276));
#51275=DIRECTION('',(0.,1.,0.));
#51276=DIRECTION('',(0.,1.,0.));
#51277=DIRECTION('center_axis',(0.364399348580517,0.,0.931242779705752));
#51278=DIRECTION('ref_axis',(0.931242779705752,0.,-0.364399348580517));
#51279=DIRECTION('',(0.,1.,0.));
#51280=DIRECTION('center_axis',(-0.624280230025758,0.,0.781200482846104));
#51281=DIRECTION('ref_axis',(0.781200482846104,0.,0.624280230025758));
#51282=DIRECTION('',(0.,1.,0.));
#51283=DIRECTION('center_axis',(-0.988679578606275,0.,-0.150042296859647));
#51284=DIRECTION('ref_axis',(-0.150042296859647,0.,0.988679578606275));
#51285=DIRECTION('',(0.,1.,0.));
#51286=DIRECTION('center_axis',(-0.364399348580519,0.,-0.931242779705751));
#51287=DIRECTION('ref_axis',(-0.931242779705751,0.,0.364399348580519));
#51288=DIRECTION('',(0.,1.,0.));
#51289=DIRECTION('center_axis',(0.624280230025758,0.,-0.781200482846105));
#51290=DIRECTION('ref_axis',(-0.781200482846105,0.,-0.624280230025758));
#51291=DIRECTION('center_axis',(0.988679578606276,0.,0.150042296859641));
#51292=DIRECTION('ref_axis',(0.150042296859641,0.,-0.988679578606276));
#51293=DIRECTION('',(0.,1.,0.));
#51294=DIRECTION('',(0.,1.,0.));
#51295=DIRECTION('center_axis',(0.364399348580517,0.,0.931242779705752));
#51296=DIRECTION('ref_axis',(0.931242779705752,0.,-0.364399348580517));
#51297=DIRECTION('',(0.,1.,0.));
#51298=DIRECTION('center_axis',(-0.624280230025758,0.,0.781200482846104));
#51299=DIRECTION('ref_axis',(0.781200482846104,0.,0.624280230025758));
#51300=DIRECTION('',(0.,1.,0.));
#51301=DIRECTION('center_axis',(-0.988679578606275,0.,-0.150042296859647));
#51302=DIRECTION('ref_axis',(-0.150042296859647,0.,0.988679578606275));
#51303=DIRECTION('',(0.,1.,0.));
#51304=DIRECTION('center_axis',(-0.364399348580519,0.,-0.931242779705751));
#51305=DIRECTION('ref_axis',(-0.931242779705751,0.,0.364399348580519));
#51306=DIRECTION('',(0.,1.,0.));
#51307=DIRECTION('center_axis',(0.624280230025758,0.,-0.781200482846105));
#51308=DIRECTION('ref_axis',(-0.781200482846105,0.,-0.624280230025758));
#51309=DIRECTION('center_axis',(0.988679578606276,0.,0.150042296859641));
#51310=DIRECTION('ref_axis',(0.150042296859641,0.,-0.988679578606276));
#51311=DIRECTION('',(0.,1.,0.));
#51312=DIRECTION('',(0.,1.,0.));
#51313=DIRECTION('center_axis',(0.364399348580517,0.,0.931242779705752));
#51314=DIRECTION('ref_axis',(0.931242779705752,0.,-0.364399348580517));
#51315=DIRECTION('',(0.,1.,0.));
#51316=DIRECTION('center_axis',(-0.624280230025758,0.,0.781200482846104));
#51317=DIRECTION('ref_axis',(0.781200482846104,0.,0.624280230025758));
#51318=DIRECTION('',(0.,1.,0.));
#51319=DIRECTION('center_axis',(-0.988679578606275,0.,-0.150042296859647));
#51320=DIRECTION('ref_axis',(-0.150042296859647,0.,0.988679578606275));
#51321=DIRECTION('',(0.,1.,0.));
#51322=DIRECTION('center_axis',(-0.364399348580519,0.,-0.931242779705751));
#51323=DIRECTION('ref_axis',(-0.931242779705751,0.,0.364399348580519));
#51324=DIRECTION('',(0.,1.,0.));
#51325=DIRECTION('center_axis',(0.624280230025758,0.,-0.781200482846105));
#51326=DIRECTION('ref_axis',(-0.781200482846105,0.,-0.624280230025758));
#51327=DIRECTION('center_axis',(0.988679578606276,0.,0.150042296859641));
#51328=DIRECTION('ref_axis',(0.150042296859641,0.,-0.988679578606276));
#51329=DIRECTION('',(0.,1.,0.));
#51330=DIRECTION('',(0.,1.,0.));
#51331=DIRECTION('center_axis',(0.364399348580517,0.,0.931242779705752));
#51332=DIRECTION('ref_axis',(0.931242779705752,0.,-0.364399348580517));
#51333=DIRECTION('',(0.,1.,0.));
#51334=DIRECTION('center_axis',(-0.624280230025758,0.,0.781200482846104));
#51335=DIRECTION('ref_axis',(0.781200482846104,0.,0.624280230025758));
#51336=DIRECTION('',(0.,1.,0.));
#51337=DIRECTION('center_axis',(-0.988679578606275,0.,-0.150042296859647));
#51338=DIRECTION('ref_axis',(-0.150042296859647,0.,0.988679578606275));
#51339=DIRECTION('',(0.,1.,0.));
#51340=DIRECTION('center_axis',(-0.364399348580519,0.,-0.931242779705751));
#51341=DIRECTION('ref_axis',(-0.931242779705751,0.,0.364399348580519));
#51342=DIRECTION('',(0.,1.,0.));
#51343=DIRECTION('center_axis',(0.624280230025758,0.,-0.781200482846105));
#51344=DIRECTION('ref_axis',(-0.781200482846105,0.,-0.624280230025758));
#51345=DIRECTION('center_axis',(0.988679578606276,0.,0.150042296859641));
#51346=DIRECTION('ref_axis',(0.150042296859641,0.,-0.988679578606276));
#51347=DIRECTION('',(0.,1.,0.));
#51348=DIRECTION('',(0.,1.,0.));
#51349=DIRECTION('center_axis',(0.364399348580517,0.,0.931242779705752));
#51350=DIRECTION('ref_axis',(0.931242779705752,0.,-0.364399348580517));
#51351=DIRECTION('',(0.,1.,0.));
#51352=DIRECTION('center_axis',(-0.624280230025758,0.,0.781200482846104));
#51353=DIRECTION('ref_axis',(0.781200482846104,0.,0.624280230025758));
#51354=DIRECTION('',(0.,1.,0.));
#51355=DIRECTION('center_axis',(-0.988679578606275,0.,-0.150042296859647));
#51356=DIRECTION('ref_axis',(-0.150042296859647,0.,0.988679578606275));
#51357=DIRECTION('',(0.,1.,0.));
#51358=DIRECTION('center_axis',(-0.364399348580519,0.,-0.931242779705751));
#51359=DIRECTION('ref_axis',(-0.931242779705751,0.,0.364399348580519));
#51360=DIRECTION('',(0.,1.,0.));
#51361=DIRECTION('center_axis',(0.624280230025758,0.,-0.781200482846105));
#51362=DIRECTION('ref_axis',(-0.781200482846105,0.,-0.624280230025758));
#51363=DIRECTION('center_axis',(0.988679578606276,0.,0.150042296859641));
#51364=DIRECTION('ref_axis',(0.150042296859641,0.,-0.988679578606276));
#51365=DIRECTION('',(0.,1.,0.));
#51366=DIRECTION('',(0.,1.,0.));
#51367=DIRECTION('center_axis',(0.364399348580517,0.,0.931242779705752));
#51368=DIRECTION('ref_axis',(0.931242779705752,0.,-0.364399348580517));
#51369=DIRECTION('',(0.,1.,0.));
#51370=DIRECTION('center_axis',(-0.624280230025758,0.,0.781200482846104));
#51371=DIRECTION('ref_axis',(0.781200482846104,0.,0.624280230025758));
#51372=DIRECTION('',(0.,1.,0.));
#51373=DIRECTION('center_axis',(-0.988679578606275,0.,-0.150042296859647));
#51374=DIRECTION('ref_axis',(-0.150042296859647,0.,0.988679578606275));
#51375=DIRECTION('',(0.,1.,0.));
#51376=DIRECTION('center_axis',(-0.364399348580519,0.,-0.931242779705751));
#51377=DIRECTION('ref_axis',(-0.931242779705751,0.,0.364399348580519));
#51378=DIRECTION('',(0.,1.,0.));
#51379=DIRECTION('center_axis',(0.624280230025758,0.,-0.781200482846105));
#51380=DIRECTION('ref_axis',(-0.781200482846105,0.,-0.624280230025758));
#51381=DIRECTION('center_axis',(0.988679578606276,0.,0.150042296859641));
#51382=DIRECTION('ref_axis',(0.150042296859641,0.,-0.988679578606276));
#51383=DIRECTION('',(0.,1.,0.));
#51384=DIRECTION('',(0.,1.,0.));
#51385=DIRECTION('center_axis',(0.364399348580517,0.,0.931242779705752));
#51386=DIRECTION('ref_axis',(0.931242779705752,0.,-0.364399348580517));
#51387=DIRECTION('',(0.,1.,0.));
#51388=DIRECTION('center_axis',(-0.624280230025758,0.,0.781200482846104));
#51389=DIRECTION('ref_axis',(0.781200482846104,0.,0.624280230025758));
#51390=DIRECTION('',(0.,1.,0.));
#51391=DIRECTION('center_axis',(-0.988679578606275,0.,-0.150042296859647));
#51392=DIRECTION('ref_axis',(-0.150042296859647,0.,0.988679578606275));
#51393=DIRECTION('',(0.,1.,0.));
#51394=DIRECTION('center_axis',(-0.364399348580519,0.,-0.931242779705751));
#51395=DIRECTION('ref_axis',(-0.931242779705751,0.,0.364399348580519));
#51396=DIRECTION('',(0.,1.,0.));
#51397=DIRECTION('center_axis',(0.624280230025758,0.,-0.781200482846105));
#51398=DIRECTION('ref_axis',(-0.781200482846105,0.,-0.624280230025758));
#51399=DIRECTION('center_axis',(0.988679578606276,0.,0.150042296859641));
#51400=DIRECTION('ref_axis',(0.150042296859641,0.,-0.988679578606276));
#51401=DIRECTION('',(0.,1.,0.));
#51402=DIRECTION('',(0.,1.,0.));
#51403=DIRECTION('center_axis',(0.364399348580517,0.,0.931242779705752));
#51404=DIRECTION('ref_axis',(0.931242779705752,0.,-0.364399348580517));
#51405=DIRECTION('',(0.,1.,0.));
#51406=DIRECTION('center_axis',(-0.624280230025758,0.,0.781200482846104));
#51407=DIRECTION('ref_axis',(0.781200482846104,0.,0.624280230025758));
#51408=DIRECTION('',(0.,1.,0.));
#51409=DIRECTION('center_axis',(-0.988679578606275,0.,-0.150042296859647));
#51410=DIRECTION('ref_axis',(-0.150042296859647,0.,0.988679578606275));
#51411=DIRECTION('',(0.,1.,0.));
#51412=DIRECTION('center_axis',(-0.364399348580519,0.,-0.931242779705751));
#51413=DIRECTION('ref_axis',(-0.931242779705751,0.,0.364399348580519));
#51414=DIRECTION('',(0.,1.,0.));
#51415=DIRECTION('center_axis',(0.624280230025758,0.,-0.781200482846105));
#51416=DIRECTION('ref_axis',(-0.781200482846105,0.,-0.624280230025758));
#51417=DIRECTION('center_axis',(0.988679578606276,0.,0.150042296859641));
#51418=DIRECTION('ref_axis',(0.150042296859641,0.,-0.988679578606276));
#51419=DIRECTION('',(0.,1.,0.));
#51420=DIRECTION('',(0.,1.,0.));
#51421=DIRECTION('center_axis',(0.364399348580517,0.,0.931242779705752));
#51422=DIRECTION('ref_axis',(0.931242779705752,0.,-0.364399348580517));
#51423=DIRECTION('',(0.,1.,0.));
#51424=DIRECTION('center_axis',(-0.624280230025758,0.,0.781200482846104));
#51425=DIRECTION('ref_axis',(0.781200482846104,0.,0.624280230025758));
#51426=DIRECTION('',(0.,1.,0.));
#51427=DIRECTION('center_axis',(-0.988679578606275,0.,-0.150042296859647));
#51428=DIRECTION('ref_axis',(-0.150042296859647,0.,0.988679578606275));
#51429=DIRECTION('',(0.,1.,0.));
#51430=DIRECTION('center_axis',(-0.364399348580519,0.,-0.931242779705751));
#51431=DIRECTION('ref_axis',(-0.931242779705751,0.,0.364399348580519));
#51432=DIRECTION('',(0.,1.,0.));
#51433=DIRECTION('center_axis',(0.624280230025758,0.,-0.781200482846105));
#51434=DIRECTION('ref_axis',(-0.781200482846105,0.,-0.624280230025758));
#51435=DIRECTION('center_axis',(0.988679578606276,0.,0.150042296859641));
#51436=DIRECTION('ref_axis',(0.150042296859641,0.,-0.988679578606276));
#51437=DIRECTION('',(0.,1.,0.));
#51438=DIRECTION('',(0.,1.,0.));
#51439=DIRECTION('center_axis',(0.364399348580517,0.,0.931242779705752));
#51440=DIRECTION('ref_axis',(0.931242779705752,0.,-0.364399348580517));
#51441=DIRECTION('',(0.,1.,0.));
#51442=DIRECTION('center_axis',(-0.624280230025758,0.,0.781200482846104));
#51443=DIRECTION('ref_axis',(0.781200482846104,0.,0.624280230025758));
#51444=DIRECTION('',(0.,1.,0.));
#51445=DIRECTION('center_axis',(-0.988679578606275,0.,-0.150042296859647));
#51446=DIRECTION('ref_axis',(-0.150042296859647,0.,0.988679578606275));
#51447=DIRECTION('',(0.,1.,0.));
#51448=DIRECTION('center_axis',(-0.364399348580519,0.,-0.931242779705751));
#51449=DIRECTION('ref_axis',(-0.931242779705751,0.,0.364399348580519));
#51450=DIRECTION('',(0.,1.,0.));
#51451=DIRECTION('center_axis',(0.624280230025758,0.,-0.781200482846105));
#51452=DIRECTION('ref_axis',(-0.781200482846105,0.,-0.624280230025758));
#51453=DIRECTION('center_axis',(0.988679578606276,0.,0.150042296859641));
#51454=DIRECTION('ref_axis',(0.150042296859641,0.,-0.988679578606276));
#51455=DIRECTION('',(0.,1.,0.));
#51456=DIRECTION('',(0.,1.,0.));
#51457=DIRECTION('center_axis',(0.364399348580517,0.,0.931242779705752));
#51458=DIRECTION('ref_axis',(0.931242779705752,0.,-0.364399348580517));
#51459=DIRECTION('',(0.,1.,0.));
#51460=DIRECTION('center_axis',(-0.624280230025758,0.,0.781200482846104));
#51461=DIRECTION('ref_axis',(0.781200482846104,0.,0.624280230025758));
#51462=DIRECTION('',(0.,1.,0.));
#51463=DIRECTION('center_axis',(-0.988679578606275,0.,-0.150042296859647));
#51464=DIRECTION('ref_axis',(-0.150042296859647,0.,0.988679578606275));
#51465=DIRECTION('',(0.,1.,0.));
#51466=DIRECTION('center_axis',(-0.364399348580519,0.,-0.931242779705751));
#51467=DIRECTION('ref_axis',(-0.931242779705751,0.,0.364399348580519));
#51468=DIRECTION('',(0.,1.,0.));
#51469=DIRECTION('center_axis',(0.624280230025758,0.,-0.781200482846105));
#51470=DIRECTION('ref_axis',(-0.781200482846105,0.,-0.624280230025758));
#51471=DIRECTION('center_axis',(0.988679578606276,0.,0.150042296859641));
#51472=DIRECTION('ref_axis',(0.150042296859641,0.,-0.988679578606276));
#51473=DIRECTION('',(0.,1.,0.));
#51474=DIRECTION('',(0.,1.,0.));
#51475=DIRECTION('center_axis',(0.364399348580517,0.,0.931242779705752));
#51476=DIRECTION('ref_axis',(0.931242779705752,0.,-0.364399348580517));
#51477=DIRECTION('',(0.,1.,0.));
#51478=DIRECTION('center_axis',(-0.624280230025758,0.,0.781200482846104));
#51479=DIRECTION('ref_axis',(0.781200482846104,0.,0.624280230025758));
#51480=DIRECTION('',(0.,1.,0.));
#51481=DIRECTION('center_axis',(-0.988679578606275,0.,-0.150042296859647));
#51482=DIRECTION('ref_axis',(-0.150042296859647,0.,0.988679578606275));
#51483=DIRECTION('',(0.,1.,0.));
#51484=DIRECTION('center_axis',(-0.364399348580519,0.,-0.931242779705751));
#51485=DIRECTION('ref_axis',(-0.931242779705751,0.,0.364399348580519));
#51486=DIRECTION('',(0.,1.,0.));
#51487=DIRECTION('center_axis',(0.624280230025758,0.,-0.781200482846105));
#51488=DIRECTION('ref_axis',(-0.781200482846105,0.,-0.624280230025758));
#51489=DIRECTION('center_axis',(0.988679578606276,0.,0.150042296859641));
#51490=DIRECTION('ref_axis',(0.150042296859641,0.,-0.988679578606276));
#51491=DIRECTION('',(0.,1.,0.));
#51492=DIRECTION('',(0.,1.,0.));
#51493=DIRECTION('center_axis',(0.364399348580517,0.,0.931242779705752));
#51494=DIRECTION('ref_axis',(0.931242779705752,0.,-0.364399348580517));
#51495=DIRECTION('',(0.,1.,0.));
#51496=DIRECTION('center_axis',(-0.624280230025758,0.,0.781200482846104));
#51497=DIRECTION('ref_axis',(0.781200482846104,0.,0.624280230025758));
#51498=DIRECTION('',(0.,1.,0.));
#51499=DIRECTION('center_axis',(-0.988679578606275,0.,-0.150042296859647));
#51500=DIRECTION('ref_axis',(-0.150042296859647,0.,0.988679578606275));
#51501=DIRECTION('',(0.,1.,0.));
#51502=DIRECTION('center_axis',(-0.364399348580519,0.,-0.931242779705751));
#51503=DIRECTION('ref_axis',(-0.931242779705751,0.,0.364399348580519));
#51504=DIRECTION('',(0.,1.,0.));
#51505=DIRECTION('center_axis',(0.624280230025758,0.,-0.781200482846105));
#51506=DIRECTION('ref_axis',(-0.781200482846105,0.,-0.624280230025758));
#51507=DIRECTION('center_axis',(0.988679578606276,0.,0.150042296859641));
#51508=DIRECTION('ref_axis',(0.150042296859641,0.,-0.988679578606276));
#51509=DIRECTION('',(0.,1.,0.));
#51510=DIRECTION('',(0.,1.,0.));
#51511=DIRECTION('center_axis',(0.364399348580517,0.,0.931242779705752));
#51512=DIRECTION('ref_axis',(0.931242779705752,0.,-0.364399348580517));
#51513=DIRECTION('',(0.,1.,0.));
#51514=DIRECTION('center_axis',(-0.624280230025758,0.,0.781200482846104));
#51515=DIRECTION('ref_axis',(0.781200482846104,0.,0.624280230025758));
#51516=DIRECTION('',(0.,1.,0.));
#51517=DIRECTION('center_axis',(-0.988679578606275,0.,-0.150042296859647));
#51518=DIRECTION('ref_axis',(-0.150042296859647,0.,0.988679578606275));
#51519=DIRECTION('',(0.,1.,0.));
#51520=DIRECTION('center_axis',(-0.364399348580519,0.,-0.931242779705751));
#51521=DIRECTION('ref_axis',(-0.931242779705751,0.,0.364399348580519));
#51522=DIRECTION('',(0.,1.,0.));
#51523=DIRECTION('center_axis',(0.624280230025758,0.,-0.781200482846105));
#51524=DIRECTION('ref_axis',(-0.781200482846105,0.,-0.624280230025758));
#51525=DIRECTION('center_axis',(0.988679578606276,0.,0.150042296859641));
#51526=DIRECTION('ref_axis',(0.150042296859641,0.,-0.988679578606276));
#51527=DIRECTION('',(0.,1.,0.));
#51528=DIRECTION('',(0.,1.,0.));
#51529=DIRECTION('center_axis',(0.364399348580517,0.,0.931242779705752));
#51530=DIRECTION('ref_axis',(0.931242779705752,0.,-0.364399348580517));
#51531=DIRECTION('',(0.,1.,0.));
#51532=DIRECTION('center_axis',(-0.624280230025758,0.,0.781200482846104));
#51533=DIRECTION('ref_axis',(0.781200482846104,0.,0.624280230025758));
#51534=DIRECTION('',(0.,1.,0.));
#51535=DIRECTION('center_axis',(-0.988679578606275,0.,-0.150042296859647));
#51536=DIRECTION('ref_axis',(-0.150042296859647,0.,0.988679578606275));
#51537=DIRECTION('',(0.,1.,0.));
#51538=DIRECTION('center_axis',(-0.364399348580519,0.,-0.931242779705751));
#51539=DIRECTION('ref_axis',(-0.931242779705751,0.,0.364399348580519));
#51540=DIRECTION('',(0.,1.,0.));
#51541=DIRECTION('center_axis',(0.624280230025758,0.,-0.781200482846105));
#51542=DIRECTION('ref_axis',(-0.781200482846105,0.,-0.624280230025758));
#51543=DIRECTION('center_axis',(0.988679578606276,0.,0.150042296859641));
#51544=DIRECTION('ref_axis',(0.150042296859641,0.,-0.988679578606276));
#51545=DIRECTION('',(0.,1.,0.));
#51546=DIRECTION('',(0.,1.,0.));
#51547=DIRECTION('center_axis',(0.364399348580517,0.,0.931242779705752));
#51548=DIRECTION('ref_axis',(0.931242779705752,0.,-0.364399348580517));
#51549=DIRECTION('',(0.,1.,0.));
#51550=DIRECTION('center_axis',(-0.624280230025758,0.,0.781200482846104));
#51551=DIRECTION('ref_axis',(0.781200482846104,0.,0.624280230025758));
#51552=DIRECTION('',(0.,1.,0.));
#51553=DIRECTION('center_axis',(-0.988679578606275,0.,-0.150042296859647));
#51554=DIRECTION('ref_axis',(-0.150042296859647,0.,0.988679578606275));
#51555=DIRECTION('',(0.,1.,0.));
#51556=DIRECTION('center_axis',(-0.364399348580519,0.,-0.931242779705751));
#51557=DIRECTION('ref_axis',(-0.931242779705751,0.,0.364399348580519));
#51558=DIRECTION('',(0.,1.,0.));
#51559=DIRECTION('center_axis',(0.624280230025758,0.,-0.781200482846105));
#51560=DIRECTION('ref_axis',(-0.781200482846105,0.,-0.624280230025758));
#51561=DIRECTION('center_axis',(0.988679578606276,0.,0.150042296859641));
#51562=DIRECTION('ref_axis',(0.150042296859641,0.,-0.988679578606276));
#51563=DIRECTION('',(0.,1.,0.));
#51564=DIRECTION('',(0.,1.,0.));
#51565=DIRECTION('center_axis',(0.364399348580517,0.,0.931242779705752));
#51566=DIRECTION('ref_axis',(0.931242779705752,0.,-0.364399348580517));
#51567=DIRECTION('',(0.,1.,0.));
#51568=DIRECTION('center_axis',(-0.624280230025758,0.,0.781200482846104));
#51569=DIRECTION('ref_axis',(0.781200482846104,0.,0.624280230025758));
#51570=DIRECTION('',(0.,1.,0.));
#51571=DIRECTION('center_axis',(-0.988679578606275,0.,-0.150042296859647));
#51572=DIRECTION('ref_axis',(-0.150042296859647,0.,0.988679578606275));
#51573=DIRECTION('',(0.,1.,0.));
#51574=DIRECTION('center_axis',(-0.364399348580519,0.,-0.931242779705751));
#51575=DIRECTION('ref_axis',(-0.931242779705751,0.,0.364399348580519));
#51576=DIRECTION('',(0.,1.,0.));
#51577=DIRECTION('center_axis',(0.624280230025758,0.,-0.781200482846105));
#51578=DIRECTION('ref_axis',(-0.781200482846105,0.,-0.624280230025758));
#51579=DIRECTION('center_axis',(0.988679578606276,0.,0.150042296859641));
#51580=DIRECTION('ref_axis',(0.150042296859641,0.,-0.988679578606276));
#51581=DIRECTION('',(0.,1.,0.));
#51582=DIRECTION('',(0.,1.,0.));
#51583=DIRECTION('center_axis',(0.364399348580517,0.,0.931242779705752));
#51584=DIRECTION('ref_axis',(0.931242779705752,0.,-0.364399348580517));
#51585=DIRECTION('',(0.,1.,0.));
#51586=DIRECTION('center_axis',(-0.624280230025758,0.,0.781200482846104));
#51587=DIRECTION('ref_axis',(0.781200482846104,0.,0.624280230025758));
#51588=DIRECTION('',(0.,1.,0.));
#51589=DIRECTION('center_axis',(-0.988679578606275,0.,-0.150042296859647));
#51590=DIRECTION('ref_axis',(-0.150042296859647,0.,0.988679578606275));
#51591=DIRECTION('',(0.,1.,0.));
#51592=DIRECTION('center_axis',(-0.364399348580519,0.,-0.931242779705751));
#51593=DIRECTION('ref_axis',(-0.931242779705751,0.,0.364399348580519));
#51594=DIRECTION('',(0.,1.,0.));
#51595=DIRECTION('center_axis',(0.624280230025758,0.,-0.781200482846105));
#51596=DIRECTION('ref_axis',(-0.781200482846105,0.,-0.624280230025758));
#51597=DIRECTION('center_axis',(0.988679578606276,0.,0.150042296859641));
#51598=DIRECTION('ref_axis',(0.150042296859641,0.,-0.988679578606276));
#51599=DIRECTION('',(0.,1.,0.));
#51600=DIRECTION('',(0.,1.,0.));
#51601=DIRECTION('center_axis',(0.364399348580517,0.,0.931242779705752));
#51602=DIRECTION('ref_axis',(0.931242779705752,0.,-0.364399348580517));
#51603=DIRECTION('',(0.,1.,0.));
#51604=DIRECTION('center_axis',(-0.624280230025758,0.,0.781200482846104));
#51605=DIRECTION('ref_axis',(0.781200482846104,0.,0.624280230025758));
#51606=DIRECTION('',(0.,1.,0.));
#51607=DIRECTION('center_axis',(-0.988679578606275,0.,-0.150042296859647));
#51608=DIRECTION('ref_axis',(-0.150042296859647,0.,0.988679578606275));
#51609=DIRECTION('',(0.,1.,0.));
#51610=DIRECTION('center_axis',(-0.364399348580519,0.,-0.931242779705751));
#51611=DIRECTION('ref_axis',(-0.931242779705751,0.,0.364399348580519));
#51612=DIRECTION('',(0.,1.,0.));
#51613=DIRECTION('center_axis',(0.624280230025758,0.,-0.781200482846105));
#51614=DIRECTION('ref_axis',(-0.781200482846105,0.,-0.624280230025758));
#51615=DIRECTION('center_axis',(0.988679578606276,0.,0.150042296859641));
#51616=DIRECTION('ref_axis',(0.150042296859641,0.,-0.988679578606276));
#51617=DIRECTION('',(0.,1.,0.));
#51618=DIRECTION('',(0.,1.,0.));
#51619=DIRECTION('center_axis',(0.364399348580517,0.,0.931242779705752));
#51620=DIRECTION('ref_axis',(0.931242779705752,0.,-0.364399348580517));
#51621=DIRECTION('',(0.,1.,0.));
#51622=DIRECTION('center_axis',(-0.624280230025758,0.,0.781200482846104));
#51623=DIRECTION('ref_axis',(0.781200482846104,0.,0.624280230025758));
#51624=DIRECTION('',(0.,1.,0.));
#51625=DIRECTION('center_axis',(-0.988679578606275,0.,-0.150042296859647));
#51626=DIRECTION('ref_axis',(-0.150042296859647,0.,0.988679578606275));
#51627=DIRECTION('',(0.,1.,0.));
#51628=DIRECTION('center_axis',(-0.364399348580519,0.,-0.931242779705751));
#51629=DIRECTION('ref_axis',(-0.931242779705751,0.,0.364399348580519));
#51630=DIRECTION('',(0.,1.,0.));
#51631=DIRECTION('center_axis',(0.624280230025758,0.,-0.781200482846105));
#51632=DIRECTION('ref_axis',(-0.781200482846105,0.,-0.624280230025758));
#51633=DIRECTION('center_axis',(0.988679578606276,0.,0.150042296859641));
#51634=DIRECTION('ref_axis',(0.150042296859641,0.,-0.988679578606276));
#51635=DIRECTION('',(0.,1.,0.));
#51636=DIRECTION('',(0.,1.,0.));
#51637=DIRECTION('center_axis',(0.364399348580517,0.,0.931242779705752));
#51638=DIRECTION('ref_axis',(0.931242779705752,0.,-0.364399348580517));
#51639=DIRECTION('',(0.,1.,0.));
#51640=DIRECTION('center_axis',(-0.624280230025758,0.,0.781200482846104));
#51641=DIRECTION('ref_axis',(0.781200482846104,0.,0.624280230025758));
#51642=DIRECTION('',(0.,1.,0.));
#51643=DIRECTION('center_axis',(-0.988679578606275,0.,-0.150042296859647));
#51644=DIRECTION('ref_axis',(-0.150042296859647,0.,0.988679578606275));
#51645=DIRECTION('',(0.,1.,0.));
#51646=DIRECTION('center_axis',(-0.364399348580519,0.,-0.931242779705751));
#51647=DIRECTION('ref_axis',(-0.931242779705751,0.,0.364399348580519));
#51648=DIRECTION('',(0.,1.,0.));
#51649=DIRECTION('center_axis',(0.624280230025758,0.,-0.781200482846105));
#51650=DIRECTION('ref_axis',(-0.781200482846105,0.,-0.624280230025758));
#51651=DIRECTION('center_axis',(0.988679578606276,0.,0.150042296859641));
#51652=DIRECTION('ref_axis',(0.150042296859641,0.,-0.988679578606276));
#51653=DIRECTION('',(0.,1.,0.));
#51654=DIRECTION('',(0.,1.,0.));
#51655=DIRECTION('center_axis',(0.364399348580517,0.,0.931242779705752));
#51656=DIRECTION('ref_axis',(0.931242779705752,0.,-0.364399348580517));
#51657=DIRECTION('',(0.,1.,0.));
#51658=DIRECTION('center_axis',(-0.624280230025758,0.,0.781200482846104));
#51659=DIRECTION('ref_axis',(0.781200482846104,0.,0.624280230025758));
#51660=DIRECTION('',(0.,1.,0.));
#51661=DIRECTION('center_axis',(-0.988679578606275,0.,-0.150042296859647));
#51662=DIRECTION('ref_axis',(-0.150042296859647,0.,0.988679578606275));
#51663=DIRECTION('',(0.,1.,0.));
#51664=DIRECTION('center_axis',(-0.364399348580519,0.,-0.931242779705751));
#51665=DIRECTION('ref_axis',(-0.931242779705751,0.,0.364399348580519));
#51666=DIRECTION('',(0.,1.,0.));
#51667=DIRECTION('center_axis',(0.624280230025758,0.,-0.781200482846105));
#51668=DIRECTION('ref_axis',(-0.781200482846105,0.,-0.624280230025758));
#51669=DIRECTION('center_axis',(0.988679578606276,0.,0.150042296859641));
#51670=DIRECTION('ref_axis',(0.150042296859641,0.,-0.988679578606276));
#51671=DIRECTION('',(0.,1.,0.));
#51672=DIRECTION('',(0.,1.,0.));
#51673=DIRECTION('center_axis',(0.364399348580517,0.,0.931242779705752));
#51674=DIRECTION('ref_axis',(0.931242779705752,0.,-0.364399348580517));
#51675=DIRECTION('',(0.,1.,0.));
#51676=DIRECTION('center_axis',(-0.624280230025758,0.,0.781200482846104));
#51677=DIRECTION('ref_axis',(0.781200482846104,0.,0.624280230025758));
#51678=DIRECTION('',(0.,1.,0.));
#51679=DIRECTION('center_axis',(-0.988679578606275,0.,-0.150042296859647));
#51680=DIRECTION('ref_axis',(-0.150042296859647,0.,0.988679578606275));
#51681=DIRECTION('',(0.,1.,0.));
#51682=DIRECTION('center_axis',(-0.364399348580519,0.,-0.931242779705751));
#51683=DIRECTION('ref_axis',(-0.931242779705751,0.,0.364399348580519));
#51684=DIRECTION('',(0.,1.,0.));
#51685=DIRECTION('center_axis',(0.624280230025758,0.,-0.781200482846105));
#51686=DIRECTION('ref_axis',(-0.781200482846105,0.,-0.624280230025758));
#51687=DIRECTION('center_axis',(0.988679578606276,0.,0.150042296859641));
#51688=DIRECTION('ref_axis',(0.150042296859641,0.,-0.988679578606276));
#51689=DIRECTION('',(0.,1.,0.));
#51690=DIRECTION('',(0.,1.,0.));
#51691=DIRECTION('center_axis',(0.364399348580517,0.,0.931242779705752));
#51692=DIRECTION('ref_axis',(0.931242779705752,0.,-0.364399348580517));
#51693=DIRECTION('',(0.,1.,0.));
#51694=DIRECTION('center_axis',(-0.624280230025758,0.,0.781200482846104));
#51695=DIRECTION('ref_axis',(0.781200482846104,0.,0.624280230025758));
#51696=DIRECTION('',(0.,1.,0.));
#51697=DIRECTION('center_axis',(-0.988679578606275,0.,-0.150042296859647));
#51698=DIRECTION('ref_axis',(-0.150042296859647,0.,0.988679578606275));
#51699=DIRECTION('',(0.,1.,0.));
#51700=DIRECTION('center_axis',(-0.364399348580519,0.,-0.931242779705751));
#51701=DIRECTION('ref_axis',(-0.931242779705751,0.,0.364399348580519));
#51702=DIRECTION('',(0.,1.,0.));
#51703=DIRECTION('center_axis',(0.624280230025758,0.,-0.781200482846105));
#51704=DIRECTION('ref_axis',(-0.781200482846105,0.,-0.624280230025758));
#51705=DIRECTION('center_axis',(0.988679578606276,0.,0.150042296859641));
#51706=DIRECTION('ref_axis',(0.150042296859641,0.,-0.988679578606276));
#51707=DIRECTION('',(0.,1.,0.));
#51708=DIRECTION('',(0.,1.,0.));
#51709=DIRECTION('center_axis',(0.364399348580517,0.,0.931242779705752));
#51710=DIRECTION('ref_axis',(0.931242779705752,0.,-0.364399348580517));
#51711=DIRECTION('',(0.,1.,0.));
#51712=DIRECTION('center_axis',(-0.624280230025758,0.,0.781200482846104));
#51713=DIRECTION('ref_axis',(0.781200482846104,0.,0.624280230025758));
#51714=DIRECTION('',(0.,1.,0.));
#51715=DIRECTION('center_axis',(-0.988679578606275,0.,-0.150042296859647));
#51716=DIRECTION('ref_axis',(-0.150042296859647,0.,0.988679578606275));
#51717=DIRECTION('',(0.,1.,0.));
#51718=DIRECTION('center_axis',(-0.364399348580519,0.,-0.931242779705751));
#51719=DIRECTION('ref_axis',(-0.931242779705751,0.,0.364399348580519));
#51720=DIRECTION('',(0.,1.,0.));
#51721=DIRECTION('center_axis',(0.624280230025758,0.,-0.781200482846105));
#51722=DIRECTION('ref_axis',(-0.781200482846105,0.,-0.624280230025758));
#51723=DIRECTION('center_axis',(0.988679578606276,0.,0.150042296859641));
#51724=DIRECTION('ref_axis',(0.150042296859641,0.,-0.988679578606276));
#51725=DIRECTION('',(0.,1.,0.));
#51726=DIRECTION('',(0.,1.,0.));
#51727=DIRECTION('center_axis',(0.364399348580517,0.,0.931242779705752));
#51728=DIRECTION('ref_axis',(0.931242779705752,0.,-0.364399348580517));
#51729=DIRECTION('',(0.,1.,0.));
#51730=DIRECTION('center_axis',(-0.624280230025758,0.,0.781200482846104));
#51731=DIRECTION('ref_axis',(0.781200482846104,0.,0.624280230025758));
#51732=DIRECTION('',(0.,1.,0.));
#51733=DIRECTION('center_axis',(-0.988679578606275,0.,-0.150042296859647));
#51734=DIRECTION('ref_axis',(-0.150042296859647,0.,0.988679578606275));
#51735=DIRECTION('',(0.,1.,0.));
#51736=DIRECTION('center_axis',(-0.364399348580519,0.,-0.931242779705751));
#51737=DIRECTION('ref_axis',(-0.931242779705751,0.,0.364399348580519));
#51738=DIRECTION('',(0.,1.,0.));
#51739=DIRECTION('center_axis',(0.624280230025758,0.,-0.781200482846105));
#51740=DIRECTION('ref_axis',(-0.781200482846105,0.,-0.624280230025758));
#51741=DIRECTION('center_axis',(0.988679578606276,0.,0.150042296859641));
#51742=DIRECTION('ref_axis',(0.150042296859641,0.,-0.988679578606276));
#51743=DIRECTION('',(0.,1.,0.));
#51744=DIRECTION('',(0.,1.,0.));
#51745=DIRECTION('center_axis',(0.364399348580517,0.,0.931242779705752));
#51746=DIRECTION('ref_axis',(0.931242779705752,0.,-0.364399348580517));
#51747=DIRECTION('',(0.,1.,0.));
#51748=DIRECTION('center_axis',(-0.624280230025758,0.,0.781200482846104));
#51749=DIRECTION('ref_axis',(0.781200482846104,0.,0.624280230025758));
#51750=DIRECTION('',(0.,1.,0.));
#51751=DIRECTION('center_axis',(-0.988679578606275,0.,-0.150042296859647));
#51752=DIRECTION('ref_axis',(-0.150042296859647,0.,0.988679578606275));
#51753=DIRECTION('',(0.,1.,0.));
#51754=DIRECTION('center_axis',(-0.364399348580519,0.,-0.931242779705751));
#51755=DIRECTION('ref_axis',(-0.931242779705751,0.,0.364399348580519));
#51756=DIRECTION('',(0.,1.,0.));
#51757=DIRECTION('center_axis',(0.624280230025758,0.,-0.781200482846105));
#51758=DIRECTION('ref_axis',(-0.781200482846105,0.,-0.624280230025758));
#51759=DIRECTION('center_axis',(0.988679578606276,0.,0.150042296859641));
#51760=DIRECTION('ref_axis',(0.150042296859641,0.,-0.988679578606276));
#51761=DIRECTION('',(0.,1.,0.));
#51762=DIRECTION('',(0.,1.,0.));
#51763=DIRECTION('center_axis',(0.364399348580517,0.,0.931242779705752));
#51764=DIRECTION('ref_axis',(0.931242779705752,0.,-0.364399348580517));
#51765=DIRECTION('',(0.,1.,0.));
#51766=DIRECTION('center_axis',(-0.624280230025758,0.,0.781200482846104));
#51767=DIRECTION('ref_axis',(0.781200482846104,0.,0.624280230025758));
#51768=DIRECTION('',(0.,1.,0.));
#51769=DIRECTION('center_axis',(-0.988679578606275,0.,-0.150042296859647));
#51770=DIRECTION('ref_axis',(-0.150042296859647,0.,0.988679578606275));
#51771=DIRECTION('',(0.,1.,0.));
#51772=DIRECTION('center_axis',(-0.364399348580519,0.,-0.931242779705751));
#51773=DIRECTION('ref_axis',(-0.931242779705751,0.,0.364399348580519));
#51774=DIRECTION('',(0.,1.,0.));
#51775=DIRECTION('center_axis',(0.624280230025758,0.,-0.781200482846105));
#51776=DIRECTION('ref_axis',(-0.781200482846105,0.,-0.624280230025758));
#51777=DIRECTION('center_axis',(0.988679578606276,0.,0.150042296859641));
#51778=DIRECTION('ref_axis',(0.150042296859641,0.,-0.988679578606276));
#51779=DIRECTION('',(0.,1.,0.));
#51780=DIRECTION('',(0.,1.,0.));
#51781=DIRECTION('center_axis',(0.364399348580517,0.,0.931242779705752));
#51782=DIRECTION('ref_axis',(0.931242779705752,0.,-0.364399348580517));
#51783=DIRECTION('',(0.,1.,0.));
#51784=DIRECTION('center_axis',(-0.624280230025758,0.,0.781200482846104));
#51785=DIRECTION('ref_axis',(0.781200482846104,0.,0.624280230025758));
#51786=DIRECTION('',(0.,1.,0.));
#51787=DIRECTION('center_axis',(-0.988679578606275,0.,-0.150042296859647));
#51788=DIRECTION('ref_axis',(-0.150042296859647,0.,0.988679578606275));
#51789=DIRECTION('',(0.,1.,0.));
#51790=DIRECTION('center_axis',(-0.364399348580519,0.,-0.931242779705751));
#51791=DIRECTION('ref_axis',(-0.931242779705751,0.,0.364399348580519));
#51792=DIRECTION('',(0.,1.,0.));
#51793=DIRECTION('center_axis',(0.624280230025758,0.,-0.781200482846105));
#51794=DIRECTION('ref_axis',(-0.781200482846105,0.,-0.624280230025758));
#51795=DIRECTION('center_axis',(0.988679578606276,0.,0.150042296859641));
#51796=DIRECTION('ref_axis',(0.150042296859641,0.,-0.988679578606276));
#51797=DIRECTION('',(0.,1.,0.));
#51798=DIRECTION('',(0.,1.,0.));
#51799=DIRECTION('center_axis',(0.364399348580517,0.,0.931242779705752));
#51800=DIRECTION('ref_axis',(0.931242779705752,0.,-0.364399348580517));
#51801=DIRECTION('',(0.,1.,0.));
#51802=DIRECTION('center_axis',(-0.624280230025758,0.,0.781200482846104));
#51803=DIRECTION('ref_axis',(0.781200482846104,0.,0.624280230025758));
#51804=DIRECTION('',(0.,1.,0.));
#51805=DIRECTION('center_axis',(-0.988679578606275,0.,-0.150042296859647));
#51806=DIRECTION('ref_axis',(-0.150042296859647,0.,0.988679578606275));
#51807=DIRECTION('',(0.,1.,0.));
#51808=DIRECTION('center_axis',(-0.364399348580519,0.,-0.931242779705751));
#51809=DIRECTION('ref_axis',(-0.931242779705751,0.,0.364399348580519));
#51810=DIRECTION('',(0.,1.,0.));
#51811=DIRECTION('center_axis',(0.624280230025758,0.,-0.781200482846105));
#51812=DIRECTION('ref_axis',(-0.781200482846105,0.,-0.624280230025758));
#51813=DIRECTION('center_axis',(0.988679578606276,0.,0.150042296859641));
#51814=DIRECTION('ref_axis',(0.150042296859641,0.,-0.988679578606276));
#51815=DIRECTION('',(0.,1.,0.));
#51816=DIRECTION('',(0.,1.,0.));
#51817=DIRECTION('center_axis',(0.364399348580517,0.,0.931242779705752));
#51818=DIRECTION('ref_axis',(0.931242779705752,0.,-0.364399348580517));
#51819=DIRECTION('',(0.,1.,0.));
#51820=DIRECTION('center_axis',(-0.624280230025758,0.,0.781200482846104));
#51821=DIRECTION('ref_axis',(0.781200482846104,0.,0.624280230025758));
#51822=DIRECTION('',(0.,1.,0.));
#51823=DIRECTION('center_axis',(-0.988679578606275,0.,-0.150042296859647));
#51824=DIRECTION('ref_axis',(-0.150042296859647,0.,0.988679578606275));
#51825=DIRECTION('',(0.,1.,0.));
#51826=DIRECTION('center_axis',(-0.364399348580519,0.,-0.931242779705751));
#51827=DIRECTION('ref_axis',(-0.931242779705751,0.,0.364399348580519));
#51828=DIRECTION('',(0.,1.,0.));
#51829=DIRECTION('center_axis',(0.624280230025758,0.,-0.781200482846105));
#51830=DIRECTION('ref_axis',(-0.781200482846105,0.,-0.624280230025758));
#51831=DIRECTION('center_axis',(0.988679578606276,0.,0.150042296859641));
#51832=DIRECTION('ref_axis',(0.150042296859641,0.,-0.988679578606276));
#51833=DIRECTION('',(0.,1.,0.));
#51834=DIRECTION('',(0.,1.,0.));
#51835=DIRECTION('center_axis',(0.364399348580517,0.,0.931242779705752));
#51836=DIRECTION('ref_axis',(0.931242779705752,0.,-0.364399348580517));
#51837=DIRECTION('',(0.,1.,0.));
#51838=DIRECTION('center_axis',(-0.624280230025758,0.,0.781200482846104));
#51839=DIRECTION('ref_axis',(0.781200482846104,0.,0.624280230025758));
#51840=DIRECTION('',(0.,1.,0.));
#51841=DIRECTION('center_axis',(-0.988679578606275,0.,-0.150042296859647));
#51842=DIRECTION('ref_axis',(-0.150042296859647,0.,0.988679578606275));
#51843=DIRECTION('',(0.,1.,0.));
#51844=DIRECTION('center_axis',(-0.364399348580519,0.,-0.931242779705751));
#51845=DIRECTION('ref_axis',(-0.931242779705751,0.,0.364399348580519));
#51846=DIRECTION('',(0.,1.,0.));
#51847=DIRECTION('center_axis',(0.624280230025758,0.,-0.781200482846105));
#51848=DIRECTION('ref_axis',(-0.781200482846105,0.,-0.624280230025758));
#51849=DIRECTION('center_axis',(0.988679578606276,0.,0.150042296859641));
#51850=DIRECTION('ref_axis',(0.150042296859641,0.,-0.988679578606276));
#51851=DIRECTION('',(0.,1.,0.));
#51852=DIRECTION('',(0.,1.,0.));
#51853=DIRECTION('center_axis',(0.364399348580517,0.,0.931242779705752));
#51854=DIRECTION('ref_axis',(0.931242779705752,0.,-0.364399348580517));
#51855=DIRECTION('',(0.,1.,0.));
#51856=DIRECTION('center_axis',(-0.624280230025758,0.,0.781200482846104));
#51857=DIRECTION('ref_axis',(0.781200482846104,0.,0.624280230025758));
#51858=DIRECTION('',(0.,1.,0.));
#51859=DIRECTION('center_axis',(-0.988679578606275,0.,-0.150042296859647));
#51860=DIRECTION('ref_axis',(-0.150042296859647,0.,0.988679578606275));
#51861=DIRECTION('',(0.,1.,0.));
#51862=DIRECTION('center_axis',(-0.364399348580519,0.,-0.931242779705751));
#51863=DIRECTION('ref_axis',(-0.931242779705751,0.,0.364399348580519));
#51864=DIRECTION('',(0.,1.,0.));
#51865=DIRECTION('center_axis',(0.624280230025758,0.,-0.781200482846105));
#51866=DIRECTION('ref_axis',(-0.781200482846105,0.,-0.624280230025758));
#51867=DIRECTION('center_axis',(0.988679578606276,0.,0.150042296859641));
#51868=DIRECTION('ref_axis',(0.150042296859641,0.,-0.988679578606276));
#51869=DIRECTION('',(0.,1.,0.));
#51870=DIRECTION('',(0.,1.,0.));
#51871=DIRECTION('center_axis',(0.364399348580517,0.,0.931242779705752));
#51872=DIRECTION('ref_axis',(0.931242779705752,0.,-0.364399348580517));
#51873=DIRECTION('',(0.,1.,0.));
#51874=DIRECTION('center_axis',(-0.624280230025758,0.,0.781200482846104));
#51875=DIRECTION('ref_axis',(0.781200482846104,0.,0.624280230025758));
#51876=DIRECTION('',(0.,1.,0.));
#51877=DIRECTION('center_axis',(-0.988679578606275,0.,-0.150042296859647));
#51878=DIRECTION('ref_axis',(-0.150042296859647,0.,0.988679578606275));
#51879=DIRECTION('',(0.,1.,0.));
#51880=DIRECTION('center_axis',(-0.364399348580519,0.,-0.931242779705751));
#51881=DIRECTION('ref_axis',(-0.931242779705751,0.,0.364399348580519));
#51882=DIRECTION('',(0.,1.,0.));
#51883=DIRECTION('center_axis',(0.624280230025758,0.,-0.781200482846105));
#51884=DIRECTION('ref_axis',(-0.781200482846105,0.,-0.624280230025758));
#51885=DIRECTION('center_axis',(0.988679578606276,0.,0.150042296859641));
#51886=DIRECTION('ref_axis',(0.150042296859641,0.,-0.988679578606276));
#51887=DIRECTION('',(0.,1.,0.));
#51888=DIRECTION('',(0.,1.,0.));
#51889=DIRECTION('center_axis',(0.364399348580517,0.,0.931242779705752));
#51890=DIRECTION('ref_axis',(0.931242779705752,0.,-0.364399348580517));
#51891=DIRECTION('',(0.,1.,0.));
#51892=DIRECTION('center_axis',(-0.624280230025758,0.,0.781200482846104));
#51893=DIRECTION('ref_axis',(0.781200482846104,0.,0.624280230025758));
#51894=DIRECTION('',(0.,1.,0.));
#51895=DIRECTION('center_axis',(-0.988679578606275,0.,-0.150042296859647));
#51896=DIRECTION('ref_axis',(-0.150042296859647,0.,0.988679578606275));
#51897=DIRECTION('',(0.,1.,0.));
#51898=DIRECTION('center_axis',(-0.364399348580519,0.,-0.931242779705751));
#51899=DIRECTION('ref_axis',(-0.931242779705751,0.,0.364399348580519));
#51900=DIRECTION('',(0.,1.,0.));
#51901=DIRECTION('center_axis',(0.624280230025758,0.,-0.781200482846105));
#51902=DIRECTION('ref_axis',(-0.781200482846105,0.,-0.624280230025758));
#51903=DIRECTION('center_axis',(0.988679578606276,0.,0.150042296859641));
#51904=DIRECTION('ref_axis',(0.150042296859641,0.,-0.988679578606276));
#51905=DIRECTION('',(0.,1.,0.));
#51906=DIRECTION('',(0.,1.,0.));
#51907=DIRECTION('center_axis',(0.364399348580517,0.,0.931242779705752));
#51908=DIRECTION('ref_axis',(0.931242779705752,0.,-0.364399348580517));
#51909=DIRECTION('',(0.,1.,0.));
#51910=DIRECTION('center_axis',(-0.624280230025758,0.,0.781200482846104));
#51911=DIRECTION('ref_axis',(0.781200482846104,0.,0.624280230025758));
#51912=DIRECTION('',(0.,1.,0.));
#51913=DIRECTION('center_axis',(-0.988679578606275,0.,-0.150042296859647));
#51914=DIRECTION('ref_axis',(-0.150042296859647,0.,0.988679578606275));
#51915=DIRECTION('',(0.,1.,0.));
#51916=DIRECTION('center_axis',(-0.364399348580519,0.,-0.931242779705751));
#51917=DIRECTION('ref_axis',(-0.931242779705751,0.,0.364399348580519));
#51918=DIRECTION('',(0.,1.,0.));
#51919=DIRECTION('center_axis',(0.624280230025758,0.,-0.781200482846105));
#51920=DIRECTION('ref_axis',(-0.781200482846105,0.,-0.624280230025758));
#51921=DIRECTION('center_axis',(0.988679578606276,0.,0.150042296859641));
#51922=DIRECTION('ref_axis',(0.150042296859641,0.,-0.988679578606276));
#51923=DIRECTION('',(0.,1.,0.));
#51924=DIRECTION('',(0.,1.,0.));
#51925=DIRECTION('center_axis',(0.364399348580517,0.,0.931242779705752));
#51926=DIRECTION('ref_axis',(0.931242779705752,0.,-0.364399348580517));
#51927=DIRECTION('',(0.,1.,0.));
#51928=DIRECTION('center_axis',(-0.624280230025758,0.,0.781200482846104));
#51929=DIRECTION('ref_axis',(0.781200482846104,0.,0.624280230025758));
#51930=DIRECTION('',(0.,1.,0.));
#51931=DIRECTION('center_axis',(-0.988679578606275,0.,-0.150042296859647));
#51932=DIRECTION('ref_axis',(-0.150042296859647,0.,0.988679578606275));
#51933=DIRECTION('',(0.,1.,0.));
#51934=DIRECTION('center_axis',(-0.364399348580519,0.,-0.931242779705751));
#51935=DIRECTION('ref_axis',(-0.931242779705751,0.,0.364399348580519));
#51936=DIRECTION('',(0.,1.,0.));
#51937=DIRECTION('center_axis',(0.624280230025758,0.,-0.781200482846105));
#51938=DIRECTION('ref_axis',(-0.781200482846105,0.,-0.624280230025758));
#51939=DIRECTION('center_axis',(0.988679578606276,0.,0.150042296859641));
#51940=DIRECTION('ref_axis',(0.150042296859641,0.,-0.988679578606276));
#51941=DIRECTION('',(0.,1.,0.));
#51942=DIRECTION('',(0.,1.,0.));
#51943=DIRECTION('center_axis',(0.364399348580517,0.,0.931242779705752));
#51944=DIRECTION('ref_axis',(0.931242779705752,0.,-0.364399348580517));
#51945=DIRECTION('',(0.,1.,0.));
#51946=DIRECTION('center_axis',(-0.624280230025758,0.,0.781200482846104));
#51947=DIRECTION('ref_axis',(0.781200482846104,0.,0.624280230025758));
#51948=DIRECTION('',(0.,1.,0.));
#51949=DIRECTION('center_axis',(-0.988679578606275,0.,-0.150042296859647));
#51950=DIRECTION('ref_axis',(-0.150042296859647,0.,0.988679578606275));
#51951=DIRECTION('',(0.,1.,0.));
#51952=DIRECTION('center_axis',(-0.364399348580519,0.,-0.931242779705751));
#51953=DIRECTION('ref_axis',(-0.931242779705751,0.,0.364399348580519));
#51954=DIRECTION('',(0.,1.,0.));
#51955=DIRECTION('center_axis',(0.624280230025758,0.,-0.781200482846105));
#51956=DIRECTION('ref_axis',(-0.781200482846105,0.,-0.624280230025758));
#51957=DIRECTION('center_axis',(0.988679578606276,0.,0.150042296859641));
#51958=DIRECTION('ref_axis',(0.150042296859641,0.,-0.988679578606276));
#51959=DIRECTION('',(0.,1.,0.));
#51960=DIRECTION('',(0.,1.,0.));
#51961=DIRECTION('center_axis',(0.364399348580517,0.,0.931242779705752));
#51962=DIRECTION('ref_axis',(0.931242779705752,0.,-0.364399348580517));
#51963=DIRECTION('',(0.,1.,0.));
#51964=DIRECTION('center_axis',(-0.624280230025758,0.,0.781200482846104));
#51965=DIRECTION('ref_axis',(0.781200482846104,0.,0.624280230025758));
#51966=DIRECTION('',(0.,1.,0.));
#51967=DIRECTION('center_axis',(-0.988679578606275,0.,-0.150042296859647));
#51968=DIRECTION('ref_axis',(-0.150042296859647,0.,0.988679578606275));
#51969=DIRECTION('',(0.,1.,0.));
#51970=DIRECTION('center_axis',(-0.364399348580519,0.,-0.931242779705751));
#51971=DIRECTION('ref_axis',(-0.931242779705751,0.,0.364399348580519));
#51972=DIRECTION('',(0.,1.,0.));
#51973=DIRECTION('center_axis',(0.624280230025758,0.,-0.781200482846105));
#51974=DIRECTION('ref_axis',(-0.781200482846105,0.,-0.624280230025758));
#51975=DIRECTION('center_axis',(0.988679578606276,0.,0.150042296859641));
#51976=DIRECTION('ref_axis',(0.150042296859641,0.,-0.988679578606276));
#51977=DIRECTION('',(0.,1.,0.));
#51978=DIRECTION('',(0.,1.,0.));
#51979=DIRECTION('center_axis',(0.364399348580517,0.,0.931242779705752));
#51980=DIRECTION('ref_axis',(0.931242779705752,0.,-0.364399348580517));
#51981=DIRECTION('',(0.,1.,0.));
#51982=DIRECTION('center_axis',(-0.624280230025758,0.,0.781200482846104));
#51983=DIRECTION('ref_axis',(0.781200482846104,0.,0.624280230025758));
#51984=DIRECTION('',(0.,1.,0.));
#51985=DIRECTION('center_axis',(-0.988679578606275,0.,-0.150042296859647));
#51986=DIRECTION('ref_axis',(-0.150042296859647,0.,0.988679578606275));
#51987=DIRECTION('',(0.,1.,0.));
#51988=DIRECTION('center_axis',(-0.364399348580519,0.,-0.931242779705751));
#51989=DIRECTION('ref_axis',(-0.931242779705751,0.,0.364399348580519));
#51990=DIRECTION('',(0.,1.,0.));
#51991=DIRECTION('center_axis',(0.624280230025758,0.,-0.781200482846105));
#51992=DIRECTION('ref_axis',(-0.781200482846105,0.,-0.624280230025758));
#51993=DIRECTION('center_axis',(0.988679578606276,0.,0.150042296859641));
#51994=DIRECTION('ref_axis',(0.150042296859641,0.,-0.988679578606276));
#51995=DIRECTION('',(0.,1.,0.));
#51996=DIRECTION('',(0.,1.,0.));
#51997=DIRECTION('center_axis',(0.364399348580517,0.,0.931242779705752));
#51998=DIRECTION('ref_axis',(0.931242779705752,0.,-0.364399348580517));
#51999=DIRECTION('',(0.,1.,0.));
#52000=DIRECTION('center_axis',(-0.624280230025758,0.,0.781200482846104));
#52001=DIRECTION('ref_axis',(0.781200482846104,0.,0.624280230025758));
#52002=DIRECTION('',(0.,1.,0.));
#52003=DIRECTION('center_axis',(-0.988679578606275,0.,-0.150042296859647));
#52004=DIRECTION('ref_axis',(-0.150042296859647,0.,0.988679578606275));
#52005=DIRECTION('',(0.,1.,0.));
#52006=DIRECTION('center_axis',(-0.364399348580519,0.,-0.931242779705751));
#52007=DIRECTION('ref_axis',(-0.931242779705751,0.,0.364399348580519));
#52008=DIRECTION('',(0.,1.,0.));
#52009=DIRECTION('center_axis',(0.624280230025758,0.,-0.781200482846105));
#52010=DIRECTION('ref_axis',(-0.781200482846105,0.,-0.624280230025758));
#52011=DIRECTION('center_axis',(0.988679578606276,0.,0.150042296859641));
#52012=DIRECTION('ref_axis',(0.150042296859641,0.,-0.988679578606276));
#52013=DIRECTION('',(0.,1.,0.));
#52014=DIRECTION('',(0.,1.,0.));
#52015=DIRECTION('center_axis',(0.364399348580517,0.,0.931242779705752));
#52016=DIRECTION('ref_axis',(0.931242779705752,0.,-0.364399348580517));
#52017=DIRECTION('',(0.,1.,0.));
#52018=DIRECTION('center_axis',(-0.624280230025758,0.,0.781200482846104));
#52019=DIRECTION('ref_axis',(0.781200482846104,0.,0.624280230025758));
#52020=DIRECTION('',(0.,1.,0.));
#52021=DIRECTION('center_axis',(-0.988679578606275,0.,-0.150042296859647));
#52022=DIRECTION('ref_axis',(-0.150042296859647,0.,0.988679578606275));
#52023=DIRECTION('',(0.,1.,0.));
#52024=DIRECTION('center_axis',(-0.364399348580519,0.,-0.931242779705751));
#52025=DIRECTION('ref_axis',(-0.931242779705751,0.,0.364399348580519));
#52026=DIRECTION('',(0.,1.,0.));
#52027=DIRECTION('center_axis',(0.624280230025758,0.,-0.781200482846105));
#52028=DIRECTION('ref_axis',(-0.781200482846105,0.,-0.624280230025758));
#52029=DIRECTION('center_axis',(0.988679578606276,0.,0.150042296859641));
#52030=DIRECTION('ref_axis',(0.150042296859641,0.,-0.988679578606276));
#52031=DIRECTION('',(0.,1.,0.));
#52032=DIRECTION('',(0.,1.,0.));
#52033=DIRECTION('center_axis',(0.364399348580517,0.,0.931242779705752));
#52034=DIRECTION('ref_axis',(0.931242779705752,0.,-0.364399348580517));
#52035=DIRECTION('',(0.,1.,0.));
#52036=DIRECTION('center_axis',(-0.624280230025758,0.,0.781200482846104));
#52037=DIRECTION('ref_axis',(0.781200482846104,0.,0.624280230025758));
#52038=DIRECTION('',(0.,1.,0.));
#52039=DIRECTION('center_axis',(-0.988679578606275,0.,-0.150042296859647));
#52040=DIRECTION('ref_axis',(-0.150042296859647,0.,0.988679578606275));
#52041=DIRECTION('',(0.,1.,0.));
#52042=DIRECTION('center_axis',(-0.364399348580519,0.,-0.931242779705751));
#52043=DIRECTION('ref_axis',(-0.931242779705751,0.,0.364399348580519));
#52044=DIRECTION('',(0.,1.,0.));
#52045=DIRECTION('center_axis',(0.624280230025758,0.,-0.781200482846105));
#52046=DIRECTION('ref_axis',(-0.781200482846105,0.,-0.624280230025758));
#52047=DIRECTION('center_axis',(0.988679578606276,0.,0.150042296859641));
#52048=DIRECTION('ref_axis',(0.150042296859641,0.,-0.988679578606276));
#52049=DIRECTION('',(0.,1.,0.));
#52050=DIRECTION('',(0.,1.,0.));
#52051=DIRECTION('center_axis',(0.364399348580517,0.,0.931242779705752));
#52052=DIRECTION('ref_axis',(0.931242779705752,0.,-0.364399348580517));
#52053=DIRECTION('',(0.,1.,0.));
#52054=DIRECTION('center_axis',(-0.624280230025758,0.,0.781200482846104));
#52055=DIRECTION('ref_axis',(0.781200482846104,0.,0.624280230025758));
#52056=DIRECTION('',(0.,1.,0.));
#52057=DIRECTION('center_axis',(-0.988679578606275,0.,-0.150042296859647));
#52058=DIRECTION('ref_axis',(-0.150042296859647,0.,0.988679578606275));
#52059=DIRECTION('',(0.,1.,0.));
#52060=DIRECTION('center_axis',(-0.364399348580519,0.,-0.931242779705751));
#52061=DIRECTION('ref_axis',(-0.931242779705751,0.,0.364399348580519));
#52062=DIRECTION('',(0.,1.,0.));
#52063=DIRECTION('center_axis',(0.624280230025758,0.,-0.781200482846105));
#52064=DIRECTION('ref_axis',(-0.781200482846105,0.,-0.624280230025758));
#52065=DIRECTION('center_axis',(0.988679578606276,0.,0.150042296859641));
#52066=DIRECTION('ref_axis',(0.150042296859641,0.,-0.988679578606276));
#52067=DIRECTION('',(0.,1.,0.));
#52068=DIRECTION('',(0.,1.,0.));
#52069=DIRECTION('center_axis',(0.364399348580517,0.,0.931242779705752));
#52070=DIRECTION('ref_axis',(0.931242779705752,0.,-0.364399348580517));
#52071=DIRECTION('',(0.,1.,0.));
#52072=DIRECTION('center_axis',(-0.624280230025758,0.,0.781200482846104));
#52073=DIRECTION('ref_axis',(0.781200482846104,0.,0.624280230025758));
#52074=DIRECTION('',(0.,1.,0.));
#52075=DIRECTION('center_axis',(-0.988679578606275,0.,-0.150042296859647));
#52076=DIRECTION('ref_axis',(-0.150042296859647,0.,0.988679578606275));
#52077=DIRECTION('',(0.,1.,0.));
#52078=DIRECTION('center_axis',(-0.364399348580519,0.,-0.931242779705751));
#52079=DIRECTION('ref_axis',(-0.931242779705751,0.,0.364399348580519));
#52080=DIRECTION('',(0.,1.,0.));
#52081=DIRECTION('center_axis',(0.624280230025758,0.,-0.781200482846105));
#52082=DIRECTION('ref_axis',(-0.781200482846105,0.,-0.624280230025758));
#52083=DIRECTION('center_axis',(0.988679578606276,0.,0.150042296859641));
#52084=DIRECTION('ref_axis',(0.150042296859641,0.,-0.988679578606276));
#52085=DIRECTION('',(0.,1.,0.));
#52086=DIRECTION('',(0.,1.,0.));
#52087=DIRECTION('center_axis',(0.364399348580517,0.,0.931242779705752));
#52088=DIRECTION('ref_axis',(0.931242779705752,0.,-0.364399348580517));
#52089=DIRECTION('',(0.,1.,0.));
#52090=DIRECTION('center_axis',(-0.624280230025758,0.,0.781200482846104));
#52091=DIRECTION('ref_axis',(0.781200482846104,0.,0.624280230025758));
#52092=DIRECTION('',(0.,1.,0.));
#52093=DIRECTION('center_axis',(-0.988679578606275,0.,-0.150042296859647));
#52094=DIRECTION('ref_axis',(-0.150042296859647,0.,0.988679578606275));
#52095=DIRECTION('',(0.,1.,0.));
#52096=DIRECTION('center_axis',(-0.364399348580519,0.,-0.931242779705751));
#52097=DIRECTION('ref_axis',(-0.931242779705751,0.,0.364399348580519));
#52098=DIRECTION('',(0.,1.,0.));
#52099=DIRECTION('center_axis',(0.624280230025758,0.,-0.781200482846105));
#52100=DIRECTION('ref_axis',(-0.781200482846105,0.,-0.624280230025758));
#52101=DIRECTION('center_axis',(0.988679578606276,0.,0.150042296859641));
#52102=DIRECTION('ref_axis',(0.150042296859641,0.,-0.988679578606276));
#52103=DIRECTION('',(0.,1.,0.));
#52104=DIRECTION('',(0.,1.,0.));
#52105=DIRECTION('center_axis',(0.364399348580517,0.,0.931242779705752));
#52106=DIRECTION('ref_axis',(0.931242779705752,0.,-0.364399348580517));
#52107=DIRECTION('',(0.,1.,0.));
#52108=DIRECTION('center_axis',(-0.624280230025758,0.,0.781200482846104));
#52109=DIRECTION('ref_axis',(0.781200482846104,0.,0.624280230025758));
#52110=DIRECTION('',(0.,1.,0.));
#52111=DIRECTION('center_axis',(-0.988679578606275,0.,-0.150042296859647));
#52112=DIRECTION('ref_axis',(-0.150042296859647,0.,0.988679578606275));
#52113=DIRECTION('',(0.,1.,0.));
#52114=DIRECTION('center_axis',(-0.364399348580519,0.,-0.931242779705751));
#52115=DIRECTION('ref_axis',(-0.931242779705751,0.,0.364399348580519));
#52116=DIRECTION('',(0.,1.,0.));
#52117=DIRECTION('center_axis',(0.624280230025758,0.,-0.781200482846105));
#52118=DIRECTION('ref_axis',(-0.781200482846105,0.,-0.624280230025758));
#52119=DIRECTION('center_axis',(0.988679578606276,0.,0.150042296859641));
#52120=DIRECTION('ref_axis',(0.150042296859641,0.,-0.988679578606276));
#52121=DIRECTION('',(0.,1.,0.));
#52122=DIRECTION('',(0.,1.,0.));
#52123=DIRECTION('center_axis',(0.364399348580517,0.,0.931242779705752));
#52124=DIRECTION('ref_axis',(0.931242779705752,0.,-0.364399348580517));
#52125=DIRECTION('',(0.,1.,0.));
#52126=DIRECTION('center_axis',(-0.624280230025758,0.,0.781200482846104));
#52127=DIRECTION('ref_axis',(0.781200482846104,0.,0.624280230025758));
#52128=DIRECTION('',(0.,1.,0.));
#52129=DIRECTION('center_axis',(-0.988679578606275,0.,-0.150042296859647));
#52130=DIRECTION('ref_axis',(-0.150042296859647,0.,0.988679578606275));
#52131=DIRECTION('',(0.,1.,0.));
#52132=DIRECTION('center_axis',(-0.364399348580519,0.,-0.931242779705751));
#52133=DIRECTION('ref_axis',(-0.931242779705751,0.,0.364399348580519));
#52134=DIRECTION('',(0.,1.,0.));
#52135=DIRECTION('center_axis',(0.624280230025758,0.,-0.781200482846105));
#52136=DIRECTION('ref_axis',(-0.781200482846105,0.,-0.624280230025758));
#52137=DIRECTION('center_axis',(0.988679578606276,0.,0.150042296859641));
#52138=DIRECTION('ref_axis',(0.150042296859641,0.,-0.988679578606276));
#52139=DIRECTION('',(0.,1.,0.));
#52140=DIRECTION('',(0.,1.,0.));
#52141=DIRECTION('center_axis',(0.364399348580517,0.,0.931242779705752));
#52142=DIRECTION('ref_axis',(0.931242779705752,0.,-0.364399348580517));
#52143=DIRECTION('',(0.,1.,0.));
#52144=DIRECTION('center_axis',(-0.624280230025758,0.,0.781200482846104));
#52145=DIRECTION('ref_axis',(0.781200482846104,0.,0.624280230025758));
#52146=DIRECTION('',(0.,1.,0.));
#52147=DIRECTION('center_axis',(-0.988679578606275,0.,-0.150042296859647));
#52148=DIRECTION('ref_axis',(-0.150042296859647,0.,0.988679578606275));
#52149=DIRECTION('',(0.,1.,0.));
#52150=DIRECTION('center_axis',(-0.364399348580519,0.,-0.931242779705751));
#52151=DIRECTION('ref_axis',(-0.931242779705751,0.,0.364399348580519));
#52152=DIRECTION('',(0.,1.,0.));
#52153=DIRECTION('center_axis',(0.624280230025758,0.,-0.781200482846105));
#52154=DIRECTION('ref_axis',(-0.781200482846105,0.,-0.624280230025758));
#52155=DIRECTION('center_axis',(0.988679578606276,0.,0.150042296859641));
#52156=DIRECTION('ref_axis',(0.150042296859641,0.,-0.988679578606276));
#52157=DIRECTION('',(0.,1.,0.));
#52158=DIRECTION('',(0.,1.,0.));
#52159=DIRECTION('center_axis',(0.364399348580517,0.,0.931242779705752));
#52160=DIRECTION('ref_axis',(0.931242779705752,0.,-0.364399348580517));
#52161=DIRECTION('',(0.,1.,0.));
#52162=DIRECTION('center_axis',(-0.624280230025758,0.,0.781200482846104));
#52163=DIRECTION('ref_axis',(0.781200482846104,0.,0.624280230025758));
#52164=DIRECTION('',(0.,1.,0.));
#52165=DIRECTION('center_axis',(-0.988679578606275,0.,-0.150042296859647));
#52166=DIRECTION('ref_axis',(-0.150042296859647,0.,0.988679578606275));
#52167=DIRECTION('',(0.,1.,0.));
#52168=DIRECTION('center_axis',(-0.364399348580519,0.,-0.931242779705751));
#52169=DIRECTION('ref_axis',(-0.931242779705751,0.,0.364399348580519));
#52170=DIRECTION('',(0.,1.,0.));
#52171=DIRECTION('center_axis',(0.624280230025758,0.,-0.781200482846105));
#52172=DIRECTION('ref_axis',(-0.781200482846105,0.,-0.624280230025758));
#52173=DIRECTION('center_axis',(0.988679578606276,0.,0.150042296859641));
#52174=DIRECTION('ref_axis',(0.150042296859641,0.,-0.988679578606276));
#52175=DIRECTION('',(0.,1.,0.));
#52176=DIRECTION('',(0.,1.,0.));
#52177=DIRECTION('center_axis',(0.364399348580517,0.,0.931242779705752));
#52178=DIRECTION('ref_axis',(0.931242779705752,0.,-0.364399348580517));
#52179=DIRECTION('',(0.,1.,0.));
#52180=DIRECTION('center_axis',(-0.624280230025758,0.,0.781200482846104));
#52181=DIRECTION('ref_axis',(0.781200482846104,0.,0.624280230025758));
#52182=DIRECTION('',(0.,1.,0.));
#52183=DIRECTION('center_axis',(-0.988679578606275,0.,-0.150042296859647));
#52184=DIRECTION('ref_axis',(-0.150042296859647,0.,0.988679578606275));
#52185=DIRECTION('',(0.,1.,0.));
#52186=DIRECTION('center_axis',(-0.364399348580519,0.,-0.931242779705751));
#52187=DIRECTION('ref_axis',(-0.931242779705751,0.,0.364399348580519));
#52188=DIRECTION('',(0.,1.,0.));
#52189=DIRECTION('center_axis',(0.624280230025758,0.,-0.781200482846105));
#52190=DIRECTION('ref_axis',(-0.781200482846105,0.,-0.624280230025758));
#52191=DIRECTION('center_axis',(0.988679578606276,0.,0.150042296859641));
#52192=DIRECTION('ref_axis',(0.150042296859641,0.,-0.988679578606276));
#52193=DIRECTION('',(0.,1.,0.));
#52194=DIRECTION('',(0.,1.,0.));
#52195=DIRECTION('center_axis',(0.364399348580517,0.,0.931242779705752));
#52196=DIRECTION('ref_axis',(0.931242779705752,0.,-0.364399348580517));
#52197=DIRECTION('',(0.,1.,0.));
#52198=DIRECTION('center_axis',(-0.624280230025758,0.,0.781200482846104));
#52199=DIRECTION('ref_axis',(0.781200482846104,0.,0.624280230025758));
#52200=DIRECTION('',(0.,1.,0.));
#52201=DIRECTION('center_axis',(-0.988679578606275,0.,-0.150042296859647));
#52202=DIRECTION('ref_axis',(-0.150042296859647,0.,0.988679578606275));
#52203=DIRECTION('',(0.,1.,0.));
#52204=DIRECTION('center_axis',(-0.364399348580519,0.,-0.931242779705751));
#52205=DIRECTION('ref_axis',(-0.931242779705751,0.,0.364399348580519));
#52206=DIRECTION('',(0.,1.,0.));
#52207=DIRECTION('center_axis',(0.624280230025758,0.,-0.781200482846105));
#52208=DIRECTION('ref_axis',(-0.781200482846105,0.,-0.624280230025758));
#52209=DIRECTION('center_axis',(0.988679578606276,0.,0.150042296859641));
#52210=DIRECTION('ref_axis',(0.150042296859641,0.,-0.988679578606276));
#52211=DIRECTION('',(0.,1.,0.));
#52212=DIRECTION('',(0.,1.,0.));
#52213=DIRECTION('center_axis',(0.364399348580517,0.,0.931242779705752));
#52214=DIRECTION('ref_axis',(0.931242779705752,0.,-0.364399348580517));
#52215=DIRECTION('',(0.,1.,0.));
#52216=DIRECTION('center_axis',(-0.624280230025758,0.,0.781200482846104));
#52217=DIRECTION('ref_axis',(0.781200482846104,0.,0.624280230025758));
#52218=DIRECTION('',(0.,1.,0.));
#52219=DIRECTION('center_axis',(-0.988679578606275,0.,-0.150042296859647));
#52220=DIRECTION('ref_axis',(-0.150042296859647,0.,0.988679578606275));
#52221=DIRECTION('',(0.,1.,0.));
#52222=DIRECTION('center_axis',(-0.364399348580519,0.,-0.931242779705751));
#52223=DIRECTION('ref_axis',(-0.931242779705751,0.,0.364399348580519));
#52224=DIRECTION('',(0.,1.,0.));
#52225=DIRECTION('center_axis',(0.624280230025758,0.,-0.781200482846105));
#52226=DIRECTION('ref_axis',(-0.781200482846105,0.,-0.624280230025758));
#52227=DIRECTION('center_axis',(0.988679578606276,0.,0.150042296859641));
#52228=DIRECTION('ref_axis',(0.150042296859641,0.,-0.988679578606276));
#52229=DIRECTION('',(0.,1.,0.));
#52230=DIRECTION('',(0.,1.,0.));
#52231=DIRECTION('center_axis',(0.364399348580517,0.,0.931242779705752));
#52232=DIRECTION('ref_axis',(0.931242779705752,0.,-0.364399348580517));
#52233=DIRECTION('',(0.,1.,0.));
#52234=DIRECTION('center_axis',(-0.624280230025758,0.,0.781200482846104));
#52235=DIRECTION('ref_axis',(0.781200482846104,0.,0.624280230025758));
#52236=DIRECTION('',(0.,1.,0.));
#52237=DIRECTION('center_axis',(-0.988679578606275,0.,-0.150042296859647));
#52238=DIRECTION('ref_axis',(-0.150042296859647,0.,0.988679578606275));
#52239=DIRECTION('',(0.,1.,0.));
#52240=DIRECTION('center_axis',(-0.364399348580519,0.,-0.931242779705751));
#52241=DIRECTION('ref_axis',(-0.931242779705751,0.,0.364399348580519));
#52242=DIRECTION('',(0.,1.,0.));
#52243=DIRECTION('center_axis',(0.624280230025758,0.,-0.781200482846105));
#52244=DIRECTION('ref_axis',(-0.781200482846105,0.,-0.624280230025758));
#52245=DIRECTION('center_axis',(0.988679578606276,0.,0.150042296859641));
#52246=DIRECTION('ref_axis',(0.150042296859641,0.,-0.988679578606276));
#52247=DIRECTION('',(0.,1.,0.));
#52248=DIRECTION('',(0.,1.,0.));
#52249=DIRECTION('center_axis',(0.364399348580517,0.,0.931242779705752));
#52250=DIRECTION('ref_axis',(0.931242779705752,0.,-0.364399348580517));
#52251=DIRECTION('',(0.,1.,0.));
#52252=DIRECTION('center_axis',(-0.624280230025758,0.,0.781200482846104));
#52253=DIRECTION('ref_axis',(0.781200482846104,0.,0.624280230025758));
#52254=DIRECTION('',(0.,1.,0.));
#52255=DIRECTION('center_axis',(-0.988679578606275,0.,-0.150042296859647));
#52256=DIRECTION('ref_axis',(-0.150042296859647,0.,0.988679578606275));
#52257=DIRECTION('',(0.,1.,0.));
#52258=DIRECTION('center_axis',(-0.364399348580519,0.,-0.931242779705751));
#52259=DIRECTION('ref_axis',(-0.931242779705751,0.,0.364399348580519));
#52260=DIRECTION('',(0.,1.,0.));
#52261=DIRECTION('center_axis',(0.624280230025758,0.,-0.781200482846105));
#52262=DIRECTION('ref_axis',(-0.781200482846105,0.,-0.624280230025758));
#52263=DIRECTION('center_axis',(0.988679578606276,0.,0.150042296859641));
#52264=DIRECTION('ref_axis',(0.150042296859641,0.,-0.988679578606276));
#52265=DIRECTION('',(0.,1.,0.));
#52266=DIRECTION('',(0.,1.,0.));
#52267=DIRECTION('center_axis',(0.364399348580517,0.,0.931242779705752));
#52268=DIRECTION('ref_axis',(0.931242779705752,0.,-0.364399348580517));
#52269=DIRECTION('',(0.,1.,0.));
#52270=DIRECTION('center_axis',(-0.624280230025758,0.,0.781200482846104));
#52271=DIRECTION('ref_axis',(0.781200482846104,0.,0.624280230025758));
#52272=DIRECTION('',(0.,1.,0.));
#52273=DIRECTION('center_axis',(-0.988679578606275,0.,-0.150042296859647));
#52274=DIRECTION('ref_axis',(-0.150042296859647,0.,0.988679578606275));
#52275=DIRECTION('',(0.,1.,0.));
#52276=DIRECTION('center_axis',(-0.364399348580519,0.,-0.931242779705751));
#52277=DIRECTION('ref_axis',(-0.931242779705751,0.,0.364399348580519));
#52278=DIRECTION('',(0.,1.,0.));
#52279=DIRECTION('center_axis',(0.624280230025758,0.,-0.781200482846105));
#52280=DIRECTION('ref_axis',(-0.781200482846105,0.,-0.624280230025758));
#52281=DIRECTION('center_axis',(0.988679578606276,0.,0.150042296859641));
#52282=DIRECTION('ref_axis',(0.150042296859641,0.,-0.988679578606276));
#52283=DIRECTION('',(0.,1.,0.));
#52284=DIRECTION('',(0.,1.,0.));
#52285=DIRECTION('center_axis',(0.364399348580517,0.,0.931242779705752));
#52286=DIRECTION('ref_axis',(0.931242779705752,0.,-0.364399348580517));
#52287=DIRECTION('',(0.,1.,0.));
#52288=DIRECTION('center_axis',(-0.624280230025758,0.,0.781200482846104));
#52289=DIRECTION('ref_axis',(0.781200482846104,0.,0.624280230025758));
#52290=DIRECTION('',(0.,1.,0.));
#52291=DIRECTION('center_axis',(-0.988679578606275,0.,-0.150042296859647));
#52292=DIRECTION('ref_axis',(-0.150042296859647,0.,0.988679578606275));
#52293=DIRECTION('',(0.,1.,0.));
#52294=DIRECTION('center_axis',(-0.364399348580519,0.,-0.931242779705751));
#52295=DIRECTION('ref_axis',(-0.931242779705751,0.,0.364399348580519));
#52296=DIRECTION('',(0.,1.,0.));
#52297=DIRECTION('center_axis',(0.624280230025758,0.,-0.781200482846105));
#52298=DIRECTION('ref_axis',(-0.781200482846105,0.,-0.624280230025758));
#52299=DIRECTION('center_axis',(0.988679578606276,0.,0.150042296859641));
#52300=DIRECTION('ref_axis',(0.150042296859641,0.,-0.988679578606276));
#52301=DIRECTION('',(0.,1.,0.));
#52302=DIRECTION('',(0.,1.,0.));
#52303=DIRECTION('center_axis',(0.364399348580517,0.,0.931242779705752));
#52304=DIRECTION('ref_axis',(0.931242779705752,0.,-0.364399348580517));
#52305=DIRECTION('',(0.,1.,0.));
#52306=DIRECTION('center_axis',(-0.624280230025758,0.,0.781200482846104));
#52307=DIRECTION('ref_axis',(0.781200482846104,0.,0.624280230025758));
#52308=DIRECTION('',(0.,1.,0.));
#52309=DIRECTION('center_axis',(-0.988679578606275,0.,-0.150042296859647));
#52310=DIRECTION('ref_axis',(-0.150042296859647,0.,0.988679578606275));
#52311=DIRECTION('',(0.,1.,0.));
#52312=DIRECTION('center_axis',(-0.364399348580519,0.,-0.931242779705751));
#52313=DIRECTION('ref_axis',(-0.931242779705751,0.,0.364399348580519));
#52314=DIRECTION('',(0.,1.,0.));
#52315=DIRECTION('center_axis',(0.624280230025758,0.,-0.781200482846105));
#52316=DIRECTION('ref_axis',(-0.781200482846105,0.,-0.624280230025758));
#52317=DIRECTION('center_axis',(0.988679578606276,0.,0.150042296859641));
#52318=DIRECTION('ref_axis',(0.150042296859641,0.,-0.988679578606276));
#52319=DIRECTION('',(0.,1.,0.));
#52320=DIRECTION('',(0.,1.,0.));
#52321=DIRECTION('center_axis',(0.364399348580517,0.,0.931242779705752));
#52322=DIRECTION('ref_axis',(0.931242779705752,0.,-0.364399348580517));
#52323=DIRECTION('',(0.,1.,0.));
#52324=DIRECTION('center_axis',(-0.624280230025758,0.,0.781200482846104));
#52325=DIRECTION('ref_axis',(0.781200482846104,0.,0.624280230025758));
#52326=DIRECTION('',(0.,1.,0.));
#52327=DIRECTION('center_axis',(-0.988679578606275,0.,-0.150042296859647));
#52328=DIRECTION('ref_axis',(-0.150042296859647,0.,0.988679578606275));
#52329=DIRECTION('',(0.,1.,0.));
#52330=DIRECTION('center_axis',(-0.364399348580519,0.,-0.931242779705751));
#52331=DIRECTION('ref_axis',(-0.931242779705751,0.,0.364399348580519));
#52332=DIRECTION('',(0.,1.,0.));
#52333=DIRECTION('center_axis',(0.624280230025758,0.,-0.781200482846105));
#52334=DIRECTION('ref_axis',(-0.781200482846105,0.,-0.624280230025758));
#52335=DIRECTION('center_axis',(0.988679578606276,0.,0.150042296859641));
#52336=DIRECTION('ref_axis',(0.150042296859641,0.,-0.988679578606276));
#52337=DIRECTION('',(0.,1.,0.));
#52338=DIRECTION('',(0.,1.,0.));
#52339=DIRECTION('center_axis',(0.364399348580517,0.,0.931242779705752));
#52340=DIRECTION('ref_axis',(0.931242779705752,0.,-0.364399348580517));
#52341=DIRECTION('',(0.,1.,0.));
#52342=DIRECTION('center_axis',(-0.624280230025758,0.,0.781200482846104));
#52343=DIRECTION('ref_axis',(0.781200482846104,0.,0.624280230025758));
#52344=DIRECTION('',(0.,1.,0.));
#52345=DIRECTION('center_axis',(-0.988679578606275,0.,-0.150042296859647));
#52346=DIRECTION('ref_axis',(-0.150042296859647,0.,0.988679578606275));
#52347=DIRECTION('',(0.,1.,0.));
#52348=DIRECTION('center_axis',(-0.364399348580519,0.,-0.931242779705751));
#52349=DIRECTION('ref_axis',(-0.931242779705751,0.,0.364399348580519));
#52350=DIRECTION('',(0.,1.,0.));
#52351=DIRECTION('center_axis',(0.624280230025758,0.,-0.781200482846105));
#52352=DIRECTION('ref_axis',(-0.781200482846105,0.,-0.624280230025758));
#52353=DIRECTION('center_axis',(0.988679578606276,0.,0.150042296859641));
#52354=DIRECTION('ref_axis',(0.150042296859641,0.,-0.988679578606276));
#52355=DIRECTION('',(0.,1.,0.));
#52356=DIRECTION('',(0.,1.,0.));
#52357=DIRECTION('center_axis',(0.364399348580517,0.,0.931242779705752));
#52358=DIRECTION('ref_axis',(0.931242779705752,0.,-0.364399348580517));
#52359=DIRECTION('',(0.,1.,0.));
#52360=DIRECTION('center_axis',(-0.624280230025758,0.,0.781200482846104));
#52361=DIRECTION('ref_axis',(0.781200482846104,0.,0.624280230025758));
#52362=DIRECTION('',(0.,1.,0.));
#52363=DIRECTION('center_axis',(-0.988679578606275,0.,-0.150042296859647));
#52364=DIRECTION('ref_axis',(-0.150042296859647,0.,0.988679578606275));
#52365=DIRECTION('',(0.,1.,0.));
#52366=DIRECTION('center_axis',(-0.364399348580519,0.,-0.931242779705751));
#52367=DIRECTION('ref_axis',(-0.931242779705751,0.,0.364399348580519));
#52368=DIRECTION('',(0.,1.,0.));
#52369=DIRECTION('center_axis',(0.624280230025758,0.,-0.781200482846105));
#52370=DIRECTION('ref_axis',(-0.781200482846105,0.,-0.624280230025758));
#52371=DIRECTION('center_axis',(0.988679578606276,0.,0.150042296859641));
#52372=DIRECTION('ref_axis',(0.150042296859641,0.,-0.988679578606276));
#52373=DIRECTION('',(0.,1.,0.));
#52374=DIRECTION('',(0.,1.,0.));
#52375=DIRECTION('center_axis',(0.364399348580517,0.,0.931242779705752));
#52376=DIRECTION('ref_axis',(0.931242779705752,0.,-0.364399348580517));
#52377=DIRECTION('',(0.,1.,0.));
#52378=DIRECTION('center_axis',(-0.624280230025758,0.,0.781200482846104));
#52379=DIRECTION('ref_axis',(0.781200482846104,0.,0.624280230025758));
#52380=DIRECTION('',(0.,1.,0.));
#52381=DIRECTION('center_axis',(-0.988679578606275,0.,-0.150042296859647));
#52382=DIRECTION('ref_axis',(-0.150042296859647,0.,0.988679578606275));
#52383=DIRECTION('',(0.,1.,0.));
#52384=DIRECTION('center_axis',(-0.364399348580519,0.,-0.931242779705751));
#52385=DIRECTION('ref_axis',(-0.931242779705751,0.,0.364399348580519));
#52386=DIRECTION('',(0.,1.,0.));
#52387=DIRECTION('center_axis',(0.624280230025758,0.,-0.781200482846105));
#52388=DIRECTION('ref_axis',(-0.781200482846105,0.,-0.624280230025758));
#52389=DIRECTION('center_axis',(0.988679578606276,0.,0.150042296859641));
#52390=DIRECTION('ref_axis',(0.150042296859641,0.,-0.988679578606276));
#52391=DIRECTION('',(0.,1.,0.));
#52392=DIRECTION('',(0.,1.,0.));
#52393=DIRECTION('center_axis',(0.364399348580517,0.,0.931242779705752));
#52394=DIRECTION('ref_axis',(0.931242779705752,0.,-0.364399348580517));
#52395=DIRECTION('',(0.,1.,0.));
#52396=DIRECTION('center_axis',(-0.624280230025758,0.,0.781200482846104));
#52397=DIRECTION('ref_axis',(0.781200482846104,0.,0.624280230025758));
#52398=DIRECTION('',(0.,1.,0.));
#52399=DIRECTION('center_axis',(-0.988679578606275,0.,-0.150042296859647));
#52400=DIRECTION('ref_axis',(-0.150042296859647,0.,0.988679578606275));
#52401=DIRECTION('',(0.,1.,0.));
#52402=DIRECTION('center_axis',(-0.364399348580519,0.,-0.931242779705751));
#52403=DIRECTION('ref_axis',(-0.931242779705751,0.,0.364399348580519));
#52404=DIRECTION('',(0.,1.,0.));
#52405=DIRECTION('center_axis',(0.624280230025758,0.,-0.781200482846105));
#52406=DIRECTION('ref_axis',(-0.781200482846105,0.,-0.624280230025758));
#52407=DIRECTION('center_axis',(0.988679578606276,0.,0.150042296859641));
#52408=DIRECTION('ref_axis',(0.150042296859641,0.,-0.988679578606276));
#52409=DIRECTION('',(0.,1.,0.));
#52410=DIRECTION('',(0.,1.,0.));
#52411=DIRECTION('center_axis',(0.364399348580517,0.,0.931242779705752));
#52412=DIRECTION('ref_axis',(0.931242779705752,0.,-0.364399348580517));
#52413=DIRECTION('',(0.,1.,0.));
#52414=DIRECTION('center_axis',(-0.624280230025758,0.,0.781200482846104));
#52415=DIRECTION('ref_axis',(0.781200482846104,0.,0.624280230025758));
#52416=DIRECTION('',(0.,1.,0.));
#52417=DIRECTION('center_axis',(-0.988679578606275,0.,-0.150042296859647));
#52418=DIRECTION('ref_axis',(-0.150042296859647,0.,0.988679578606275));
#52419=DIRECTION('',(0.,1.,0.));
#52420=DIRECTION('center_axis',(-0.364399348580519,0.,-0.931242779705751));
#52421=DIRECTION('ref_axis',(-0.931242779705751,0.,0.364399348580519));
#52422=DIRECTION('',(0.,1.,0.));
#52423=DIRECTION('center_axis',(0.624280230025758,0.,-0.781200482846105));
#52424=DIRECTION('ref_axis',(-0.781200482846105,0.,-0.624280230025758));
#52425=DIRECTION('center_axis',(0.988679578606276,0.,0.150042296859641));
#52426=DIRECTION('ref_axis',(0.150042296859641,0.,-0.988679578606276));
#52427=DIRECTION('',(0.,1.,0.));
#52428=DIRECTION('',(0.,1.,0.));
#52429=DIRECTION('center_axis',(0.364399348580517,0.,0.931242779705752));
#52430=DIRECTION('ref_axis',(0.931242779705752,0.,-0.364399348580517));
#52431=DIRECTION('',(0.,1.,0.));
#52432=DIRECTION('center_axis',(-0.624280230025758,0.,0.781200482846104));
#52433=DIRECTION('ref_axis',(0.781200482846104,0.,0.624280230025758));
#52434=DIRECTION('',(0.,1.,0.));
#52435=DIRECTION('center_axis',(-0.988679578606275,0.,-0.150042296859647));
#52436=DIRECTION('ref_axis',(-0.150042296859647,0.,0.988679578606275));
#52437=DIRECTION('',(0.,1.,0.));
#52438=DIRECTION('center_axis',(-0.364399348580519,0.,-0.931242779705751));
#52439=DIRECTION('ref_axis',(-0.931242779705751,0.,0.364399348580519));
#52440=DIRECTION('',(0.,1.,0.));
#52441=DIRECTION('center_axis',(0.624280230025758,0.,-0.781200482846105));
#52442=DIRECTION('ref_axis',(-0.781200482846105,0.,-0.624280230025758));
#52443=DIRECTION('',(1.,0.,0.));
#52444=DIRECTION('',(0.,0.,-1.));
#52445=DIRECTION('',(0.,0.,1.));
#52446=DIRECTION('',(1.,0.,0.));
#52447=DIRECTION('',(-1.28155793877546E-15,0.,1.));
#52448=DIRECTION('',(-3.22130537245211E-15,1.,-4.12828947328605E-30));
#52449=DIRECTION('',(0.,0.,1.));
#52450=DIRECTION('',(1.,0.,0.));
#52451=CARTESIAN_POINT('',(0.,0.,0.));
#52452=CARTESIAN_POINT('',(0.,0.,0.));
#52453=CARTESIAN_POINT('Origin',(-74.39,83.,-72.));
#52454=CARTESIAN_POINT('',(-83.59,84.75,-72.));
#52455=CARTESIAN_POINT('Origin',(-83.59,83.,-72.));
#52456=CARTESIAN_POINT('',(-84.39,84.75,-72.));
#52457=CARTESIAN_POINT('',(-74.39,84.75,-72.));
#52458=CARTESIAN_POINT('Origin',(-84.39,83.,-72.));
#52459=CARTESIAN_POINT('Origin',(-74.39,1.15752220392301,-72.));
#52460=CARTESIAN_POINT('',(-83.59,2.907522203923,-72.));
#52461=CARTESIAN_POINT('Origin',(-83.59,1.157522203923,-72.));
#52462=CARTESIAN_POINT('',(-84.39,2.907522203923,-72.));
#52463=CARTESIAN_POINT('',(-74.39,2.907522203923,-72.));
#52464=CARTESIAN_POINT('Origin',(-84.39,1.157522203923,-72.));
#52465=CARTESIAN_POINT('Origin',(-74.39,1.15752220392301,72.));
#52466=CARTESIAN_POINT('',(-83.59,2.907522203923,72.));
#52467=CARTESIAN_POINT('Origin',(-83.59,1.157522203923,72.));
#52468=CARTESIAN_POINT('',(-84.39,2.907522203923,72.));
#52469=CARTESIAN_POINT('',(-74.39,2.907522203923,72.));
#52470=CARTESIAN_POINT('Origin',(-84.39,1.157522203923,72.));
#52471=CARTESIAN_POINT('Origin',(-74.39,83.,72.));
#52472=CARTESIAN_POINT('',(-83.59,84.75,72.));
#52473=CARTESIAN_POINT('Origin',(-83.59,83.,72.));
#52474=CARTESIAN_POINT('',(-84.39,84.75,72.));
#52475=CARTESIAN_POINT('',(-74.39,84.75,72.));
#52476=CARTESIAN_POINT('Origin',(-84.39,83.,72.));
#52477=CARTESIAN_POINT('Origin',(38.3304246383764,1.80000000000005,76.7999999999841));
#52478=CARTESIAN_POINT('',(39.5804246383764,1.80000000000005,76.7999999999841));
#52479=CARTESIAN_POINT('Origin',(38.3304246383764,1.80000000000005,76.7999999999841));
#52480=CARTESIAN_POINT('',(39.5804246383764,1.80000000000005,75.9999999999841));
#52481=CARTESIAN_POINT('',(39.5804246383764,1.80000000000005,76.7999999999841));
#52482=CARTESIAN_POINT('Origin',(38.3304246383764,1.80000000000005,75.9999999999841));
#52483=CARTESIAN_POINT('Origin',(-52.1104246383764,1.80000000000003,76.7999999999841));
#52484=CARTESIAN_POINT('',(-50.8604246383764,1.80000000000003,76.7999999999841));
#52485=CARTESIAN_POINT('Origin',(-52.1104246383764,1.80000000000003,76.7999999999841));
#52486=CARTESIAN_POINT('',(-50.8604246383764,1.80000000000003,75.9999999999841));
#52487=CARTESIAN_POINT('',(-50.8604246383764,1.80000000000003,76.7999999999841));
#52488=CARTESIAN_POINT('Origin',(-52.1104246383764,1.80000000000003,75.9999999999841));
#52489=CARTESIAN_POINT('Origin',(60.61,66.0787611019615,38.));
#52490=CARTESIAN_POINT('',(69.81,66.0787611019615,36.5));
#52491=CARTESIAN_POINT('',(69.81,66.0787611019615,39.5));
#52492=CARTESIAN_POINT('Origin',(69.81,66.0787611019615,38.));
#52493=CARTESIAN_POINT('',(70.61,66.0787611019615,36.5));
#52494=CARTESIAN_POINT('',(60.61,66.0787611019615,36.5));
#52495=CARTESIAN_POINT('',(70.61,66.0787611019615,39.5));
#52496=CARTESIAN_POINT('Origin',(70.61,66.0787611019615,38.));
#52497=CARTESIAN_POINT('',(60.61,66.0787611019615,39.5));
#52498=CARTESIAN_POINT('Origin',(60.61,38.0787611019615,68.));
#52499=CARTESIAN_POINT('',(69.81,38.0787611019615,69.5));
#52500=CARTESIAN_POINT('',(69.81,38.0787611019615,66.5));
#52501=CARTESIAN_POINT('Origin',(69.81,38.0787611019615,68.));
#52502=CARTESIAN_POINT('',(70.61,38.0787611019615,66.5));
#52503=CARTESIAN_POINT('',(60.61,38.0787611019615,66.5));
#52504=CARTESIAN_POINT('',(70.61,38.0787611019615,69.5));
#52505=CARTESIAN_POINT('Origin',(70.61,38.0787611019615,68.));
#52506=CARTESIAN_POINT('',(60.61,38.0787611019615,69.5));
#52507=CARTESIAN_POINT('Origin',(60.61,38.0787611019615,63.));
#52508=CARTESIAN_POINT('',(69.81,38.0787611019615,64.5));
#52509=CARTESIAN_POINT('',(69.81,38.0787611019615,61.5));
#52510=CARTESIAN_POINT('Origin',(69.81,38.0787611019615,63.));
#52511=CARTESIAN_POINT('',(70.61,38.0787611019615,61.5));
#52512=CARTESIAN_POINT('',(60.61,38.0787611019615,61.5));
#52513=CARTESIAN_POINT('',(70.61,38.0787611019615,64.5));
#52514=CARTESIAN_POINT('Origin',(70.61,38.0787611019615,63.));
#52515=CARTESIAN_POINT('',(60.61,38.0787611019615,64.5));
#52516=CARTESIAN_POINT('Origin',(60.61,38.0787611019615,58.));
#52517=CARTESIAN_POINT('',(69.81,38.0787611019615,59.5));
#52518=CARTESIAN_POINT('',(69.81,38.0787611019615,56.5));
#52519=CARTESIAN_POINT('Origin',(69.81,38.0787611019615,58.));
#52520=CARTESIAN_POINT('',(70.61,38.0787611019615,56.5));
#52521=CARTESIAN_POINT('',(60.61,38.0787611019615,56.5));
#52522=CARTESIAN_POINT('',(70.61,38.0787611019615,59.5));
#52523=CARTESIAN_POINT('Origin',(70.61,38.0787611019615,58.));
#52524=CARTESIAN_POINT('',(60.61,38.0787611019615,59.5));
#52525=CARTESIAN_POINT('Origin',(60.61,38.0787611019615,38.));
#52526=CARTESIAN_POINT('',(69.81,38.0787611019615,39.5));
#52527=CARTESIAN_POINT('',(69.81,38.0787611019615,36.5));
#52528=CARTESIAN_POINT('Origin',(69.81,38.0787611019615,38.));
#52529=CARTESIAN_POINT('',(70.61,38.0787611019615,36.5));
#52530=CARTESIAN_POINT('',(60.61,38.0787611019615,36.5));
#52531=CARTESIAN_POINT('',(70.61,38.0787611019615,39.5));
#52532=CARTESIAN_POINT('Origin',(70.61,38.0787611019615,38.));
#52533=CARTESIAN_POINT('',(60.61,38.0787611019615,39.5));
#52534=CARTESIAN_POINT('Origin',(60.61,38.0787611019615,33.));
#52535=CARTESIAN_POINT('',(69.81,38.0787611019615,34.5));
#52536=CARTESIAN_POINT('',(69.81,38.0787611019615,31.5));
#52537=CARTESIAN_POINT('Origin',(69.81,38.0787611019615,33.));
#52538=CARTESIAN_POINT('',(70.61,38.0787611019615,31.5));
#52539=CARTESIAN_POINT('',(60.61,38.0787611019615,31.5));
#52540=CARTESIAN_POINT('',(70.61,38.0787611019615,34.5));
#52541=CARTESIAN_POINT('Origin',(70.61,38.0787611019615,33.));
#52542=CARTESIAN_POINT('',(60.61,38.0787611019615,34.5));
#52543=CARTESIAN_POINT('Origin',(60.61,66.0787611019615,33.));
#52544=CARTESIAN_POINT('',(69.81,66.0787611019615,31.5));
#52545=CARTESIAN_POINT('',(69.81,66.0787611019615,34.5));
#52546=CARTESIAN_POINT('Origin',(69.81,66.0787611019615,33.));
#52547=CARTESIAN_POINT('',(70.61,66.0787611019615,31.5));
#52548=CARTESIAN_POINT('',(60.61,66.0787611019615,31.5));
#52549=CARTESIAN_POINT('',(70.61,66.0787611019615,34.5));
#52550=CARTESIAN_POINT('Origin',(70.61,66.0787611019615,33.));
#52551=CARTESIAN_POINT('',(60.61,66.0787611019615,34.5));
#52552=CARTESIAN_POINT('Origin',(60.61,66.0787611019615,28.));
#52553=CARTESIAN_POINT('',(69.81,66.0787611019615,26.5));
#52554=CARTESIAN_POINT('',(69.81,66.0787611019615,29.5));
#52555=CARTESIAN_POINT('Origin',(69.81,66.0787611019615,28.));
#52556=CARTESIAN_POINT('',(70.61,66.0787611019615,26.5));
#52557=CARTESIAN_POINT('',(60.61,66.0787611019615,26.5));
#52558=CARTESIAN_POINT('',(70.61,66.0787611019615,29.5));
#52559=CARTESIAN_POINT('Origin',(70.61,66.0787611019615,28.));
#52560=CARTESIAN_POINT('',(60.61,66.0787611019615,29.5));
#52561=CARTESIAN_POINT('Origin',(60.61,66.0787611019615,63.));
#52562=CARTESIAN_POINT('',(69.81,66.0787611019615,61.5));
#52563=CARTESIAN_POINT('',(69.81,66.0787611019615,64.5));
#52564=CARTESIAN_POINT('Origin',(69.81,66.0787611019615,63.));
#52565=CARTESIAN_POINT('',(70.61,66.0787611019615,61.5));
#52566=CARTESIAN_POINT('',(60.61,66.0787611019615,61.5));
#52567=CARTESIAN_POINT('',(70.61,66.0787611019615,64.5));
#52568=CARTESIAN_POINT('Origin',(70.61,66.0787611019615,63.));
#52569=CARTESIAN_POINT('',(60.61,66.0787611019615,64.5));
#52570=CARTESIAN_POINT('Origin',(60.61,66.0787611019615,58.));
#52571=CARTESIAN_POINT('',(69.81,66.0787611019615,56.5));
#52572=CARTESIAN_POINT('',(69.81,66.0787611019615,59.5));
#52573=CARTESIAN_POINT('Origin',(69.81,66.0787611019615,58.));
#52574=CARTESIAN_POINT('',(70.61,66.0787611019615,56.5));
#52575=CARTESIAN_POINT('',(60.61,66.0787611019615,56.5));
#52576=CARTESIAN_POINT('',(70.61,66.0787611019615,59.5));
#52577=CARTESIAN_POINT('Origin',(70.61,66.0787611019615,58.));
#52578=CARTESIAN_POINT('',(60.61,66.0787611019615,59.5));
#52579=CARTESIAN_POINT('Origin',(60.61,66.0787611019615,53.));
#52580=CARTESIAN_POINT('',(69.81,66.0787611019615,51.5));
#52581=CARTESIAN_POINT('',(69.81,66.0787611019615,54.5));
#52582=CARTESIAN_POINT('Origin',(69.81,66.0787611019615,53.));
#52583=CARTESIAN_POINT('',(70.61,66.0787611019615,51.5));
#52584=CARTESIAN_POINT('',(60.61,66.0787611019615,51.5));
#52585=CARTESIAN_POINT('',(70.61,66.0787611019615,54.5));
#52586=CARTESIAN_POINT('Origin',(70.61,66.0787611019615,53.));
#52587=CARTESIAN_POINT('',(60.61,66.0787611019615,54.5));
#52588=CARTESIAN_POINT('Origin',(60.61,66.0787611019615,48.));
#52589=CARTESIAN_POINT('',(69.81,66.0787611019615,46.5));
#52590=CARTESIAN_POINT('',(69.81,66.0787611019615,49.5));
#52591=CARTESIAN_POINT('Origin',(69.81,66.0787611019615,48.));
#52592=CARTESIAN_POINT('',(70.61,66.0787611019615,46.5));
#52593=CARTESIAN_POINT('',(60.61,66.0787611019615,46.5));
#52594=CARTESIAN_POINT('',(70.61,66.0787611019615,49.5));
#52595=CARTESIAN_POINT('Origin',(70.61,66.0787611019615,48.));
#52596=CARTESIAN_POINT('',(60.61,66.0787611019615,49.5));
#52597=CARTESIAN_POINT('Origin',(60.61,66.0787611019615,43.));
#52598=CARTESIAN_POINT('',(69.81,66.0787611019615,41.5));
#52599=CARTESIAN_POINT('',(69.81,66.0787611019615,44.5));
#52600=CARTESIAN_POINT('Origin',(69.81,66.0787611019615,43.));
#52601=CARTESIAN_POINT('',(70.61,66.0787611019615,41.5));
#52602=CARTESIAN_POINT('',(60.61,66.0787611019615,41.5));
#52603=CARTESIAN_POINT('',(70.61,66.0787611019615,44.5));
#52604=CARTESIAN_POINT('Origin',(70.61,66.0787611019615,43.));
#52605=CARTESIAN_POINT('',(60.61,66.0787611019615,44.5));
#52606=CARTESIAN_POINT('Origin',(60.61,38.0787611019615,43.));
#52607=CARTESIAN_POINT('',(69.81,38.0787611019615,44.5));
#52608=CARTESIAN_POINT('',(69.81,38.0787611019615,41.5));
#52609=CARTESIAN_POINT('Origin',(69.81,38.0787611019615,43.));
#52610=CARTESIAN_POINT('',(70.61,38.0787611019615,41.5));
#52611=CARTESIAN_POINT('',(60.61,38.0787611019615,41.5));
#52612=CARTESIAN_POINT('',(70.61,38.0787611019615,44.5));
#52613=CARTESIAN_POINT('Origin',(70.61,38.0787611019615,43.));
#52614=CARTESIAN_POINT('',(60.61,38.0787611019615,44.5));
#52615=CARTESIAN_POINT('Origin',(60.61,38.0787611019615,48.));
#52616=CARTESIAN_POINT('',(69.81,38.0787611019615,49.5));
#52617=CARTESIAN_POINT('',(69.81,38.0787611019615,46.5));
#52618=CARTESIAN_POINT('Origin',(69.81,38.0787611019615,48.));
#52619=CARTESIAN_POINT('',(70.61,38.0787611019615,46.5));
#52620=CARTESIAN_POINT('',(60.61,38.0787611019615,46.5));
#52621=CARTESIAN_POINT('',(70.61,38.0787611019615,49.5));
#52622=CARTESIAN_POINT('Origin',(70.61,38.0787611019615,48.));
#52623=CARTESIAN_POINT('',(60.61,38.0787611019615,49.5));
#52624=CARTESIAN_POINT('Origin',(60.61,38.0787611019615,53.));
#52625=CARTESIAN_POINT('',(69.81,38.0787611019615,54.5));
#52626=CARTESIAN_POINT('',(69.81,38.0787611019615,51.5));
#52627=CARTESIAN_POINT('Origin',(69.81,38.0787611019615,53.));
#52628=CARTESIAN_POINT('',(70.61,38.0787611019615,51.5));
#52629=CARTESIAN_POINT('',(60.61,38.0787611019615,51.5));
#52630=CARTESIAN_POINT('',(70.61,38.0787611019615,54.5));
#52631=CARTESIAN_POINT('Origin',(70.61,38.0787611019615,53.));
#52632=CARTESIAN_POINT('',(60.61,38.0787611019615,54.5));
#52633=CARTESIAN_POINT('Origin',(60.61,38.0787611019615,13.));
#52634=CARTESIAN_POINT('',(69.81,38.0787611019615,14.5));
#52635=CARTESIAN_POINT('',(69.81,38.0787611019615,11.5));
#52636=CARTESIAN_POINT('Origin',(69.81,38.0787611019615,13.));
#52637=CARTESIAN_POINT('',(70.61,38.0787611019615,11.5));
#52638=CARTESIAN_POINT('',(60.61,38.0787611019615,11.5));
#52639=CARTESIAN_POINT('',(70.61,38.0787611019615,14.5));
#52640=CARTESIAN_POINT('Origin',(70.61,38.0787611019615,13.));
#52641=CARTESIAN_POINT('',(60.61,38.0787611019615,14.5));
#52642=CARTESIAN_POINT('Origin',(60.61,66.0787611019615,13.));
#52643=CARTESIAN_POINT('',(69.81,66.0787611019615,11.5));
#52644=CARTESIAN_POINT('',(69.81,66.0787611019615,14.5));
#52645=CARTESIAN_POINT('Origin',(69.81,66.0787611019615,13.));
#52646=CARTESIAN_POINT('',(70.61,66.0787611019615,11.5));
#52647=CARTESIAN_POINT('',(60.61,66.0787611019615,11.5));
#52648=CARTESIAN_POINT('',(70.61,66.0787611019615,14.5));
#52649=CARTESIAN_POINT('Origin',(70.61,66.0787611019615,13.));
#52650=CARTESIAN_POINT('',(60.61,66.0787611019615,14.5));
#52651=CARTESIAN_POINT('Origin',(60.61,66.0787611019615,18.));
#52652=CARTESIAN_POINT('',(69.81,66.0787611019615,16.5));
#52653=CARTESIAN_POINT('',(69.81,66.0787611019615,19.5));
#52654=CARTESIAN_POINT('Origin',(69.81,66.0787611019615,18.));
#52655=CARTESIAN_POINT('',(70.61,66.0787611019615,16.5));
#52656=CARTESIAN_POINT('',(60.61,66.0787611019615,16.5));
#52657=CARTESIAN_POINT('',(70.61,66.0787611019615,19.5));
#52658=CARTESIAN_POINT('Origin',(70.61,66.0787611019615,18.));
#52659=CARTESIAN_POINT('',(60.61,66.0787611019615,19.5));
#52660=CARTESIAN_POINT('Origin',(60.61,38.0787611019615,28.));
#52661=CARTESIAN_POINT('',(69.81,38.0787611019615,29.5));
#52662=CARTESIAN_POINT('',(69.81,38.0787611019615,26.5));
#52663=CARTESIAN_POINT('Origin',(69.81,38.0787611019615,28.));
#52664=CARTESIAN_POINT('',(70.61,38.0787611019615,26.5));
#52665=CARTESIAN_POINT('',(60.61,38.0787611019615,26.5));
#52666=CARTESIAN_POINT('',(70.61,38.0787611019615,29.5));
#52667=CARTESIAN_POINT('Origin',(70.61,38.0787611019615,28.));
#52668=CARTESIAN_POINT('',(60.61,38.0787611019615,29.5));
#52669=CARTESIAN_POINT('Origin',(60.61,66.0787611019615,23.));
#52670=CARTESIAN_POINT('',(69.81,66.0787611019615,21.5));
#52671=CARTESIAN_POINT('',(69.81,66.0787611019615,24.5));
#52672=CARTESIAN_POINT('Origin',(69.81,66.0787611019615,23.));
#52673=CARTESIAN_POINT('',(70.61,66.0787611019615,21.5));
#52674=CARTESIAN_POINT('',(60.61,66.0787611019615,21.5));
#52675=CARTESIAN_POINT('',(70.61,66.0787611019615,24.5));
#52676=CARTESIAN_POINT('Origin',(70.61,66.0787611019615,23.));
#52677=CARTESIAN_POINT('',(60.61,66.0787611019615,24.5));
#52678=CARTESIAN_POINT('Origin',(60.61,38.0787611019615,23.));
#52679=CARTESIAN_POINT('',(69.81,38.0787611019615,24.5));
#52680=CARTESIAN_POINT('',(69.81,38.0787611019615,21.5));
#52681=CARTESIAN_POINT('Origin',(69.81,38.0787611019615,23.));
#52682=CARTESIAN_POINT('',(70.61,38.0787611019615,21.5));
#52683=CARTESIAN_POINT('',(60.61,38.0787611019615,21.5));
#52684=CARTESIAN_POINT('',(70.61,38.0787611019615,24.5));
#52685=CARTESIAN_POINT('Origin',(70.61,38.0787611019615,23.));
#52686=CARTESIAN_POINT('',(60.61,38.0787611019615,24.5));
#52687=CARTESIAN_POINT('Origin',(60.61,38.0787611019615,18.));
#52688=CARTESIAN_POINT('',(69.81,38.0787611019615,19.5));
#52689=CARTESIAN_POINT('',(69.81,38.0787611019615,16.5));
#52690=CARTESIAN_POINT('Origin',(69.81,38.0787611019615,18.));
#52691=CARTESIAN_POINT('',(70.61,38.0787611019615,16.5));
#52692=CARTESIAN_POINT('',(60.61,38.0787611019615,16.5));
#52693=CARTESIAN_POINT('',(70.61,38.0787611019615,19.5));
#52694=CARTESIAN_POINT('Origin',(70.61,38.0787611019615,18.));
#52695=CARTESIAN_POINT('',(60.61,38.0787611019615,19.5));
#52696=CARTESIAN_POINT('Origin',(60.61,66.0787611019615,68.));
#52697=CARTESIAN_POINT('',(69.81,66.0787611019615,66.5));
#52698=CARTESIAN_POINT('',(69.81,66.0787611019615,69.5));
#52699=CARTESIAN_POINT('Origin',(69.81,66.0787611019615,68.));
#52700=CARTESIAN_POINT('',(70.61,66.0787611019615,66.5));
#52701=CARTESIAN_POINT('',(60.61,66.0787611019615,66.5));
#52702=CARTESIAN_POINT('',(70.61,66.0787611019615,69.5));
#52703=CARTESIAN_POINT('Origin',(70.61,66.0787611019615,68.));
#52704=CARTESIAN_POINT('',(60.61,66.0787611019615,69.5));
#52705=CARTESIAN_POINT('Origin',(60.61,66.0787611019615,-38.));
#52706=CARTESIAN_POINT('',(69.81,66.0787611019615,-36.5));
#52707=CARTESIAN_POINT('',(69.81,66.0787611019615,-39.5));
#52708=CARTESIAN_POINT('Origin',(69.81,66.0787611019615,-38.));
#52709=CARTESIAN_POINT('',(70.61,66.0787611019615,-39.5));
#52710=CARTESIAN_POINT('',(60.61,66.0787611019615,-39.5));
#52711=CARTESIAN_POINT('',(70.61,66.0787611019615,-36.5));
#52712=CARTESIAN_POINT('Origin',(70.61,66.0787611019615,-38.));
#52713=CARTESIAN_POINT('',(60.61,66.0787611019615,-36.5));
#52714=CARTESIAN_POINT('Origin',(60.61,38.0787611019615,-68.));
#52715=CARTESIAN_POINT('',(69.81,38.0787611019615,-69.5));
#52716=CARTESIAN_POINT('',(69.81,38.0787611019615,-66.5));
#52717=CARTESIAN_POINT('Origin',(69.81,38.0787611019615,-68.));
#52718=CARTESIAN_POINT('',(70.61,38.0787611019615,-69.5));
#52719=CARTESIAN_POINT('',(60.61,38.0787611019615,-69.5));
#52720=CARTESIAN_POINT('',(70.61,38.0787611019615,-66.5));
#52721=CARTESIAN_POINT('Origin',(70.61,38.0787611019615,-68.));
#52722=CARTESIAN_POINT('',(60.61,38.0787611019615,-66.5));
#52723=CARTESIAN_POINT('Origin',(60.61,38.0787611019615,-63.));
#52724=CARTESIAN_POINT('',(69.81,38.0787611019615,-64.5));
#52725=CARTESIAN_POINT('',(69.81,38.0787611019615,-61.5));
#52726=CARTESIAN_POINT('Origin',(69.81,38.0787611019615,-63.));
#52727=CARTESIAN_POINT('',(70.61,38.0787611019615,-64.5));
#52728=CARTESIAN_POINT('',(60.61,38.0787611019615,-64.5));
#52729=CARTESIAN_POINT('',(70.61,38.0787611019615,-61.5));
#52730=CARTESIAN_POINT('Origin',(70.61,38.0787611019615,-63.));
#52731=CARTESIAN_POINT('',(60.61,38.0787611019615,-61.5));
#52732=CARTESIAN_POINT('Origin',(60.61,38.0787611019615,-58.));
#52733=CARTESIAN_POINT('',(69.81,38.0787611019615,-59.5));
#52734=CARTESIAN_POINT('',(69.81,38.0787611019615,-56.5));
#52735=CARTESIAN_POINT('Origin',(69.81,38.0787611019615,-58.));
#52736=CARTESIAN_POINT('',(70.61,38.0787611019615,-59.5));
#52737=CARTESIAN_POINT('',(60.61,38.0787611019615,-59.5));
#52738=CARTESIAN_POINT('',(70.61,38.0787611019615,-56.5));
#52739=CARTESIAN_POINT('Origin',(70.61,38.0787611019615,-58.));
#52740=CARTESIAN_POINT('',(60.61,38.0787611019615,-56.5));
#52741=CARTESIAN_POINT('Origin',(60.61,38.0787611019615,-38.));
#52742=CARTESIAN_POINT('',(69.81,38.0787611019615,-39.5));
#52743=CARTESIAN_POINT('',(69.81,38.0787611019615,-36.5));
#52744=CARTESIAN_POINT('Origin',(69.81,38.0787611019615,-38.));
#52745=CARTESIAN_POINT('',(70.61,38.0787611019615,-39.5));
#52746=CARTESIAN_POINT('',(60.61,38.0787611019615,-39.5));
#52747=CARTESIAN_POINT('',(70.61,38.0787611019615,-36.5));
#52748=CARTESIAN_POINT('Origin',(70.61,38.0787611019615,-38.));
#52749=CARTESIAN_POINT('',(60.61,38.0787611019615,-36.5));
#52750=CARTESIAN_POINT('Origin',(60.61,38.0787611019615,-33.));
#52751=CARTESIAN_POINT('',(69.81,38.0787611019615,-34.5));
#52752=CARTESIAN_POINT('',(69.81,38.0787611019615,-31.5));
#52753=CARTESIAN_POINT('Origin',(69.81,38.0787611019615,-33.));
#52754=CARTESIAN_POINT('',(70.61,38.0787611019615,-34.5));
#52755=CARTESIAN_POINT('',(60.61,38.0787611019615,-34.5));
#52756=CARTESIAN_POINT('',(70.61,38.0787611019615,-31.5));
#52757=CARTESIAN_POINT('Origin',(70.61,38.0787611019615,-33.));
#52758=CARTESIAN_POINT('',(60.61,38.0787611019615,-31.5));
#52759=CARTESIAN_POINT('Origin',(60.61,66.0787611019615,-33.));
#52760=CARTESIAN_POINT('',(69.81,66.0787611019615,-31.5));
#52761=CARTESIAN_POINT('',(69.81,66.0787611019615,-34.5));
#52762=CARTESIAN_POINT('Origin',(69.81,66.0787611019615,-33.));
#52763=CARTESIAN_POINT('',(70.61,66.0787611019615,-34.5));
#52764=CARTESIAN_POINT('',(60.61,66.0787611019615,-34.5));
#52765=CARTESIAN_POINT('',(70.61,66.0787611019615,-31.5));
#52766=CARTESIAN_POINT('Origin',(70.61,66.0787611019615,-33.));
#52767=CARTESIAN_POINT('',(60.61,66.0787611019615,-31.5));
#52768=CARTESIAN_POINT('Origin',(60.61,66.0787611019615,-28.));
#52769=CARTESIAN_POINT('',(69.81,66.0787611019615,-26.5));
#52770=CARTESIAN_POINT('',(69.81,66.0787611019615,-29.5));
#52771=CARTESIAN_POINT('Origin',(69.81,66.0787611019615,-28.));
#52772=CARTESIAN_POINT('',(70.61,66.0787611019615,-29.5));
#52773=CARTESIAN_POINT('',(60.61,66.0787611019615,-29.5));
#52774=CARTESIAN_POINT('',(70.61,66.0787611019615,-26.5));
#52775=CARTESIAN_POINT('Origin',(70.61,66.0787611019615,-28.));
#52776=CARTESIAN_POINT('',(60.61,66.0787611019615,-26.5));
#52777=CARTESIAN_POINT('Origin',(60.61,66.0787611019615,-63.));
#52778=CARTESIAN_POINT('',(69.81,66.0787611019615,-61.5));
#52779=CARTESIAN_POINT('',(69.81,66.0787611019615,-64.5));
#52780=CARTESIAN_POINT('Origin',(69.81,66.0787611019615,-63.));
#52781=CARTESIAN_POINT('',(70.61,66.0787611019615,-64.5));
#52782=CARTESIAN_POINT('',(60.61,66.0787611019615,-64.5));
#52783=CARTESIAN_POINT('',(70.61,66.0787611019615,-61.5));
#52784=CARTESIAN_POINT('Origin',(70.61,66.0787611019615,-63.));
#52785=CARTESIAN_POINT('',(60.61,66.0787611019615,-61.5));
#52786=CARTESIAN_POINT('Origin',(60.61,66.0787611019615,-58.));
#52787=CARTESIAN_POINT('',(69.81,66.0787611019615,-56.5));
#52788=CARTESIAN_POINT('',(69.81,66.0787611019615,-59.5));
#52789=CARTESIAN_POINT('Origin',(69.81,66.0787611019615,-58.));
#52790=CARTESIAN_POINT('',(70.61,66.0787611019615,-59.5));
#52791=CARTESIAN_POINT('',(60.61,66.0787611019615,-59.5));
#52792=CARTESIAN_POINT('',(70.61,66.0787611019615,-56.5));
#52793=CARTESIAN_POINT('Origin',(70.61,66.0787611019615,-58.));
#52794=CARTESIAN_POINT('',(60.61,66.0787611019615,-56.5));
#52795=CARTESIAN_POINT('Origin',(60.61,66.0787611019615,-53.));
#52796=CARTESIAN_POINT('',(69.81,66.0787611019615,-51.5));
#52797=CARTESIAN_POINT('',(69.81,66.0787611019615,-54.5));
#52798=CARTESIAN_POINT('Origin',(69.81,66.0787611019615,-53.));
#52799=CARTESIAN_POINT('',(70.61,66.0787611019615,-54.5));
#52800=CARTESIAN_POINT('',(60.61,66.0787611019615,-54.5));
#52801=CARTESIAN_POINT('',(70.61,66.0787611019615,-51.5));
#52802=CARTESIAN_POINT('Origin',(70.61,66.0787611019615,-53.));
#52803=CARTESIAN_POINT('',(60.61,66.0787611019615,-51.5));
#52804=CARTESIAN_POINT('Origin',(60.61,66.0787611019615,-48.));
#52805=CARTESIAN_POINT('',(69.81,66.0787611019615,-46.5));
#52806=CARTESIAN_POINT('',(69.81,66.0787611019615,-49.5));
#52807=CARTESIAN_POINT('Origin',(69.81,66.0787611019615,-48.));
#52808=CARTESIAN_POINT('',(70.61,66.0787611019615,-49.5));
#52809=CARTESIAN_POINT('',(60.61,66.0787611019615,-49.5));
#52810=CARTESIAN_POINT('',(70.61,66.0787611019615,-46.5));
#52811=CARTESIAN_POINT('Origin',(70.61,66.0787611019615,-48.));
#52812=CARTESIAN_POINT('',(60.61,66.0787611019615,-46.5));
#52813=CARTESIAN_POINT('Origin',(60.61,66.0787611019615,-43.));
#52814=CARTESIAN_POINT('',(69.81,66.0787611019615,-41.5));
#52815=CARTESIAN_POINT('',(69.81,66.0787611019615,-44.5));
#52816=CARTESIAN_POINT('Origin',(69.81,66.0787611019615,-43.));
#52817=CARTESIAN_POINT('',(70.61,66.0787611019615,-44.5));
#52818=CARTESIAN_POINT('',(60.61,66.0787611019615,-44.5));
#52819=CARTESIAN_POINT('',(70.61,66.0787611019615,-41.5));
#52820=CARTESIAN_POINT('Origin',(70.61,66.0787611019615,-43.));
#52821=CARTESIAN_POINT('',(60.61,66.0787611019615,-41.5));
#52822=CARTESIAN_POINT('Origin',(60.61,38.0787611019615,-43.));
#52823=CARTESIAN_POINT('',(69.81,38.0787611019615,-44.5));
#52824=CARTESIAN_POINT('',(69.81,38.0787611019615,-41.5));
#52825=CARTESIAN_POINT('Origin',(69.81,38.0787611019615,-43.));
#52826=CARTESIAN_POINT('',(70.61,38.0787611019615,-44.5));
#52827=CARTESIAN_POINT('',(60.61,38.0787611019615,-44.5));
#52828=CARTESIAN_POINT('',(70.61,38.0787611019615,-41.5));
#52829=CARTESIAN_POINT('Origin',(70.61,38.0787611019615,-43.));
#52830=CARTESIAN_POINT('',(60.61,38.0787611019615,-41.5));
#52831=CARTESIAN_POINT('Origin',(60.61,38.0787611019615,-48.));
#52832=CARTESIAN_POINT('',(69.81,38.0787611019615,-49.5));
#52833=CARTESIAN_POINT('',(69.81,38.0787611019615,-46.5));
#52834=CARTESIAN_POINT('Origin',(69.81,38.0787611019615,-48.));
#52835=CARTESIAN_POINT('',(70.61,38.0787611019615,-49.5));
#52836=CARTESIAN_POINT('',(60.61,38.0787611019615,-49.5));
#52837=CARTESIAN_POINT('',(70.61,38.0787611019615,-46.5));
#52838=CARTESIAN_POINT('Origin',(70.61,38.0787611019615,-48.));
#52839=CARTESIAN_POINT('',(60.61,38.0787611019615,-46.5));
#52840=CARTESIAN_POINT('Origin',(60.61,38.0787611019615,-53.));
#52841=CARTESIAN_POINT('',(69.81,38.0787611019615,-54.5));
#52842=CARTESIAN_POINT('',(69.81,38.0787611019615,-51.5));
#52843=CARTESIAN_POINT('Origin',(69.81,38.0787611019615,-53.));
#52844=CARTESIAN_POINT('',(70.61,38.0787611019615,-54.5));
#52845=CARTESIAN_POINT('',(60.61,38.0787611019615,-54.5));
#52846=CARTESIAN_POINT('',(70.61,38.0787611019615,-51.5));
#52847=CARTESIAN_POINT('Origin',(70.61,38.0787611019615,-53.));
#52848=CARTESIAN_POINT('',(60.61,38.0787611019615,-51.5));
#52849=CARTESIAN_POINT('Origin',(60.61,38.0787611019615,-13.));
#52850=CARTESIAN_POINT('',(69.81,38.0787611019615,-14.5));
#52851=CARTESIAN_POINT('',(69.81,38.0787611019615,-11.5));
#52852=CARTESIAN_POINT('Origin',(69.81,38.0787611019615,-13.));
#52853=CARTESIAN_POINT('',(70.61,38.0787611019615,-14.5));
#52854=CARTESIAN_POINT('',(60.61,38.0787611019615,-14.5));
#52855=CARTESIAN_POINT('',(70.61,38.0787611019615,-11.5));
#52856=CARTESIAN_POINT('Origin',(70.61,38.0787611019615,-13.));
#52857=CARTESIAN_POINT('',(60.61,38.0787611019615,-11.5));
#52858=CARTESIAN_POINT('Origin',(60.61,66.0787611019615,-13.));
#52859=CARTESIAN_POINT('',(69.81,66.0787611019615,-11.5));
#52860=CARTESIAN_POINT('',(69.81,66.0787611019615,-14.5));
#52861=CARTESIAN_POINT('Origin',(69.81,66.0787611019615,-13.));
#52862=CARTESIAN_POINT('',(70.61,66.0787611019615,-14.5));
#52863=CARTESIAN_POINT('',(60.61,66.0787611019615,-14.5));
#52864=CARTESIAN_POINT('',(70.61,66.0787611019615,-11.5));
#52865=CARTESIAN_POINT('Origin',(70.61,66.0787611019615,-13.));
#52866=CARTESIAN_POINT('',(60.61,66.0787611019615,-11.5));
#52867=CARTESIAN_POINT('Origin',(60.61,66.0787611019615,-18.));
#52868=CARTESIAN_POINT('',(69.81,66.0787611019615,-16.5));
#52869=CARTESIAN_POINT('',(69.81,66.0787611019615,-19.5));
#52870=CARTESIAN_POINT('Origin',(69.81,66.0787611019615,-18.));
#52871=CARTESIAN_POINT('',(70.61,66.0787611019615,-19.5));
#52872=CARTESIAN_POINT('',(60.61,66.0787611019615,-19.5));
#52873=CARTESIAN_POINT('',(70.61,66.0787611019615,-16.5));
#52874=CARTESIAN_POINT('Origin',(70.61,66.0787611019615,-18.));
#52875=CARTESIAN_POINT('',(60.61,66.0787611019615,-16.5));
#52876=CARTESIAN_POINT('Origin',(60.61,38.0787611019615,-28.));
#52877=CARTESIAN_POINT('',(69.81,38.0787611019615,-29.5));
#52878=CARTESIAN_POINT('',(69.81,38.0787611019615,-26.5));
#52879=CARTESIAN_POINT('Origin',(69.81,38.0787611019615,-28.));
#52880=CARTESIAN_POINT('',(70.61,38.0787611019615,-29.5));
#52881=CARTESIAN_POINT('',(60.61,38.0787611019615,-29.5));
#52882=CARTESIAN_POINT('',(70.61,38.0787611019615,-26.5));
#52883=CARTESIAN_POINT('Origin',(70.61,38.0787611019615,-28.));
#52884=CARTESIAN_POINT('',(60.61,38.0787611019615,-26.5));
#52885=CARTESIAN_POINT('Origin',(60.61,66.0787611019615,-23.));
#52886=CARTESIAN_POINT('',(69.81,66.0787611019615,-21.5));
#52887=CARTESIAN_POINT('',(69.81,66.0787611019615,-24.5));
#52888=CARTESIAN_POINT('Origin',(69.81,66.0787611019615,-23.));
#52889=CARTESIAN_POINT('',(70.61,66.0787611019615,-24.5));
#52890=CARTESIAN_POINT('',(60.61,66.0787611019615,-24.5));
#52891=CARTESIAN_POINT('',(70.61,66.0787611019615,-21.5));
#52892=CARTESIAN_POINT('Origin',(70.61,66.0787611019615,-23.));
#52893=CARTESIAN_POINT('',(60.61,66.0787611019615,-21.5));
#52894=CARTESIAN_POINT('Origin',(60.61,38.0787611019615,-23.));
#52895=CARTESIAN_POINT('',(69.81,38.0787611019615,-24.5));
#52896=CARTESIAN_POINT('',(69.81,38.0787611019615,-21.5));
#52897=CARTESIAN_POINT('Origin',(69.81,38.0787611019615,-23.));
#52898=CARTESIAN_POINT('',(70.61,38.0787611019615,-24.5));
#52899=CARTESIAN_POINT('',(60.61,38.0787611019615,-24.5));
#52900=CARTESIAN_POINT('',(70.61,38.0787611019615,-21.5));
#52901=CARTESIAN_POINT('Origin',(70.61,38.0787611019615,-23.));
#52902=CARTESIAN_POINT('',(60.61,38.0787611019615,-21.5));
#52903=CARTESIAN_POINT('Origin',(60.61,38.0787611019615,-18.));
#52904=CARTESIAN_POINT('',(69.81,38.0787611019615,-19.5));
#52905=CARTESIAN_POINT('',(69.81,38.0787611019615,-16.5));
#52906=CARTESIAN_POINT('Origin',(69.81,38.0787611019615,-18.));
#52907=CARTESIAN_POINT('',(70.61,38.0787611019615,-19.5));
#52908=CARTESIAN_POINT('',(60.61,38.0787611019615,-19.5));
#52909=CARTESIAN_POINT('',(70.61,38.0787611019615,-16.5));
#52910=CARTESIAN_POINT('Origin',(70.61,38.0787611019615,-18.));
#52911=CARTESIAN_POINT('',(60.61,38.0787611019615,-16.5));
#52912=CARTESIAN_POINT('Origin',(60.61,66.0787611019615,-68.));
#52913=CARTESIAN_POINT('',(69.81,66.0787611019615,-66.5));
#52914=CARTESIAN_POINT('',(69.81,66.0787611019615,-69.5));
#52915=CARTESIAN_POINT('Origin',(69.81,66.0787611019615,-68.));
#52916=CARTESIAN_POINT('',(70.61,66.0787611019615,-69.5));
#52917=CARTESIAN_POINT('',(60.61,66.0787611019615,-69.5));
#52918=CARTESIAN_POINT('',(70.61,66.0787611019615,-66.5));
#52919=CARTESIAN_POINT('Origin',(70.61,66.0787611019615,-68.));
#52920=CARTESIAN_POINT('',(60.61,66.0787611019615,-66.5));
#52921=CARTESIAN_POINT('Origin',(-85.9899999999996,51.6837646578732,-23.6937728532034));
#52922=CARTESIAN_POINT('',(-85.5900000000003,50.5618748736031,-24.689445144648));
#52923=CARTESIAN_POINT('',(-85.5900000000001,50.3847265521965,-22.9437728532035));
#52924=CARTESIAN_POINT('Origin',(-85.59,51.6837646578732,-23.6937728532034));
#52925=CARTESIAN_POINT('',(-86.39,50.5618748740111,-24.6894451438606));
#52926=CARTESIAN_POINT('',(-86.3899999999996,50.5618748736031,-24.689445144648));
#52927=CARTESIAN_POINT('',(-86.39,50.3847265521965,-22.9437728532035));
#52928=CARTESIAN_POINT('Origin',(-86.39,51.6837646578732,-23.6937728532034));
#52929=CARTESIAN_POINT('',(-86.3899999999997,50.3847265521965,-22.9437728532035));
#52930=CARTESIAN_POINT('Origin',(-85.9899999999996,51.6837646578732,-36.3062271467966));
#52931=CARTESIAN_POINT('',(-85.5900000000001,50.3847265521965,-37.0562271467966));
#52932=CARTESIAN_POINT('',(-85.5900000000003,50.5618748736031,-35.310554855352));
#52933=CARTESIAN_POINT('Origin',(-85.59,51.6837646578732,-36.3062271467966));
#52934=CARTESIAN_POINT('',(-86.39,50.3847265521965,-37.0562271467966));
#52935=CARTESIAN_POINT('',(-85.5899999999991,50.3847265521965,-37.0562271467966));
#52936=CARTESIAN_POINT('',(-86.39,50.5618748739028,-35.3105548560302));
#52937=CARTESIAN_POINT('Origin',(-86.39,51.6837646578732,-36.3062271467966));
#52938=CARTESIAN_POINT('',(-85.5900000000004,50.5618748736031,-35.310554855352));
#52939=CARTESIAN_POINT('Origin',(-85.9899999999998,28.8625290471562,-27.));
#52940=CARTESIAN_POINT('',(-85.5900000000001,28.8625290471562,-28.5));
#52941=CARTESIAN_POINT('',(-85.5900000000002,27.3891253349642,-26.7187856673305));
#52942=CARTESIAN_POINT('Origin',(-85.59,28.8625290471562,-27.));
#52943=CARTESIAN_POINT('',(-86.39,28.8625290471562,-28.5));
#52944=CARTESIAN_POINT('',(-85.5899999999995,28.8625290471562,-28.5));
#52945=CARTESIAN_POINT('',(-86.39,27.3891253344444,-26.7187856670729));
#52946=CARTESIAN_POINT('Origin',(-86.39,28.8625290471562,-27.));
#52947=CARTESIAN_POINT('',(-85.5900000000002,27.3891253349642,-26.7187856673305));
#52948=CARTESIAN_POINT('Origin',(-85.9899999999998,28.8625290471562,-33.));
#52949=CARTESIAN_POINT('',(-85.5900000000001,27.3891253349642,-33.2812143326694));
#52950=CARTESIAN_POINT('',(-85.5900000000001,28.8625290471562,-31.5));
#52951=CARTESIAN_POINT('Origin',(-85.59,28.8625290471562,-33.));
#52952=CARTESIAN_POINT('',(-86.39,27.3891253342258,-33.2812143328545));
#52953=CARTESIAN_POINT('',(-86.39,27.3891253349642,-33.2812143326695));
#52954=CARTESIAN_POINT('',(-86.39,28.8625290471562,-31.5));
#52955=CARTESIAN_POINT('Origin',(-86.39,28.8625290471562,-33.));
#52956=CARTESIAN_POINT('',(-86.3900000000002,28.8625290471562,-31.5));
#52957=CARTESIAN_POINT('Origin',(-85.9899999999998,39.3187444720575,-45.1106160516509));
#52958=CARTESIAN_POINT('',(-85.59,38.8257009268133,-46.5272698775706));
#52959=CARTESIAN_POINT('',(-85.5900000000001,38.0197063663809,-44.3606160516509));
#52960=CARTESIAN_POINT('Origin',(-85.59,39.3187444720575,-45.1106160516509));
#52961=CARTESIAN_POINT('',(-86.39,38.825700926233,-46.5272698779012));
#52962=CARTESIAN_POINT('',(-86.3900000000002,38.8257009268133,-46.5272698775706));
#52963=CARTESIAN_POINT('',(-86.39,38.0197063663809,-44.3606160516509));
#52964=CARTESIAN_POINT('Origin',(-86.39,39.3187444720575,-45.1106160516509));
#52965=CARTESIAN_POINT('',(-86.3900000000002,38.0197063663809,-44.3606160516509));
#52966=CARTESIAN_POINT('Origin',(-85.9899999999998,39.3187444720576,-14.8893839483491));
#52967=CARTESIAN_POINT('',(-85.5900000000001,38.0197063663809,-15.6393839483491));
#52968=CARTESIAN_POINT('',(-85.59,38.8257009268133,-13.4727301224294));
#52969=CARTESIAN_POINT('Origin',(-85.59,39.3187444720576,-14.8893839483491));
#52970=CARTESIAN_POINT('',(-86.39,38.0197063663809,-15.6393839483491));
#52971=CARTESIAN_POINT('',(-85.5899999999993,38.0197063663809,-15.6393839483491));
#52972=CARTESIAN_POINT('',(-86.3900000000001,38.8257009252949,-13.4727301229578));
#52973=CARTESIAN_POINT('Origin',(-86.39,39.3187444720576,-14.8893839483491));
#52974=CARTESIAN_POINT('',(-85.5900000000001,38.8257009268133,-13.4727301224294));
#52975=CARTESIAN_POINT('Origin',(-85.9899999999998,58.0740500613155,-12.6254738595756));
#52976=CARTESIAN_POINT('',(-85.5900000000001,57.1538693431447,-13.8100697594109));
#52977=CARTESIAN_POINT('',(-85.5900000000001,56.7750119556388,-11.8754738595756));
#52978=CARTESIAN_POINT('Origin',(-85.59,58.0740500613155,-12.6254738595756));
#52979=CARTESIAN_POINT('',(-86.39,57.1538693432358,-13.8100697584817));
#52980=CARTESIAN_POINT('',(-86.3900000000001,57.1538693431447,-13.8100697594109));
#52981=CARTESIAN_POINT('',(-86.39,56.7750119556388,-11.8754738595756));
#52982=CARTESIAN_POINT('Origin',(-86.39,58.0740500613155,-12.6254738595756));
#52983=CARTESIAN_POINT('',(-86.3900000000001,56.7750119556388,-11.8754738595756));
#52984=CARTESIAN_POINT('Origin',(-85.9899999999996,58.0740500613155,-47.3745261404244));
#52985=CARTESIAN_POINT('',(-85.5900000000001,56.7750119556388,-48.1245261404244));
#52986=CARTESIAN_POINT('',(-85.59,57.1538693431447,-46.1899302405891));
#52987=CARTESIAN_POINT('Origin',(-85.59,58.0740500613155,-47.3745261404244));
#52988=CARTESIAN_POINT('',(-86.39,56.7750119556388,-48.1245261404244));
#52989=CARTESIAN_POINT('',(-85.5899999999992,56.7750119556388,-48.1245261404244));
#52990=CARTESIAN_POINT('',(-86.39,57.1538693431799,-46.1899302415125));
#52991=CARTESIAN_POINT('Origin',(-86.39,58.0740500613155,-47.3745261404244));
#52992=CARTESIAN_POINT('',(-85.59,57.1538693431447,-46.1899302405891));
#52993=CARTESIAN_POINT('Origin',(-85.9899999999995,16.7400532252403,-27.));
#52994=CARTESIAN_POINT('',(-85.5900000000001,16.7400532252403,-28.5));
#52995=CARTESIAN_POINT('',(-85.59,15.2486853399007,-26.8393082747068));
#52996=CARTESIAN_POINT('Origin',(-85.59,16.7400532252403,-27.));
#52997=CARTESIAN_POINT('',(-86.39,16.7400532252403,-28.5));
#52998=CARTESIAN_POINT('',(-85.5899999999992,16.7400532252403,-28.5));
#52999=CARTESIAN_POINT('',(-86.39,15.2486853393764,-26.8393082746143));
#53000=CARTESIAN_POINT('Origin',(-86.39,16.7400532252403,-27.));
#53001=CARTESIAN_POINT('',(-85.5900000000001,15.2486853399007,-26.8393082747068));
#53002=CARTESIAN_POINT('Origin',(-85.9899999999995,16.7400532252403,-33.));
#53003=CARTESIAN_POINT('',(-85.59,15.2486853399007,-33.1606917252932));
#53004=CARTESIAN_POINT('',(-85.5900000000001,16.7400532252403,-31.5));
#53005=CARTESIAN_POINT('Origin',(-85.59,16.7400532252403,-33.));
#53006=CARTESIAN_POINT('',(-86.39,15.2486853407812,-33.1606917252392));
#53007=CARTESIAN_POINT('',(-86.3899999999997,15.2486853399007,-33.1606917252932));
#53008=CARTESIAN_POINT('',(-86.39,16.7400532252403,-31.5));
#53009=CARTESIAN_POINT('Origin',(-86.39,16.7400532252403,-33.));
#53010=CARTESIAN_POINT('',(-86.3899999999997,16.7400532252403,-31.5));
#53011=CARTESIAN_POINT('Origin',(-85.9899999999996,33.2574367244157,-55.6091090308774));
#53012=CARTESIAN_POINT('',(-85.59,32.6508629759236,-56.980993970528));
#53013=CARTESIAN_POINT('',(-85.5900000000001,31.9583986187391,-54.8591090308774));
#53014=CARTESIAN_POINT('Origin',(-85.59,33.2574367244157,-55.6091090308774));
#53015=CARTESIAN_POINT('',(-86.39,32.6508629762386,-56.9809939712314));
#53016=CARTESIAN_POINT('',(-86.3899999999996,32.6508629759238,-56.9809939705281));
#53017=CARTESIAN_POINT('',(-86.39,31.9583986187391,-54.8591090308774));
#53018=CARTESIAN_POINT('Origin',(-86.39,33.2574367244157,-55.6091090308774));
#53019=CARTESIAN_POINT('',(-86.3899999999997,31.9583986187391,-54.8591090308774));
#53020=CARTESIAN_POINT('Origin',(-85.9899999999995,33.2574367244158,-4.3908909691226));
#53021=CARTESIAN_POINT('',(-85.5900000000001,31.9583986187391,-5.14089096912259));
#53022=CARTESIAN_POINT('',(-85.59,32.6508629759237,-3.01900602947195));
#53023=CARTESIAN_POINT('Origin',(-85.59,33.2574367244158,-4.3908909691226));
#53024=CARTESIAN_POINT('',(-86.39,31.9583986187391,-5.14089096912259));
#53025=CARTESIAN_POINT('',(-85.5899999999992,31.9583986187391,-5.1408909691226));
#53026=CARTESIAN_POINT('',(-86.39,32.6508629756065,-3.01900602877295));
#53027=CARTESIAN_POINT('Origin',(-86.39,33.2574367244158,-4.3908909691226));
#53028=CARTESIAN_POINT('',(-85.5900000000001,32.6508629759238,-3.0190060294719));
#53029=CARTESIAN_POINT('Origin',(-85.9899999999993,64.1105207282856,-2.16999996598415));
#53030=CARTESIAN_POINT('',(-85.5899999999999,63.2487659305948,-3.39775347082817));
#53031=CARTESIAN_POINT('',(-85.5900000000001,62.811482622609,-1.41999996598415));
#53032=CARTESIAN_POINT('Origin',(-85.59,64.1105207282856,-2.16999996598415));
#53033=CARTESIAN_POINT('',(-86.39,63.2487659307941,-3.39775346999418));
#53034=CARTESIAN_POINT('',(-86.39,63.2487659305948,-3.39775347082816));
#53035=CARTESIAN_POINT('',(-86.39,62.811482622609,-1.41999996598415));
#53036=CARTESIAN_POINT('Origin',(-86.39,64.1105207282856,-2.16999996598415));
#53037=CARTESIAN_POINT('',(-86.3899999999996,62.811482622609,-1.41999996598415));
#53038=CARTESIAN_POINT('Origin',(-85.9899999999999,64.1105207282856,-57.8300000340159));
#53039=CARTESIAN_POINT('',(-85.5900000000001,62.8114826226089,-58.5800000340159));
#53040=CARTESIAN_POINT('',(-85.5900000000001,63.2487659305946,-56.6022465291719));
#53041=CARTESIAN_POINT('Origin',(-85.59,64.1105207282856,-57.8300000340159));
#53042=CARTESIAN_POINT('',(-86.39,62.8114826226089,-58.5800000340159));
#53043=CARTESIAN_POINT('',(-85.5899999999994,62.8114826226089,-58.5800000340159));
#53044=CARTESIAN_POINT('',(-86.39,63.248765930775,-56.602246529842));
#53045=CARTESIAN_POINT('Origin',(-86.39,64.1105207282856,-57.8300000340159));
#53046=CARTESIAN_POINT('',(-85.5900000000001,63.2487659305946,-56.602246529172));
#53047=CARTESIAN_POINT('Origin',(-85.9900000001603,27.9852423132283,4.74081761843475));
#53048=CARTESIAN_POINT('',(-85.59,26.6862042075517,3.99081761843476));
#53049=CARTESIAN_POINT('',(-85.5899999999998,27.3389968866617,6.09446707403308));
#53050=CARTESIAN_POINT('Origin',(-85.59,27.9852423132283,4.74081761843475));
#53051=CARTESIAN_POINT('',(-86.39,26.6862042075517,3.99081761843476));
#53052=CARTESIAN_POINT('',(913.61,26.6862042075521,3.99081761843475));
#53053=CARTESIAN_POINT('',(-86.3899999999999,27.3389968866617,6.09446707403308));
#53054=CARTESIAN_POINT('Origin',(-86.39,27.9852423132283,4.74081761843475));
#53055=CARTESIAN_POINT('',(-85.5899999999998,27.3389968866617,6.09446707403308));
#53056=CARTESIAN_POINT('Origin',(-85.9900000000819,6.19540997866983,-27.));
#53057=CARTESIAN_POINT('',(-85.5900000000001,6.19540997866983,-28.5));
#53058=CARTESIAN_POINT('',(-85.59,4.69995568091292,-26.8833104832455));
#53059=CARTESIAN_POINT('Origin',(-85.59,6.19540997866983,-27.));
#53060=CARTESIAN_POINT('',(-86.39,6.19540997866983,-28.5));
#53061=CARTESIAN_POINT('',(913.61,6.19540997867027,-28.5));
#53062=CARTESIAN_POINT('',(-86.39,4.69995568091292,-26.8833104832455));
#53063=CARTESIAN_POINT('Origin',(-86.39,6.19540997866983,-27.));
#53064=CARTESIAN_POINT('',(-85.59,4.69995568091292,-26.8833104832455));
#53065=CARTESIAN_POINT('Origin',(-85.99,6.19541004646761,-33.));
#53066=CARTESIAN_POINT('',(-85.5899999999999,4.69995574181559,-33.1166894283889));
#53067=CARTESIAN_POINT('',(-85.5900000000001,6.19541004646761,-31.5));
#53068=CARTESIAN_POINT('Origin',(-85.59,6.19541004646761,-33.));
#53069=CARTESIAN_POINT('',(-86.3899999999999,4.69995574181559,-33.1166894283889));
#53070=CARTESIAN_POINT('',(-86.3899999999999,4.69995574181558,-33.1166894283889));
#53071=CARTESIAN_POINT('',(-86.39,6.19541004646761,-31.5));
#53072=CARTESIAN_POINT('Origin',(-86.39,6.19541004646761,-33.));
#53073=CARTESIAN_POINT('',(913.61,6.19541004646805,-31.5));
#53074=CARTESIAN_POINT('Origin',(-85.9900000000002,27.9852422140127,-64.7408177902812));
#53075=CARTESIAN_POINT('',(-85.5899999999997,27.338996733446,-66.0944672200995));
#53076=CARTESIAN_POINT('',(-85.59,26.686204108336,-63.9908177902812));
#53077=CARTESIAN_POINT('Origin',(-85.59,27.9852422140127,-64.7408177902812));
#53078=CARTESIAN_POINT('',(-86.3899999999998,27.338996733446,-66.0944672200995));
#53079=CARTESIAN_POINT('',(-86.3899999999999,27.338996733446,-66.0944672200995));
#53080=CARTESIAN_POINT('',(-86.39,26.686204108336,-63.9908177902812));
#53081=CARTESIAN_POINT('Origin',(-86.39,27.9852422140127,-64.7408177902812));
#53082=CARTESIAN_POINT('',(913.61,26.6862041083364,-63.9908177902812));
#53083=CARTESIAN_POINT('Ctrl Pts',(-85.5900000000001,42.9713195513441,-22.1631559443849));
#53084=CARTESIAN_POINT('Ctrl Pts',(-86.55,42.9713195513441,-22.1631559443849));
#53085=CARTESIAN_POINT('Ctrl Pts',(-85.5900000000001,42.9868830995498,-22.1599633677126));
#53086=CARTESIAN_POINT('Ctrl Pts',(-86.55,42.9868830995498,-22.1599633677126));
#53087=CARTESIAN_POINT('Ctrl Pts',(-85.5900000000001,43.5156846168693,-22.0531343444844));
#53088=CARTESIAN_POINT('Ctrl Pts',(-86.55,43.5156846168693,-22.0531343444844));
#53089=CARTESIAN_POINT('Ctrl Pts',(-85.5900000000002,44.0551666698534,-22.));
#53090=CARTESIAN_POINT('Ctrl Pts',(-86.5500000000001,44.0551666698534,-22.));
#53091=CARTESIAN_POINT('Ctrl Pts',(-85.5900000000002,44.5787611019615,-22.));
#53092=CARTESIAN_POINT('Ctrl Pts',(-86.5500000000001,44.5787611019615,-22.));
#53093=CARTESIAN_POINT('',(-85.5900000000004,44.5787611019615,-22.));
#53094=CARTESIAN_POINT('',(-85.5900000000003,42.9713195513605,-22.1631559443815));
#53095=CARTESIAN_POINT('Ctrl Pts',(-85.5900000000003,44.5787611019615,-22.));
#53096=CARTESIAN_POINT('Ctrl Pts',(-85.5900000000003,44.0551666698534,-22.));
#53097=CARTESIAN_POINT('Ctrl Pts',(-85.5900000000001,43.5315722377453,-22.0515695504083));
#53098=CARTESIAN_POINT('Ctrl Pts',(-85.5900000000001,43.0180385258325,-22.1537177567742));
#53099=CARTESIAN_POINT('Ctrl Pts',(-85.5900000000001,43.0024561811422,-22.1568172778458));
#53100=CARTESIAN_POINT('Ctrl Pts',(-85.5900000000001,42.9868830995607,-22.1599633677104));
#53101=CARTESIAN_POINT('Ctrl Pts',(-85.5900000000001,42.9713195513605,-22.1631559443815));
#53102=CARTESIAN_POINT('',(-86.39,44.5787611019615,-22.));
#53103=CARTESIAN_POINT('',(913.61,44.578761101962,-22.));
#53104=CARTESIAN_POINT('',(-86.39,42.9713195515195,-22.1631559452401));
#53105=CARTESIAN_POINT('Ctrl Pts',(-86.3899999999999,42.9713195513441,-22.1631559443849));
#53106=CARTESIAN_POINT('Ctrl Pts',(-86.3899999999999,42.9868830995498,-22.1599633677126));
#53107=CARTESIAN_POINT('Ctrl Pts',(-86.3899999999999,43.0024561811367,-22.1568172778469));
#53108=CARTESIAN_POINT('Ctrl Pts',(-86.3899999999999,43.0180385258325,-22.1537177567742));
#53109=CARTESIAN_POINT('Ctrl Pts',(-86.3899999999999,43.5315722377453,-22.0515695504083));
#53110=CARTESIAN_POINT('Ctrl Pts',(-86.39,44.0551666698534,-22.));
#53111=CARTESIAN_POINT('Ctrl Pts',(-86.39,44.5787611019615,-22.));
#53112=CARTESIAN_POINT('',(-86.3899999999997,42.9713195513605,-22.1631559443815));
#53113=CARTESIAN_POINT('Ctrl Pts',(-85.59,36.8454205805627,-11.0146003459994));
#53114=CARTESIAN_POINT('Ctrl Pts',(-86.55,36.8454205805627,-11.0146003459994));
#53115=CARTESIAN_POINT('Ctrl Pts',(-85.59,38.0507425034688,-10.5236598584192));
#53116=CARTESIAN_POINT('Ctrl Pts',(-86.55,38.0507425034688,-10.5236598584192));
#53117=CARTESIAN_POINT('Ctrl Pts',(-85.59,40.5938700965656,-9.76033053442545));
#53118=CARTESIAN_POINT('Ctrl Pts',(-86.5499999999999,40.5938700965656,-9.76033053442545));
#53119=CARTESIAN_POINT('Ctrl Pts',(-85.5900000000001,43.2370503696844,-9.5));
#53120=CARTESIAN_POINT('Ctrl Pts',(-86.5500000000001,43.2370503696844,-9.5));
#53121=CARTESIAN_POINT('Ctrl Pts',(-85.5900000000001,44.5787611019615,-9.5));
#53122=CARTESIAN_POINT('Ctrl Pts',(-86.5500000000001,44.5787611019615,-9.5));
#53123=CARTESIAN_POINT('',(-85.5900000000001,44.5787611019615,-9.5));
#53124=CARTESIAN_POINT('',(-85.59,36.8454205811755,-11.0146003457498));
#53125=CARTESIAN_POINT('Ctrl Pts',(-85.5900000000001,44.5787611019615,-9.5));
#53126=CARTESIAN_POINT('Ctrl Pts',(-85.5900000000001,43.2370503696844,-9.5));
#53127=CARTESIAN_POINT('Ctrl Pts',(-85.59,40.5938700967862,-9.76033053440373));
#53128=CARTESIAN_POINT('Ctrl Pts',(-85.59,38.0507425038933,-10.5236598582919));
#53129=CARTESIAN_POINT('Ctrl Pts',(-85.59,36.8454205811755,-11.0146003457498));
#53130=CARTESIAN_POINT('',(-86.39,44.5787611019615,-9.5));
#53131=CARTESIAN_POINT('',(913.61,44.578761101962,-9.5));
#53132=CARTESIAN_POINT('',(-86.39,36.8454205803542,-11.0146003454874));
#53133=CARTESIAN_POINT('Ctrl Pts',(-86.3899999999999,36.8454205805627,-11.0146003459994));
#53134=CARTESIAN_POINT('Ctrl Pts',(-86.3899999999999,38.0507425034688,-10.5236598584192));
#53135=CARTESIAN_POINT('Ctrl Pts',(-86.3899999999999,40.5938700965656,-9.76033053442545));
#53136=CARTESIAN_POINT('Ctrl Pts',(-86.39,43.2370503696844,-9.5));
#53137=CARTESIAN_POINT('Ctrl Pts',(-86.39,44.5787611019615,-9.5));
#53138=CARTESIAN_POINT('',(-86.39,36.8454205811755,-11.0146003457498));
#53139=CARTESIAN_POINT('Ctrl Pts',(-85.59,50.3318213149459,-13.4727301355976));
#53140=CARTESIAN_POINT('Ctrl Pts',(-86.5500000000005,50.3318213149459,-13.4727301355976));
#53141=CARTESIAN_POINT('Ctrl Pts',(-85.59,49.5680966220862,-13.206928056047));
#53142=CARTESIAN_POINT('Ctrl Pts',(-86.5500000000006,49.5680966220862,-13.206928056047));
#53143=CARTESIAN_POINT('Ctrl Pts',(-85.5900000000001,47.6781372544074,-12.6924535152679));
#53144=CARTESIAN_POINT('Ctrl Pts',(-86.5500000000007,47.6781372544074,-12.6924535152679));
#53145=CARTESIAN_POINT('Ctrl Pts',(-85.5899999999996,45.7241239221981,-12.5));
#53146=CARTESIAN_POINT('Ctrl Pts',(-86.5500000000002,45.7241239221981,-12.5));
#53147=CARTESIAN_POINT('Ctrl Pts',(-85.5899999999996,44.5787611019615,-12.5));
#53148=CARTESIAN_POINT('Ctrl Pts',(-86.5500000000002,44.5787611019615,-12.5));
#53149=CARTESIAN_POINT('',(-85.5900000000002,50.3318212771098,-13.4727301224294));
#53150=CARTESIAN_POINT('',(-85.5899999999998,44.5787611019615,-12.5));
#53151=CARTESIAN_POINT('Ctrl Pts',(-85.5900000000002,50.3318212771098,-13.4727301224294));
#53152=CARTESIAN_POINT('Ctrl Pts',(-85.5900000000002,49.5680965962538,-13.2069280490151));
#53153=CARTESIAN_POINT('Ctrl Pts',(-85.5900000000003,47.6781372410534,-12.6924535139526));
#53154=CARTESIAN_POINT('Ctrl Pts',(-85.5899999999999,45.7241239221981,-12.5));
#53155=CARTESIAN_POINT('Ctrl Pts',(-85.5899999999998,44.5787611019615,-12.5));
#53156=CARTESIAN_POINT('',(-86.39,44.5787611019615,-12.5));
#53157=CARTESIAN_POINT('',(913.61,44.578761101962,-12.5));
#53158=CARTESIAN_POINT('',(-86.3900000000001,50.3318212785861,-13.4727301229432));
#53159=CARTESIAN_POINT('Ctrl Pts',(-86.3900000000002,50.3318212785861,-13.4727301229432));
#53160=CARTESIAN_POINT('Ctrl Pts',(-86.3900000000003,49.5680965972618,-13.2069280492894));
#53161=CARTESIAN_POINT('Ctrl Pts',(-86.3900000000004,47.6781372415745,-12.692453514004));
#53162=CARTESIAN_POINT('Ctrl Pts',(-86.3899999999999,45.7241239221981,-12.5));
#53163=CARTESIAN_POINT('Ctrl Pts',(-86.3899999999998,44.5787611019615,-12.5));
#53164=CARTESIAN_POINT('',(-86.3900000000003,50.3318212771098,-13.4727301224294));
#53165=CARTESIAN_POINT('Ctrl Pts',(-85.5899999999998,30.8757056257453,-0.530143046109299));
#53166=CARTESIAN_POINT('Ctrl Pts',(-86.55,30.8757056257453,-0.530143046109299));
#53167=CARTESIAN_POINT('Ctrl Pts',(-85.5899999999998,31.2936434644341,-0.335776881547456));
#53168=CARTESIAN_POINT('Ctrl Pts',(-86.55,31.2936434644341,-0.335776881547456));
#53169=CARTESIAN_POINT('Ctrl Pts',(-85.5899999999998,33.6635280544018,0.70564601555246));
#53170=CARTESIAN_POINT('Ctrl Pts',(-86.55,33.6635280544018,0.70564601555246));
#53171=CARTESIAN_POINT('Ctrl Pts',(-85.5899999999998,38.1974539606436,2.08099740293234));
#53172=CARTESIAN_POINT('Ctrl Pts',(-86.55,38.1974539606436,2.08099740293234));
#53173=CARTESIAN_POINT('Ctrl Pts',(-85.5899999999998,42.4516587215222,2.5));
#53174=CARTESIAN_POINT('Ctrl Pts',(-86.55,42.4516587215222,2.5));
#53175=CARTESIAN_POINT('Ctrl Pts',(-85.5899999999998,44.5787611019615,2.5));
#53176=CARTESIAN_POINT('Ctrl Pts',(-86.55,44.5787611019615,2.5));
#53177=CARTESIAN_POINT('',(-85.59,44.5787611019615,2.5));
#53178=CARTESIAN_POINT('',(-85.5900000000001,30.8757056257996,-0.53014304608406));
#53179=CARTESIAN_POINT('Ctrl Pts',(-85.59,44.5787611019615,2.5));
#53180=CARTESIAN_POINT('Ctrl Pts',(-85.5900000000001,42.4516587215222,2.5));
#53181=CARTESIAN_POINT('Ctrl Pts',(-85.5900000000001,38.1974539606436,2.08099740293234));
#53182=CARTESIAN_POINT('Ctrl Pts',(-85.5900000000001,33.6635280544172,0.705646015557152));
#53183=CARTESIAN_POINT('Ctrl Pts',(-85.5900000000001,31.2936434644636,-0.335776881534512));
#53184=CARTESIAN_POINT('Ctrl Pts',(-85.5900000000001,30.8757056257996,-0.53014304608406));
#53185=CARTESIAN_POINT('',(-86.39,44.5787611019615,2.5));
#53186=CARTESIAN_POINT('',(913.61,44.578761101962,2.5));
#53187=CARTESIAN_POINT('',(-86.39,30.8757056270897,-0.530143045484072));
#53188=CARTESIAN_POINT('Ctrl Pts',(-86.39,30.8757056270897,-0.530143045484066));
#53189=CARTESIAN_POINT('Ctrl Pts',(-86.39,31.2936434644341,-0.335776881547456));
#53190=CARTESIAN_POINT('Ctrl Pts',(-86.39,33.6635280544018,0.70564601555246));
#53191=CARTESIAN_POINT('Ctrl Pts',(-86.39,38.1974539606436,2.08099740293234));
#53192=CARTESIAN_POINT('Ctrl Pts',(-86.39,42.4516587215222,2.5));
#53193=CARTESIAN_POINT('Ctrl Pts',(-86.39,44.5787611019615,2.5));
#53194=CARTESIAN_POINT('',(-86.39,30.8757056258048,-0.530143046081613));
#53195=CARTESIAN_POINT('Ctrl Pts',(-85.5899999999995,56.5066592280182,-3.0190060294803));
#53196=CARTESIAN_POINT('Ctrl Pts',(-86.5500000000001,56.5066592280182,-3.0190060294803));
#53197=CARTESIAN_POINT('Ctrl Pts',(-85.5899999999995,56.2948319481592,-2.92534739713906));
#53198=CARTESIAN_POINT('Ctrl Pts',(-86.5500000000001,56.2948319481592,-2.92534739713906));
#53199=CARTESIAN_POINT('Ctrl Pts',(-85.5899999999995,54.3068457690469,-2.07424376132673));
#53200=CARTESIAN_POINT('Ctrl Pts',(-86.5500000000001,54.3068457690469,-2.07424376132673));
#53201=CARTESIAN_POINT('Ctrl Pts',(-85.5899999999994,50.3710245071578,-0.880325434261424));
#53202=CARTESIAN_POINT('Ctrl Pts',(-86.5499999999999,50.3710245071578,-0.880325434261424));
#53203=CARTESIAN_POINT('Ctrl Pts',(-85.5899999999998,46.5095155703603,-0.500000000000001));
#53204=CARTESIAN_POINT('Ctrl Pts',(-86.5500000000004,46.5095155703603,-0.500000000000001));
#53205=CARTESIAN_POINT('Ctrl Pts',(-85.5899999999998,44.5787611019615,-0.5));
#53206=CARTESIAN_POINT('Ctrl Pts',(-86.5500000000004,44.5787611019615,-0.5));
#53207=CARTESIAN_POINT('',(-85.59,56.5066592279994,-3.01900602947196));
#53208=CARTESIAN_POINT('',(-85.5900000000003,44.5787611019615,-0.5));
#53209=CARTESIAN_POINT('Ctrl Pts',(-85.59,56.5066592279994,-3.01900602947196));
#53210=CARTESIAN_POINT('Ctrl Pts',(-85.59,56.2948319481467,-2.92534739713372));
#53211=CARTESIAN_POINT('Ctrl Pts',(-85.59,54.3068457690404,-2.07424376132475));
#53212=CARTESIAN_POINT('Ctrl Pts',(-85.5899999999998,50.3710245071578,-0.880325434261424));
#53213=CARTESIAN_POINT('Ctrl Pts',(-85.5900000000003,46.5095155703603,-0.500000000000001));
#53214=CARTESIAN_POINT('Ctrl Pts',(-85.5900000000003,44.5787611019615,-0.5));
#53215=CARTESIAN_POINT('',(-86.39,44.5787611019615,-0.5));
#53216=CARTESIAN_POINT('',(913.61,44.578761101962,-0.5));
#53217=CARTESIAN_POINT('',(-86.39,56.5066592282128,-3.01900602900217));
#53218=CARTESIAN_POINT('Ctrl Pts',(-86.3899999999997,56.5066592280182,-3.0190060294803));
#53219=CARTESIAN_POINT('Ctrl Pts',(-86.3899999999997,56.2948319481592,-2.92534739713906));
#53220=CARTESIAN_POINT('Ctrl Pts',(-86.3899999999997,54.3068457690469,-2.07424376132673));
#53221=CARTESIAN_POINT('Ctrl Pts',(-86.3899999999995,50.3710245071578,-0.880325434261424));
#53222=CARTESIAN_POINT('Ctrl Pts',(-86.39,46.5095155703603,-0.500000000000001));
#53223=CARTESIAN_POINT('Ctrl Pts',(-86.39,44.5787611019615,-0.5));
#53224=CARTESIAN_POINT('',(-86.3899999999997,56.5066592279993,-3.01900602947191));
#53225=CARTESIAN_POINT('Origin',(-74.39,80.0825925853381,-65.5038314833765));
#53226=CARTESIAN_POINT('',(-83.59,81.8325925853381,-65.5038314833765));
#53227=CARTESIAN_POINT('Origin',(-83.59,80.0825925853381,-65.5038314833765));
#53228=CARTESIAN_POINT('',(-84.39,81.8325925853381,-65.5038314833765));
#53229=CARTESIAN_POINT('',(-74.39,81.8325925853381,-65.5038314833765));
#53230=CARTESIAN_POINT('Origin',(-84.39,80.0825925853381,-65.5038314833765));
#53231=CARTESIAN_POINT('Origin',(-74.39,9.0749296185849,-65.5038314833765));
#53232=CARTESIAN_POINT('',(-83.59,10.8249296185849,-65.5038314833765));
#53233=CARTESIAN_POINT('Origin',(-83.59,9.07492961858489,-65.5038314833765));
#53234=CARTESIAN_POINT('',(-84.39,10.8249296185849,-65.5038314833765));
#53235=CARTESIAN_POINT('',(-74.39,10.8249296185849,-65.5038314833765));
#53236=CARTESIAN_POINT('Origin',(-84.39,9.07492961858489,-65.5038314833765));
#53237=CARTESIAN_POINT('Origin',(-74.39,9.0749296185849,5.50383148337648));
#53238=CARTESIAN_POINT('',(-83.59,10.8249296185849,5.50383148337648));
#53239=CARTESIAN_POINT('Origin',(-83.59,9.07492961858489,5.50383148337648));
#53240=CARTESIAN_POINT('',(-84.39,10.8249296185849,5.50383148337648));
#53241=CARTESIAN_POINT('',(-74.39,10.8249296185849,5.50383148337648));
#53242=CARTESIAN_POINT('Origin',(-84.39,9.07492961858489,5.50383148337648));
#53243=CARTESIAN_POINT('Origin',(-74.39,80.0825925853381,5.50383148337648));
#53244=CARTESIAN_POINT('',(-83.59,81.8325925853382,5.50383148337648));
#53245=CARTESIAN_POINT('Origin',(-83.59,80.0825925853381,5.50383148337648));
#53246=CARTESIAN_POINT('',(-84.39,81.8325925853382,5.50383148337648));
#53247=CARTESIAN_POINT('',(-74.39,81.8325925853382,5.50383148337648));
#53248=CARTESIAN_POINT('Origin',(-84.39,80.0825925853381,5.50383148337648));
#53249=CARTESIAN_POINT('Origin',(-85.09,44.5787611019615,-30.));
#53250=CARTESIAN_POINT('',(-85.1899999999999,44.5787611019615,-72.4898979485563));
#53251=CARTESIAN_POINT('Origin',(-85.1899999999999,44.5787611019615,-30.));
#53252=CARTESIAN_POINT('',(-85.59,44.5787611019615,-72.));
#53253=CARTESIAN_POINT('Origin',(-85.09,44.5787611019615,-72.));
#53254=CARTESIAN_POINT('Origin',(-85.59,44.5787611019615,-30.));
#53255=CARTESIAN_POINT('Origin',(-85.59,44.5787611019615,-30.));
#53256=CARTESIAN_POINT('',(-85.35,44.5787611019615,-73.2737346662473));
#53257=CARTESIAN_POINT('Origin',(-85.35,44.5787611019615,-30.));
#53258=CARTESIAN_POINT('',(-84.39,44.5787611019615,-74.4494897427832));
#53259=CARTESIAN_POINT('Origin',(-85.59,44.5787611019615,-74.4494897427832));
#53260=CARTESIAN_POINT('Origin',(-84.39,44.5787611019615,-30.));
#53261=CARTESIAN_POINT('Origin',(-85.09,44.5787611019615,-30.));
#53262=CARTESIAN_POINT('',(-86.39,44.5787611019615,-72.));
#53263=CARTESIAN_POINT('Origin',(-86.39,44.5787611019615,-30.));
#53264=CARTESIAN_POINT('Origin',(-85.09,44.5787611019615,-72.));
#53265=CARTESIAN_POINT('Origin',(-85.59,44.5787611019615,-30.));
#53266=CARTESIAN_POINT('',(-83.59,44.5787611019615,-74.4494897427832));
#53267=CARTESIAN_POINT('Origin',(-83.59,44.5787611019615,-30.));
#53268=CARTESIAN_POINT('Origin',(-85.59,44.5787611019615,-74.4494897427832));
#53269=CARTESIAN_POINT('Origin',(-48.39,-0.8,-66.39));
#53270=CARTESIAN_POINT('',(-48.39,-0.8,-67.64));
#53271=CARTESIAN_POINT('Origin',(-48.39,-0.8,-66.39));
#53272=CARTESIAN_POINT('',(-48.39,1.38777878078145E-16,-67.64));
#53273=CARTESIAN_POINT('',(-48.39,-0.8,-67.64));
#53274=CARTESIAN_POINT('Origin',(-48.39,1.0842021724855E-16,-66.39));
#53275=CARTESIAN_POINT('Origin',(-48.39,-0.8,67.61));
#53276=CARTESIAN_POINT('',(-48.39,-0.8,66.36));
#53277=CARTESIAN_POINT('Origin',(-48.39,-0.8,67.61));
#53278=CARTESIAN_POINT('',(-48.39,1.38777878078145E-16,66.36));
#53279=CARTESIAN_POINT('',(-48.39,-0.8,66.36));
#53280=CARTESIAN_POINT('Origin',(-48.39,1.0842021724855E-16,67.61));
#53281=CARTESIAN_POINT('Origin',(61.61,-0.8,67.61));
#53282=CARTESIAN_POINT('',(61.61,-0.8,66.36));
#53283=CARTESIAN_POINT('Origin',(61.61,-0.8,67.61));
#53284=CARTESIAN_POINT('',(61.61,1.38777878078145E-16,66.36));
#53285=CARTESIAN_POINT('',(61.61,-0.8,66.36));
#53286=CARTESIAN_POINT('Origin',(61.61,1.0842021724855E-16,67.61));
#53287=CARTESIAN_POINT('Origin',(61.61,-0.8,-66.39));
#53288=CARTESIAN_POINT('',(61.61,-0.8,-67.64));
#53289=CARTESIAN_POINT('Origin',(61.61,-0.8,-66.39));
#53290=CARTESIAN_POINT('',(61.61,1.38777878078145E-16,-67.64));
#53291=CARTESIAN_POINT('',(61.61,-0.8,-67.64));
#53292=CARTESIAN_POINT('Origin',(61.61,1.0842021724855E-16,-66.39));
#53293=CARTESIAN_POINT('Ctrl Pts',(-85.5899999999997,44.5787611019615,10.));
#53294=CARTESIAN_POINT('Ctrl Pts',(-86.5500000000002,44.5787611019615,10.));
#53295=CARTESIAN_POINT('Ctrl Pts',(-85.5899999999997,45.8877414717319,9.99999275845459));
#53296=CARTESIAN_POINT('Ctrl Pts',(-86.5500000000002,45.8877414717319,9.99999275845459));
#53297=CARTESIAN_POINT('Ctrl Pts',(-85.5899999999995,48.505792262655,9.872293593712));
#53298=CARTESIAN_POINT('Ctrl Pts',(-86.55,48.505792262655,9.872293593712));
#53299=CARTESIAN_POINT('Ctrl Pts',(-85.5899999999998,52.3946948078235,9.29405950036845));
#53300=CARTESIAN_POINT('Ctrl Pts',(-86.5500000000003,52.3946948078235,9.29405950036845));
#53301=CARTESIAN_POINT('Ctrl Pts',(-85.5899999999998,56.2089960261238,8.34006566164691));
#53302=CARTESIAN_POINT('Ctrl Pts',(-86.5500000000003,56.2089960261238,8.34006566164691));
#53303=CARTESIAN_POINT('Ctrl Pts',(-85.5899999999998,59.3413461461202,7.21805787048124));
#53304=CARTESIAN_POINT('Ctrl Pts',(-86.5500000000003,59.3413461461202,7.21805787048124));
#53305=CARTESIAN_POINT('Ctrl Pts',(-85.5899999999999,61.1821105626304,6.39829807210438));
#53306=CARTESIAN_POINT('Ctrl Pts',(-86.5500000000004,61.1821105626304,6.39829807210438));
#53307=CARTESIAN_POINT('Ctrl Pts',(-85.5899999999999,61.8185255808726,6.09446728275319));
#53308=CARTESIAN_POINT('Ctrl Pts',(-86.5500000000004,61.8185255808726,6.09446728275319));
#53309=CARTESIAN_POINT('',(-85.59,61.8185255808636,6.09446728275746));
#53310=CARTESIAN_POINT('',(-85.5899999999999,44.5787611019615,10.));
#53311=CARTESIAN_POINT('Ctrl Pts',(-85.5899999999999,61.8185255808636,6.09446728275746));
#53312=CARTESIAN_POINT('Ctrl Pts',(-85.5899999999999,61.1821105626304,6.39829807210438));
#53313=CARTESIAN_POINT('Ctrl Pts',(-85.5899999999998,59.3413461461202,7.21805787048124));
#53314=CARTESIAN_POINT('Ctrl Pts',(-85.5899999999998,56.2089960261238,8.34006566164691));
#53315=CARTESIAN_POINT('Ctrl Pts',(-85.5899999999998,52.3946948078235,9.29405950036845));
#53316=CARTESIAN_POINT('Ctrl Pts',(-85.5899999999995,48.505792262655,9.872293593712));
#53317=CARTESIAN_POINT('Ctrl Pts',(-85.5899999999997,45.8877414717319,9.99999275845459));
#53318=CARTESIAN_POINT('Ctrl Pts',(-85.5899999999997,44.5787611019615,10.));
#53319=CARTESIAN_POINT('',(-86.3899999999999,44.5787611019615,10.));
#53320=CARTESIAN_POINT('',(903.61,44.578761101962,10.));
#53321=CARTESIAN_POINT('',(-86.39,61.8185255808636,6.09446728275746));
#53322=CARTESIAN_POINT('Ctrl Pts',(-86.39,61.8185255808636,6.09446728275747));
#53323=CARTESIAN_POINT('Ctrl Pts',(-86.39,61.1821105626304,6.39829807210438));
#53324=CARTESIAN_POINT('Ctrl Pts',(-86.39,59.3413461461202,7.21805787048124));
#53325=CARTESIAN_POINT('Ctrl Pts',(-86.39,56.2089960261238,8.34006566164691));
#53326=CARTESIAN_POINT('Ctrl Pts',(-86.39,52.3946948078235,9.29405950036845));
#53327=CARTESIAN_POINT('Ctrl Pts',(-86.3899999999996,48.505792262655,9.872293593712));
#53328=CARTESIAN_POINT('Ctrl Pts',(-86.3899999999998,45.8877414717319,9.99999275845459));
#53329=CARTESIAN_POINT('Ctrl Pts',(-86.3899999999998,44.5787611019615,10.));
#53330=CARTESIAN_POINT('',(-86.39,61.8185255808636,6.09446728275746));
#53331=CARTESIAN_POINT('Origin',(-84.39,-3.2,80.));
#53332=CARTESIAN_POINT('',(-67.3504246383764,-3.20000000000001,-80.));
#53333=CARTESIAN_POINT('',(-67.3504246383764,-3.20000000000001,-78.16));
#53334=CARTESIAN_POINT('',(-67.3504246383764,-3.20000000000001,-80.));
#53335=CARTESIAN_POINT('',(-82.2324777960769,-3.2,-80.));
#53336=CARTESIAN_POINT('',(-84.39,-3.2,-80.));
#53337=CARTESIAN_POINT('',(-82.2324777960769,-3.2,-70.));
#53338=CARTESIAN_POINT('',(-82.2324777960769,-3.2,-70.));
#53339=CARTESIAN_POINT('',(-82.79,-3.2,-68.8330657242578));
#53340=CARTESIAN_POINT('Origin',(-83.7324777960769,-3.2,-70.));
#53341=CARTESIAN_POINT('',(-82.79,-3.2,68.8330657242578));
#53342=CARTESIAN_POINT('',(-82.79,-3.2,80.));
#53343=CARTESIAN_POINT('',(-82.2324777960769,-3.2,70.));
#53344=CARTESIAN_POINT('Origin',(-83.7324777960769,-3.2,70.));
#53345=CARTESIAN_POINT('',(-82.2324777960769,-3.2,80.));
#53346=CARTESIAN_POINT('',(-82.2324777960769,-3.2,70.));
#53347=CARTESIAN_POINT('',(-67.3504246383764,-3.2,80.));
#53348=CARTESIAN_POINT('',(-84.39,-3.2,80.));
#53349=CARTESIAN_POINT('',(-67.3504246383764,-3.19999999999999,78.16));
#53350=CARTESIAN_POINT('',(-67.3504246383764,-3.19999999999999,78.16));
#53351=CARTESIAN_POINT('',(-67.1104246383764,-3.19999999999999,78.16));
#53352=CARTESIAN_POINT('',(-67.1104246383764,-3.19999999999999,78.16));
#53353=CARTESIAN_POINT('',(-67.1104246383764,-3.19999999999999,78.4));
#53354=CARTESIAN_POINT('',(-67.1104246383764,-3.19999999999999,78.4));
#53355=CARTESIAN_POINT('',(52.8895753616236,-3.19999999999999,78.4));
#53356=CARTESIAN_POINT('',(52.8895753616236,-3.19999999999999,78.4));
#53357=CARTESIAN_POINT('',(52.8895753616236,-3.19999999999999,78.16));
#53358=CARTESIAN_POINT('',(52.8895753616236,-3.19999999999999,78.16));
#53359=CARTESIAN_POINT('',(53.1295753616236,-3.19999999999999,78.16));
#53360=CARTESIAN_POINT('',(53.1295753616236,-3.19999999999999,78.16));
#53361=CARTESIAN_POINT('',(53.1295753616236,-3.2,80.));
#53362=CARTESIAN_POINT('',(53.1295753616236,-3.2,80.));
#53363=CARTESIAN_POINT('',(68.4524777960769,-3.2,80.));
#53364=CARTESIAN_POINT('',(-84.39,-3.2,80.));
#53365=CARTESIAN_POINT('',(68.4524777960769,-3.2,70.));
#53366=CARTESIAN_POINT('',(68.4524777960769,-3.2,70.));
#53367=CARTESIAN_POINT('',(69.01,-3.2,68.8330657242578));
#53368=CARTESIAN_POINT('Origin',(69.9524777960769,-3.2,70.));
#53369=CARTESIAN_POINT('',(69.01,-3.2,-68.8330657242578));
#53370=CARTESIAN_POINT('',(69.01,-3.2,80.));
#53371=CARTESIAN_POINT('',(68.4524777960769,-3.2,-70.));
#53372=CARTESIAN_POINT('Origin',(69.9524777960769,-3.2,-70.));
#53373=CARTESIAN_POINT('',(68.4524777960769,-3.2,-80.));
#53374=CARTESIAN_POINT('',(68.4524777960769,-3.2,-70.));
#53375=CARTESIAN_POINT('',(53.1295753616236,-3.2,-80.));
#53376=CARTESIAN_POINT('',(-84.39,-3.2,-80.));
#53377=CARTESIAN_POINT('',(53.1295753616236,-3.20000000000001,-78.16));
#53378=CARTESIAN_POINT('',(53.1295753616236,-3.20000000000001,-78.16));
#53379=CARTESIAN_POINT('',(52.8895753616236,-3.20000000000001,-78.16));
#53380=CARTESIAN_POINT('',(52.8895753616236,-3.20000000000001,-78.16));
#53381=CARTESIAN_POINT('',(52.8895753616236,-3.20000000000001,-78.4));
#53382=CARTESIAN_POINT('',(52.8895753616236,-3.20000000000001,-78.4));
#53383=CARTESIAN_POINT('',(-67.1104246383764,-3.20000000000001,-78.4));
#53384=CARTESIAN_POINT('',(-67.1104246383764,-3.20000000000001,-78.4));
#53385=CARTESIAN_POINT('',(-67.1104246383764,-3.20000000000001,-78.16));
#53386=CARTESIAN_POINT('',(-67.1104246383764,-3.20000000000001,-78.16));
#53387=CARTESIAN_POINT('',(-67.3504246383764,-3.20000000000001,-78.16));
#53388=CARTESIAN_POINT('',(-44.7186753691159,-3.2,69.61));
#53389=CARTESIAN_POINT('',(-43.1186753691159,-3.2,69.61));
#53390=CARTESIAN_POINT('',(-84.39,-3.2,69.61));
#53391=CARTESIAN_POINT('',(-52.061324630884,-3.2,69.61));
#53392=CARTESIAN_POINT('',(-84.39,-3.2,69.61));
#53393=CARTESIAN_POINT('',(-53.661324630884,-3.2,69.61));
#53394=CARTESIAN_POINT('',(-84.39,-3.2,69.61));
#53395=CARTESIAN_POINT('',(-53.661324630884,-3.2,65.61));
#53396=CARTESIAN_POINT('',(-53.661324630884,-3.2,65.61));
#53397=CARTESIAN_POINT('',(-52.061324630884,-3.2,65.61));
#53398=CARTESIAN_POINT('',(-84.39,-3.2,65.61));
#53399=CARTESIAN_POINT('',(-44.7186753691159,-3.2,65.61));
#53400=CARTESIAN_POINT('',(-84.39,-3.2,65.61));
#53401=CARTESIAN_POINT('',(-43.1186753691159,-3.2,65.61));
#53402=CARTESIAN_POINT('',(-84.39,-3.2,65.61));
#53403=CARTESIAN_POINT('',(-43.1186753691159,-3.2,67.61));
#53404=CARTESIAN_POINT('',(65.2813246308841,-3.2,-64.39));
#53405=CARTESIAN_POINT('',(66.8813246308841,-3.2,-64.39));
#53406=CARTESIAN_POINT('',(-84.39,-3.2,-64.39));
#53407=CARTESIAN_POINT('',(57.938675369116,-3.2,-64.39));
#53408=CARTESIAN_POINT('',(-84.39,-3.2,-64.39));
#53409=CARTESIAN_POINT('',(56.338675369116,-3.2,-64.39));
#53410=CARTESIAN_POINT('',(-84.39,-3.2,-64.39));
#53411=CARTESIAN_POINT('',(56.338675369116,-3.2,-68.39));
#53412=CARTESIAN_POINT('',(56.338675369116,-3.2,-68.39));
#53413=CARTESIAN_POINT('',(57.938675369116,-3.2,-68.39));
#53414=CARTESIAN_POINT('',(-84.39,-3.2,-68.39));
#53415=CARTESIAN_POINT('',(65.2813246308841,-3.2,-68.39));
#53416=CARTESIAN_POINT('',(-84.39,-3.2,-68.39));
#53417=CARTESIAN_POINT('',(66.8813246308841,-3.2,-68.39));
#53418=CARTESIAN_POINT('',(-84.39,-3.2,-68.39));
#53419=CARTESIAN_POINT('',(66.8813246308841,-3.2,-66.39));
#53420=CARTESIAN_POINT('',(65.2813246308841,-3.2,69.61));
#53421=CARTESIAN_POINT('',(66.8813246308841,-3.2,69.61));
#53422=CARTESIAN_POINT('',(-84.39,-3.2,69.61));
#53423=CARTESIAN_POINT('',(57.938675369116,-3.2,69.61));
#53424=CARTESIAN_POINT('',(-84.39,-3.2,69.61));
#53425=CARTESIAN_POINT('',(56.338675369116,-3.2,69.61));
#53426=CARTESIAN_POINT('',(-84.39,-3.2,69.61));
#53427=CARTESIAN_POINT('',(56.338675369116,-3.2,65.61));
#53428=CARTESIAN_POINT('',(56.338675369116,-3.2,65.61));
#53429=CARTESIAN_POINT('',(57.938675369116,-3.2,65.61));
#53430=CARTESIAN_POINT('',(-84.39,-3.2,65.61));
#53431=CARTESIAN_POINT('',(65.2813246308841,-3.2,65.61));
#53432=CARTESIAN_POINT('',(-84.39,-3.2,65.61));
#53433=CARTESIAN_POINT('',(66.8813246308841,-3.2,65.61));
#53434=CARTESIAN_POINT('',(-84.39,-3.2,65.61));
#53435=CARTESIAN_POINT('',(66.8813246308841,-3.2,67.61));
#53436=CARTESIAN_POINT('',(-44.7186753691159,-3.2,-64.39));
#53437=CARTESIAN_POINT('',(-43.1186753691159,-3.2,-64.39));
#53438=CARTESIAN_POINT('',(-84.39,-3.2,-64.39));
#53439=CARTESIAN_POINT('',(-52.061324630884,-3.2,-64.39));
#53440=CARTESIAN_POINT('',(-84.39,-3.2,-64.39));
#53441=CARTESIAN_POINT('',(-53.661324630884,-3.2,-64.39));
#53442=CARTESIAN_POINT('',(-84.39,-3.2,-64.39));
#53443=CARTESIAN_POINT('',(-53.661324630884,-3.2,-68.39));
#53444=CARTESIAN_POINT('',(-53.661324630884,-3.2,-68.39));
#53445=CARTESIAN_POINT('',(-52.061324630884,-3.2,-68.39));
#53446=CARTESIAN_POINT('',(-84.39,-3.2,-68.39));
#53447=CARTESIAN_POINT('',(-44.7186753691159,-3.2,-68.39));
#53448=CARTESIAN_POINT('',(-84.39,-3.2,-68.39));
#53449=CARTESIAN_POINT('',(-43.1186753691159,-3.2,-68.39));
#53450=CARTESIAN_POINT('',(-84.39,-3.2,-68.39));
#53451=CARTESIAN_POINT('',(-43.1186753691159,-3.2,-66.39));
#53452=CARTESIAN_POINT('Origin',(-84.39,-4.,80.));
#53453=CARTESIAN_POINT('',(-67.3504246383764,-4.,-80.));
#53454=CARTESIAN_POINT('',(-82.2324777960769,-4.,-80.));
#53455=CARTESIAN_POINT('',(-84.39,-4.,-80.));
#53456=CARTESIAN_POINT('',(-67.3504246383764,-4.,-78.16));
#53457=CARTESIAN_POINT('',(-67.3504246383764,-4.,80.));
#53458=CARTESIAN_POINT('',(-67.1104246383764,-4.,-78.16));
#53459=CARTESIAN_POINT('',(-84.39,-4.,-78.16));
#53460=CARTESIAN_POINT('',(-67.1104246383764,-4.00000000000001,-78.4));
#53461=CARTESIAN_POINT('',(-67.1104246383764,-4.,80.));
#53462=CARTESIAN_POINT('',(52.8895753616236,-4.,-78.4));
#53463=CARTESIAN_POINT('',(-67.1104246383764,-4.00000000000001,-78.4));
#53464=CARTESIAN_POINT('',(52.8895753616236,-4.,-78.16));
#53465=CARTESIAN_POINT('',(52.8895753616236,-4.,80.));
#53466=CARTESIAN_POINT('',(53.1295753616236,-4.,-78.16));
#53467=CARTESIAN_POINT('',(-84.39,-4.,-78.16));
#53468=CARTESIAN_POINT('',(53.1295753616236,-4.,-80.));
#53469=CARTESIAN_POINT('',(53.1295753616241,-4.,79.9999999999995));
#53470=CARTESIAN_POINT('',(68.4524777960769,-4.,-80.));
#53471=CARTESIAN_POINT('',(-84.39,-4.,-80.));
#53472=CARTESIAN_POINT('',(68.4524777960769,-4.,-70.));
#53473=CARTESIAN_POINT('',(68.4524777960769,-4.,80.));
#53474=CARTESIAN_POINT('',(69.01,-4.,-68.8330657242578));
#53475=CARTESIAN_POINT('Origin',(69.9524777960769,-4.,-70.));
#53476=CARTESIAN_POINT('',(69.01,-4.,68.8330657242578));
#53477=CARTESIAN_POINT('',(69.01,-4.,80.));
#53478=CARTESIAN_POINT('',(68.4524777960769,-4.,70.));
#53479=CARTESIAN_POINT('Origin',(69.9524777960769,-4.,70.));
#53480=CARTESIAN_POINT('',(68.4524777960769,-4.,80.));
#53481=CARTESIAN_POINT('',(68.4524777960769,-4.,80.));
#53482=CARTESIAN_POINT('',(53.1295753616236,-4.,80.));
#53483=CARTESIAN_POINT('',(-84.39,-4.,80.));
#53484=CARTESIAN_POINT('',(53.1295753616236,-4.,78.16));
#53485=CARTESIAN_POINT('',(53.1295753616236,-4.,80.0000000000005));
#53486=CARTESIAN_POINT('',(52.8895753616236,-4.,78.16));
#53487=CARTESIAN_POINT('',(-84.39,-4.,78.16));
#53488=CARTESIAN_POINT('',(52.8895753616236,-3.99999999999999,78.4));
#53489=CARTESIAN_POINT('',(52.8895753616236,-4.,80.));
#53490=CARTESIAN_POINT('',(-67.1104246383764,-4.,78.4));
#53491=CARTESIAN_POINT('',(52.8895753616236,-3.99999999999999,78.4));
#53492=CARTESIAN_POINT('',(-67.1104246383764,-4.,78.16));
#53493=CARTESIAN_POINT('',(-67.1104246383764,-4.,80.));
#53494=CARTESIAN_POINT('',(-67.3504246383764,-4.,78.16));
#53495=CARTESIAN_POINT('',(-84.39,-4.,78.16));
#53496=CARTESIAN_POINT('',(-67.3504246383764,-4.,80.));
#53497=CARTESIAN_POINT('',(-67.3504246383764,-4.,80.));
#53498=CARTESIAN_POINT('',(-82.2324777960769,-4.,80.));
#53499=CARTESIAN_POINT('',(-84.39,-4.,80.));
#53500=CARTESIAN_POINT('',(-82.2324777960769,-4.,70.));
#53501=CARTESIAN_POINT('',(-82.2324777960769,-4.,80.));
#53502=CARTESIAN_POINT('',(-82.79,-4.,68.8330657242578));
#53503=CARTESIAN_POINT('Origin',(-83.7324777960769,-4.,70.));
#53504=CARTESIAN_POINT('',(-82.79,-4.,-68.8330657242578));
#53505=CARTESIAN_POINT('',(-82.79,-4.,80.));
#53506=CARTESIAN_POINT('',(-82.2324777960769,-4.,-70.));
#53507=CARTESIAN_POINT('Origin',(-83.7324777960769,-4.,-70.));
#53508=CARTESIAN_POINT('',(-82.2324777960769,-4.,80.));
#53509=CARTESIAN_POINT('',(56.338675369116,-4.,-68.39));
#53510=CARTESIAN_POINT('',(66.8813246308841,-4.,-68.39));
#53511=CARTESIAN_POINT('',(57.61,-4.,-68.39));
#53512=CARTESIAN_POINT('',(56.338675369116,-4.,-64.39));
#53513=CARTESIAN_POINT('',(56.338675369116,-4.,-66.39));
#53514=CARTESIAN_POINT('',(66.8813246308841,-4.,-64.39));
#53515=CARTESIAN_POINT('',(57.61,-4.,-64.39));
#53516=CARTESIAN_POINT('',(66.8813246308841,-4.,-66.39));
#53517=CARTESIAN_POINT('',(56.338675369116,-4.,65.61));
#53518=CARTESIAN_POINT('',(66.8813246308841,-4.,65.61));
#53519=CARTESIAN_POINT('',(57.61,-4.,65.61));
#53520=CARTESIAN_POINT('',(56.338675369116,-4.,69.61));
#53521=CARTESIAN_POINT('',(56.338675369116,-4.,67.61));
#53522=CARTESIAN_POINT('',(66.8813246308841,-4.,69.61));
#53523=CARTESIAN_POINT('',(57.61,-4.,69.61));
#53524=CARTESIAN_POINT('',(66.8813246308841,-4.,67.61));
#53525=CARTESIAN_POINT('',(-53.661324630884,-4.,65.61));
#53526=CARTESIAN_POINT('',(-43.1186753691159,-4.,65.61));
#53527=CARTESIAN_POINT('',(-52.39,-4.,65.61));
#53528=CARTESIAN_POINT('',(-53.661324630884,-4.,69.61));
#53529=CARTESIAN_POINT('',(-53.661324630884,-4.,67.61));
#53530=CARTESIAN_POINT('',(-43.1186753691159,-4.,69.61));
#53531=CARTESIAN_POINT('',(-52.39,-4.,69.61));
#53532=CARTESIAN_POINT('',(-43.1186753691159,-4.,67.61));
#53533=CARTESIAN_POINT('',(-53.661324630884,-4.,-68.39));
#53534=CARTESIAN_POINT('',(-43.1186753691159,-4.,-68.39));
#53535=CARTESIAN_POINT('',(-52.39,-4.,-68.39));
#53536=CARTESIAN_POINT('',(-53.661324630884,-4.,-64.39));
#53537=CARTESIAN_POINT('',(-53.661324630884,-4.,-66.39));
#53538=CARTESIAN_POINT('',(-43.1186753691159,-4.,-64.39));
#53539=CARTESIAN_POINT('',(-52.39,-4.,-64.39));
#53540=CARTESIAN_POINT('',(-43.1186753691159,-4.,-66.39));
#53541=CARTESIAN_POINT('Origin',(-83.59,-2.4,-80.));
#53542=CARTESIAN_POINT('',(-67.3504246383764,-3.20000000000001,-80.));
#53543=CARTESIAN_POINT('',(-82.2324777960769,-2.4,-80.));
#53544=CARTESIAN_POINT('Origin',(-83.59,-2.4,-80.));
#53545=CARTESIAN_POINT('',(53.1295753616236,-3.20000000000001,-80.));
#53546=CARTESIAN_POINT('',(68.4524777960769,-2.4,-80.));
#53547=CARTESIAN_POINT('Origin',(-63.1104246383764,2.79999999999999,79.2));
#53548=CARTESIAN_POINT('',(52.8895753616236,-2.4,79.2));
#53549=CARTESIAN_POINT('',(52.8895753616236,2.80000000000002,79.2));
#53550=CARTESIAN_POINT('',(52.8895753616236,2.80000000000001,79.2));
#53551=CARTESIAN_POINT('',(-67.1104246383764,-2.4,79.2));
#53552=CARTESIAN_POINT('',(-67.1104246383764,-2.4,79.2));
#53553=CARTESIAN_POINT('',(-67.1104246383764,2.79999999999997,79.2));
#53554=CARTESIAN_POINT('',(-67.1104246383764,-3.2,79.2));
#53555=CARTESIAN_POINT('',(-63.1104246383764,6.79999999999999,79.2));
#53556=CARTESIAN_POINT('Origin',(-63.1104246383764,2.79999999999999,79.2));
#53557=CARTESIAN_POINT('',(48.8895753616235,6.80000000000003,79.2));
#53558=CARTESIAN_POINT('',(-63.1104246383764,6.79999999999999,79.2));
#53559=CARTESIAN_POINT('Origin',(48.8895753616236,2.80000000000003,79.2));
#53560=CARTESIAN_POINT('',(-57.3817492692605,3.80000000000003,79.1999999999841));
#53561=CARTESIAN_POINT('',(-57.3817492692605,-0.199999999999971,79.199999999992));
#53562=CARTESIAN_POINT('',(-57.3817492692605,1.80000000000003,79.1999999999841));
#53563=CARTESIAN_POINT('',(-55.7817492692724,-0.199999999999971,79.2));
#53564=CARTESIAN_POINT('',(-63.1104246383764,-0.199999999999971,79.2));
#53565=CARTESIAN_POINT('',(-48.4391000074804,-0.199999999999971,79.2));
#53566=CARTESIAN_POINT('',(-63.1104246383764,-0.199999999999972,79.2));
#53567=CARTESIAN_POINT('',(-46.8391000074924,-0.199999999999969,79.1999999999841));
#53568=CARTESIAN_POINT('',(-63.1104246383764,-0.199999999999971,79.2));
#53569=CARTESIAN_POINT('',(-46.8391000074924,3.80000000000003,79.199999999992));
#53570=CARTESIAN_POINT('',(-46.8391000074924,3.80000000000003,79.1999999999841));
#53571=CARTESIAN_POINT('',(-48.4391000074804,3.80000000000003,79.2));
#53572=CARTESIAN_POINT('',(-63.1104246383764,3.80000000000003,79.2));
#53573=CARTESIAN_POINT('',(-55.7817492692724,3.80000000000003,79.2));
#53574=CARTESIAN_POINT('',(-63.1104246383764,3.80000000000003,79.2));
#53575=CARTESIAN_POINT('',(-63.1104246383764,3.80000000000003,79.2));
#53576=CARTESIAN_POINT('',(33.0591000074924,-0.199999999999946,79.199999999992));
#53577=CARTESIAN_POINT('',(33.0591000074924,3.80000000000005,79.1999999999841));
#53578=CARTESIAN_POINT('',(33.0591000074924,3.80000000000005,79.1999999999841));
#53579=CARTESIAN_POINT('',(34.6591000074805,-0.199999999999947,79.2));
#53580=CARTESIAN_POINT('',(-63.1104246383764,-0.200000000000004,79.2));
#53581=CARTESIAN_POINT('',(42.0017492692724,-0.199999999999943,79.2));
#53582=CARTESIAN_POINT('',(-63.1104246383764,-0.200000000000005,79.2));
#53583=CARTESIAN_POINT('',(43.6017492692605,-0.19999999999994,79.1999999999841));
#53584=CARTESIAN_POINT('',(-63.1104246383764,-0.200000000000004,79.2));
#53585=CARTESIAN_POINT('',(43.6017492692605,3.80000000000006,79.199999999992));
#53586=CARTESIAN_POINT('',(43.6017492692605,1.80000000000006,79.1999999999841));
#53587=CARTESIAN_POINT('',(42.0017492692724,3.80000000000006,79.2));
#53588=CARTESIAN_POINT('',(-63.1104246383764,3.8,79.2));
#53589=CARTESIAN_POINT('',(34.6591000074805,3.80000000000005,79.2));
#53590=CARTESIAN_POINT('',(-63.1104246383764,3.8,79.2));
#53591=CARTESIAN_POINT('',(-63.1104246383764,3.8,79.2));
#53592=CARTESIAN_POINT('Origin',(-63.1104246383764,2.79999999999999,80.));
#53593=CARTESIAN_POINT('',(52.8895753616236,-2.4,80.));
#53594=CARTESIAN_POINT('',(-67.1104246383764,-2.4,80.));
#53595=CARTESIAN_POINT('',(-67.1104246383764,-2.4,80.));
#53596=CARTESIAN_POINT('',(52.8895753616236,2.80000000000002,80.));
#53597=CARTESIAN_POINT('',(52.8895753616236,2.80000000000012,80.));
#53598=CARTESIAN_POINT('',(48.8895753616235,6.80000000000003,80.));
#53599=CARTESIAN_POINT('Origin',(48.8895753616236,2.80000000000003,80.));
#53600=CARTESIAN_POINT('',(-63.1104246383764,6.79999999999999,80.));
#53601=CARTESIAN_POINT('',(-63.1104246383764,6.79999999999999,80.));
#53602=CARTESIAN_POINT('',(-67.1104246383764,2.79999999999997,80.));
#53603=CARTESIAN_POINT('Origin',(-63.1104246383764,2.79999999999999,80.));
#53604=CARTESIAN_POINT('',(-67.1104246383764,2.79999999999999,80.));
#53605=CARTESIAN_POINT('',(-46.8391000074924,3.80000000000003,79.9999999999841));
#53606=CARTESIAN_POINT('',(-57.3817492692605,3.80000000000003,79.999999999992));
#53607=CARTESIAN_POINT('',(-48.1104246383764,3.80000000000003,79.9999999999841));
#53608=CARTESIAN_POINT('',(-46.8391000074924,-0.199999999999972,79.9999999999841));
#53609=CARTESIAN_POINT('',(-46.8391000074924,1.80000000000003,79.9999999999841));
#53610=CARTESIAN_POINT('',(-57.3817492692605,-0.199999999999971,79.9999999999841));
#53611=CARTESIAN_POINT('',(-48.1104246383764,-0.199999999999972,79.9999999999841));
#53612=CARTESIAN_POINT('',(-57.3817492692605,1.80000000000003,79.9999999999841));
#53613=CARTESIAN_POINT('',(33.0591000074924,-0.199999999999949,79.9999999999841));
#53614=CARTESIAN_POINT('',(33.0591000074924,3.80000000000005,79.9999999999841));
#53615=CARTESIAN_POINT('',(33.0591000074924,1.80000000000005,79.9999999999841));
#53616=CARTESIAN_POINT('',(43.6017492692605,3.80000000000006,79.9999999999841));
#53617=CARTESIAN_POINT('',(34.3304246383764,3.80000000000005,79.9999999999841));
#53618=CARTESIAN_POINT('',(43.6017492692605,-0.199999999999941,79.999999999992));
#53619=CARTESIAN_POINT('',(43.6017492692605,1.80000000000006,79.9999999999841));
#53620=CARTESIAN_POINT('',(34.3304246383764,-0.199999999999948,79.9999999999841));
#53621=CARTESIAN_POINT('Origin',(69.81,-2.4,80.));
#53622=CARTESIAN_POINT('',(53.1295753616236,-3.2,80.));
#53623=CARTESIAN_POINT('',(68.4524777960769,-2.4,80.));
#53624=CARTESIAN_POINT('Origin',(69.81,-2.4,80.));
#53625=CARTESIAN_POINT('',(-67.3504246383764,-3.2,80.));
#53626=CARTESIAN_POINT('',(-82.2324777960769,-2.4,80.));
#53627=CARTESIAN_POINT('Origin',(70.61,91.,80.));
#53628=CARTESIAN_POINT('',(70.61,86.,-80.));
#53629=CARTESIAN_POINT('',(70.6100000000008,-1.84247779607696,-80.));
#53630=CARTESIAN_POINT('',(70.61,91.,-80.));
#53631=CARTESIAN_POINT('',(70.61,91.,-75.));
#53632=CARTESIAN_POINT('',(70.61,168.5,2.50000000000003));
#53633=CARTESIAN_POINT('',(70.61,91.,75.));
#53634=CARTESIAN_POINT('',(70.61,91.,80.));
#53635=CARTESIAN_POINT('',(70.61,86.,80.));
#53636=CARTESIAN_POINT('',(70.61,88.5,77.5));
#53637=CARTESIAN_POINT('',(70.61,-1.84247779607696,80.));
#53638=CARTESIAN_POINT('',(70.61,91.,80.));
#53639=CARTESIAN_POINT('',(70.61,-1.84247779607696,70.));
#53640=CARTESIAN_POINT('',(70.61,-1.84247779607696,80.));
#53641=CARTESIAN_POINT('',(70.61,-2.4,68.8330657242578));
#53642=CARTESIAN_POINT('Origin',(70.61,-3.34247779607697,70.));
#53643=CARTESIAN_POINT('',(70.61,-2.4,-68.8330657242578));
#53644=CARTESIAN_POINT('',(70.61,-2.4,80.));
#53645=CARTESIAN_POINT('',(70.61,-1.84247779607696,-70.));
#53646=CARTESIAN_POINT('Origin',(70.61,-3.34247779607697,-70.));
#53647=CARTESIAN_POINT('',(70.61,-1.84247779607696,80.));
#53648=CARTESIAN_POINT('',(70.61,46.0787611019615,-66.5));
#53649=CARTESIAN_POINT('',(70.61,1.35867816760341E-14,-66.5));
#53650=CARTESIAN_POINT('',(70.61,46.0787611019615,-69.5));
#53651=CARTESIAN_POINT('',(70.61,1.35867816760341E-14,-69.5));
#53652=CARTESIAN_POINT('Origin',(70.61,46.0787611019615,-68.));
#53653=CARTESIAN_POINT('',(70.61,46.0787611019615,-21.5));
#53654=CARTESIAN_POINT('',(70.61,1.35867816760341E-14,-21.5));
#53655=CARTESIAN_POINT('',(70.61,46.0787611019615,-24.5));
#53656=CARTESIAN_POINT('',(70.61,1.35867816760341E-14,-24.5));
#53657=CARTESIAN_POINT('Origin',(70.61,46.0787611019615,-23.));
#53658=CARTESIAN_POINT('',(70.61,46.0787611019615,-16.5));
#53659=CARTESIAN_POINT('',(70.61,1.35867816760341E-14,-16.5));
#53660=CARTESIAN_POINT('',(70.61,46.0787611019615,-19.5));
#53661=CARTESIAN_POINT('',(70.61,1.35867816760341E-14,-19.5));
#53662=CARTESIAN_POINT('Origin',(70.61,46.0787611019615,-18.));
#53663=CARTESIAN_POINT('',(70.61,46.0787611019615,-11.5));
#53664=CARTESIAN_POINT('',(70.61,1.35867816760341E-14,-11.5));
#53665=CARTESIAN_POINT('',(70.61,46.0787611019615,-14.5));
#53666=CARTESIAN_POINT('',(70.61,1.35867816760341E-14,-14.5));
#53667=CARTESIAN_POINT('Origin',(70.61,46.0787611019615,-13.));
#53668=CARTESIAN_POINT('',(70.61,46.0787611019615,-41.5));
#53669=CARTESIAN_POINT('',(70.61,1.35867816760341E-14,-41.5));
#53670=CARTESIAN_POINT('',(70.61,46.0787611019615,-44.5));
#53671=CARTESIAN_POINT('',(70.61,1.35867816760341E-14,-44.5));
#53672=CARTESIAN_POINT('Origin',(70.61,46.0787611019615,-43.));
#53673=CARTESIAN_POINT('',(70.61,46.0787611019615,-46.5));
#53674=CARTESIAN_POINT('',(70.61,1.35867816760341E-14,-46.5));
#53675=CARTESIAN_POINT('',(70.61,46.0787611019615,-49.5));
#53676=CARTESIAN_POINT('',(70.61,1.35867816760341E-14,-49.5));
#53677=CARTESIAN_POINT('Origin',(70.61,46.0787611019615,-48.));
#53678=CARTESIAN_POINT('',(70.61,46.0787611019615,-51.5));
#53679=CARTESIAN_POINT('',(70.61,1.35867816760341E-14,-51.5));
#53680=CARTESIAN_POINT('',(70.61,46.0787611019615,-54.5));
#53681=CARTESIAN_POINT('',(70.61,1.35867816760341E-14,-54.5));
#53682=CARTESIAN_POINT('Origin',(70.61,46.0787611019615,-53.));
#53683=CARTESIAN_POINT('',(70.61,46.0787611019615,-56.5));
#53684=CARTESIAN_POINT('',(70.61,1.35867816760341E-14,-56.5));
#53685=CARTESIAN_POINT('',(70.61,46.0787611019615,-59.5));
#53686=CARTESIAN_POINT('',(70.61,1.35867816760341E-14,-59.5));
#53687=CARTESIAN_POINT('Origin',(70.61,46.0787611019615,-58.));
#53688=CARTESIAN_POINT('',(70.61,46.0787611019615,-61.5));
#53689=CARTESIAN_POINT('',(70.61,1.35867816760341E-14,-61.5));
#53690=CARTESIAN_POINT('',(70.61,46.0787611019615,-64.5));
#53691=CARTESIAN_POINT('',(70.61,1.35867816760341E-14,-64.5));
#53692=CARTESIAN_POINT('Origin',(70.61,46.0787611019615,-63.));
#53693=CARTESIAN_POINT('',(70.61,46.0787611019615,-26.5));
#53694=CARTESIAN_POINT('',(70.61,1.35867816760341E-14,-26.5));
#53695=CARTESIAN_POINT('',(70.61,46.0787611019615,-29.5));
#53696=CARTESIAN_POINT('',(70.61,1.35867816760341E-14,-29.5));
#53697=CARTESIAN_POINT('Origin',(70.61,46.0787611019615,-28.));
#53698=CARTESIAN_POINT('',(70.61,46.0787611019615,-31.5));
#53699=CARTESIAN_POINT('',(70.61,1.35867816760341E-14,-31.5));
#53700=CARTESIAN_POINT('',(70.61,46.0787611019615,-34.5));
#53701=CARTESIAN_POINT('',(70.61,1.35867816760341E-14,-34.5));
#53702=CARTESIAN_POINT('Origin',(70.61,46.0787611019615,-33.));
#53703=CARTESIAN_POINT('',(70.61,46.0787611019615,-36.5));
#53704=CARTESIAN_POINT('',(70.61,1.35867816760341E-14,-36.5));
#53705=CARTESIAN_POINT('',(70.61,46.0787611019615,-39.5));
#53706=CARTESIAN_POINT('',(70.61,1.35867816760341E-14,-39.5));
#53707=CARTESIAN_POINT('Origin',(70.61,46.0787611019615,-38.));
#53708=CARTESIAN_POINT('',(70.61,18.0787611019615,16.5));
#53709=CARTESIAN_POINT('',(70.61,1.35867816760341E-14,16.5));
#53710=CARTESIAN_POINT('',(70.61,18.0787611019615,19.5));
#53711=CARTESIAN_POINT('Origin',(70.61,18.0787611019615,18.));
#53712=CARTESIAN_POINT('',(70.61,1.35867816760341E-14,19.5));
#53713=CARTESIAN_POINT('',(70.61,18.0787611019615,21.5));
#53714=CARTESIAN_POINT('',(70.61,1.35867816760341E-14,21.5));
#53715=CARTESIAN_POINT('',(70.61,18.0787611019615,24.5));
#53716=CARTESIAN_POINT('Origin',(70.61,18.0787611019615,23.));
#53717=CARTESIAN_POINT('',(70.61,1.35867816760341E-14,24.5));
#53718=CARTESIAN_POINT('',(70.61,18.0787611019615,26.5));
#53719=CARTESIAN_POINT('',(70.61,1.35867816760341E-14,26.5));
#53720=CARTESIAN_POINT('',(70.61,18.0787611019615,29.5));
#53721=CARTESIAN_POINT('Origin',(70.61,18.0787611019615,28.));
#53722=CARTESIAN_POINT('',(70.61,1.35867816760341E-14,29.5));
#53723=CARTESIAN_POINT('',(70.61,18.0787611019615,11.5));
#53724=CARTESIAN_POINT('',(70.61,1.35867816760341E-14,11.5));
#53725=CARTESIAN_POINT('',(70.61,18.0787611019615,14.5));
#53726=CARTESIAN_POINT('Origin',(70.61,18.0787611019615,13.));
#53727=CARTESIAN_POINT('',(70.61,1.35867816760341E-14,14.5));
#53728=CARTESIAN_POINT('',(70.61,18.0787611019615,51.5));
#53729=CARTESIAN_POINT('',(70.61,1.35867816760341E-14,51.5));
#53730=CARTESIAN_POINT('',(70.61,18.0787611019615,54.5));
#53731=CARTESIAN_POINT('Origin',(70.61,18.0787611019615,53.));
#53732=CARTESIAN_POINT('',(70.61,1.35867816760341E-14,54.5));
#53733=CARTESIAN_POINT('',(70.61,18.0787611019615,46.5));
#53734=CARTESIAN_POINT('',(70.61,1.35867816760341E-14,46.5));
#53735=CARTESIAN_POINT('',(70.61,18.0787611019615,49.5));
#53736=CARTESIAN_POINT('Origin',(70.61,18.0787611019615,48.));
#53737=CARTESIAN_POINT('',(70.61,1.35867816760341E-14,49.5));
#53738=CARTESIAN_POINT('',(70.61,18.0787611019615,41.5));
#53739=CARTESIAN_POINT('',(70.61,1.35867816760341E-14,41.5));
#53740=CARTESIAN_POINT('',(70.61,18.0787611019615,44.5));
#53741=CARTESIAN_POINT('Origin',(70.61,18.0787611019615,43.));
#53742=CARTESIAN_POINT('',(70.61,1.35867816760341E-14,44.5));
#53743=CARTESIAN_POINT('',(70.61,18.0787611019615,31.5));
#53744=CARTESIAN_POINT('',(70.61,1.35867816760341E-14,31.5));
#53745=CARTESIAN_POINT('',(70.61,18.0787611019615,34.5));
#53746=CARTESIAN_POINT('Origin',(70.61,18.0787611019615,33.));
#53747=CARTESIAN_POINT('',(70.61,1.35867816760341E-14,34.5));
#53748=CARTESIAN_POINT('',(70.61,18.0787611019615,36.5));
#53749=CARTESIAN_POINT('',(70.61,1.35867816760341E-14,36.5));
#53750=CARTESIAN_POINT('',(70.61,18.0787611019615,39.5));
#53751=CARTESIAN_POINT('Origin',(70.61,18.0787611019615,38.));
#53752=CARTESIAN_POINT('',(70.61,1.35867816760341E-14,39.5));
#53753=CARTESIAN_POINT('',(70.61,18.0787611019615,56.5));
#53754=CARTESIAN_POINT('',(70.61,1.35867816760341E-14,56.5));
#53755=CARTESIAN_POINT('',(70.61,18.0787611019615,59.5));
#53756=CARTESIAN_POINT('Origin',(70.61,18.0787611019615,58.));
#53757=CARTESIAN_POINT('',(70.61,1.35867816760341E-14,59.5));
#53758=CARTESIAN_POINT('',(70.61,18.0787611019615,61.5));
#53759=CARTESIAN_POINT('',(70.61,1.35867816760341E-14,61.5));
#53760=CARTESIAN_POINT('',(70.61,18.0787611019615,64.5));
#53761=CARTESIAN_POINT('Origin',(70.61,18.0787611019615,63.));
#53762=CARTESIAN_POINT('',(70.61,1.35867816760341E-14,64.5));
#53763=CARTESIAN_POINT('',(70.61,18.0787611019615,66.5));
#53764=CARTESIAN_POINT('',(70.61,1.35867816760341E-14,66.5));
#53765=CARTESIAN_POINT('',(70.61,18.0787611019615,69.5));
#53766=CARTESIAN_POINT('Origin',(70.61,18.0787611019615,68.));
#53767=CARTESIAN_POINT('',(70.61,1.35867816760341E-14,69.5));
#53768=CARTESIAN_POINT('',(70.61,46.0787611019615,36.5));
#53769=CARTESIAN_POINT('',(70.61,1.35867816760341E-14,36.5));
#53770=CARTESIAN_POINT('',(70.61,46.0787611019615,39.5));
#53771=CARTESIAN_POINT('Origin',(70.61,46.0787611019615,38.));
#53772=CARTESIAN_POINT('',(70.61,1.35867816760341E-14,39.5));
#53773=CARTESIAN_POINT('',(70.61,46.0787611019615,31.5));
#53774=CARTESIAN_POINT('',(70.61,1.35867816760341E-14,31.5));
#53775=CARTESIAN_POINT('',(70.61,46.0787611019615,34.5));
#53776=CARTESIAN_POINT('Origin',(70.61,46.0787611019615,33.));
#53777=CARTESIAN_POINT('',(70.61,1.35867816760341E-14,34.5));
#53778=CARTESIAN_POINT('',(70.61,46.0787611019615,26.5));
#53779=CARTESIAN_POINT('',(70.61,1.35867816760341E-14,26.5));
#53780=CARTESIAN_POINT('',(70.61,46.0787611019615,29.5));
#53781=CARTESIAN_POINT('Origin',(70.61,46.0787611019615,28.));
#53782=CARTESIAN_POINT('',(70.61,1.35867816760341E-14,29.5));
#53783=CARTESIAN_POINT('',(70.61,46.0787611019615,61.5));
#53784=CARTESIAN_POINT('',(70.61,1.35867816760341E-14,61.5));
#53785=CARTESIAN_POINT('',(70.61,46.0787611019615,64.5));
#53786=CARTESIAN_POINT('Origin',(70.61,46.0787611019615,63.));
#53787=CARTESIAN_POINT('',(70.61,1.35867816760341E-14,64.5));
#53788=CARTESIAN_POINT('',(70.61,46.0787611019615,56.5));
#53789=CARTESIAN_POINT('',(70.61,1.35867816760341E-14,56.5));
#53790=CARTESIAN_POINT('',(70.61,46.0787611019615,59.5));
#53791=CARTESIAN_POINT('Origin',(70.61,46.0787611019615,58.));
#53792=CARTESIAN_POINT('',(70.61,1.35867816760341E-14,59.5));
#53793=CARTESIAN_POINT('',(70.61,46.0787611019615,51.5));
#53794=CARTESIAN_POINT('',(70.61,1.35867816760341E-14,51.5));
#53795=CARTESIAN_POINT('',(70.61,46.0787611019615,54.5));
#53796=CARTESIAN_POINT('Origin',(70.61,46.0787611019615,53.));
#53797=CARTESIAN_POINT('',(70.61,1.35867816760341E-14,54.5));
#53798=CARTESIAN_POINT('',(70.61,46.0787611019615,46.5));
#53799=CARTESIAN_POINT('',(70.61,1.35867816760341E-14,46.5));
#53800=CARTESIAN_POINT('',(70.61,46.0787611019615,49.5));
#53801=CARTESIAN_POINT('Origin',(70.61,46.0787611019615,48.));
#53802=CARTESIAN_POINT('',(70.61,1.35867816760341E-14,49.5));
#53803=CARTESIAN_POINT('',(70.61,46.0787611019615,41.5));
#53804=CARTESIAN_POINT('',(70.61,1.35867816760341E-14,41.5));
#53805=CARTESIAN_POINT('',(70.61,46.0787611019615,44.5));
#53806=CARTESIAN_POINT('Origin',(70.61,46.0787611019615,43.));
#53807=CARTESIAN_POINT('',(70.61,1.35867816760341E-14,44.5));
#53808=CARTESIAN_POINT('',(70.61,46.0787611019615,11.5));
#53809=CARTESIAN_POINT('',(70.61,1.35867816760341E-14,11.5));
#53810=CARTESIAN_POINT('',(70.61,46.0787611019615,14.5));
#53811=CARTESIAN_POINT('Origin',(70.61,46.0787611019615,13.));
#53812=CARTESIAN_POINT('',(70.61,1.35867816760341E-14,14.5));
#53813=CARTESIAN_POINT('',(70.61,46.0787611019615,16.5));
#53814=CARTESIAN_POINT('',(70.61,1.35867816760341E-14,16.5));
#53815=CARTESIAN_POINT('',(70.61,46.0787611019615,19.5));
#53816=CARTESIAN_POINT('Origin',(70.61,46.0787611019615,18.));
#53817=CARTESIAN_POINT('',(70.61,1.35867816760341E-14,19.5));
#53818=CARTESIAN_POINT('',(70.61,46.0787611019615,21.5));
#53819=CARTESIAN_POINT('',(70.61,1.35867816760341E-14,21.5));
#53820=CARTESIAN_POINT('',(70.61,46.0787611019615,24.5));
#53821=CARTESIAN_POINT('Origin',(70.61,46.0787611019615,23.));
#53822=CARTESIAN_POINT('',(70.61,1.35867816760341E-14,24.5));
#53823=CARTESIAN_POINT('',(70.61,46.0787611019615,66.5));
#53824=CARTESIAN_POINT('',(70.61,1.35867816760341E-14,66.5));
#53825=CARTESIAN_POINT('',(70.61,46.0787611019615,69.5));
#53826=CARTESIAN_POINT('Origin',(70.61,46.0787611019615,68.));
#53827=CARTESIAN_POINT('',(70.61,1.35867816760341E-14,69.5));
#53828=CARTESIAN_POINT('',(70.61,18.0787611019615,-66.5));
#53829=CARTESIAN_POINT('',(70.61,1.35867816760341E-14,-66.5));
#53830=CARTESIAN_POINT('',(70.61,18.0787611019615,-69.5));
#53831=CARTESIAN_POINT('',(70.61,1.35867816760341E-14,-69.5));
#53832=CARTESIAN_POINT('Origin',(70.61,18.0787611019615,-68.));
#53833=CARTESIAN_POINT('',(70.61,18.0787611019615,-61.5));
#53834=CARTESIAN_POINT('',(70.61,1.35867816760341E-14,-61.5));
#53835=CARTESIAN_POINT('',(70.61,18.0787611019615,-64.5));
#53836=CARTESIAN_POINT('',(70.61,1.35867816760341E-14,-64.5));
#53837=CARTESIAN_POINT('Origin',(70.61,18.0787611019615,-63.));
#53838=CARTESIAN_POINT('',(70.61,18.0787611019615,-56.5));
#53839=CARTESIAN_POINT('',(70.61,1.35867816760341E-14,-56.5));
#53840=CARTESIAN_POINT('',(70.61,18.0787611019615,-59.5));
#53841=CARTESIAN_POINT('',(70.61,1.35867816760341E-14,-59.5));
#53842=CARTESIAN_POINT('Origin',(70.61,18.0787611019615,-58.));
#53843=CARTESIAN_POINT('',(70.61,18.0787611019615,-36.5));
#53844=CARTESIAN_POINT('',(70.61,1.35867816760341E-14,-36.5));
#53845=CARTESIAN_POINT('',(70.61,18.0787611019615,-39.5));
#53846=CARTESIAN_POINT('',(70.61,1.35867816760341E-14,-39.5));
#53847=CARTESIAN_POINT('Origin',(70.61,18.0787611019615,-38.));
#53848=CARTESIAN_POINT('',(70.61,18.0787611019615,-31.5));
#53849=CARTESIAN_POINT('',(70.61,1.35867816760341E-14,-31.5));
#53850=CARTESIAN_POINT('',(70.61,18.0787611019615,-34.5));
#53851=CARTESIAN_POINT('',(70.61,1.35867816760341E-14,-34.5));
#53852=CARTESIAN_POINT('Origin',(70.61,18.0787611019615,-33.));
#53853=CARTESIAN_POINT('',(70.61,18.0787611019615,-41.5));
#53854=CARTESIAN_POINT('',(70.61,1.35867816760341E-14,-41.5));
#53855=CARTESIAN_POINT('',(70.61,18.0787611019615,-44.5));
#53856=CARTESIAN_POINT('',(70.61,1.35867816760341E-14,-44.5));
#53857=CARTESIAN_POINT('Origin',(70.61,18.0787611019615,-43.));
#53858=CARTESIAN_POINT('',(70.61,18.0787611019615,-46.5));
#53859=CARTESIAN_POINT('',(70.61,1.35867816760341E-14,-46.5));
#53860=CARTESIAN_POINT('',(70.61,18.0787611019615,-49.5));
#53861=CARTESIAN_POINT('',(70.61,1.35867816760341E-14,-49.5));
#53862=CARTESIAN_POINT('Origin',(70.61,18.0787611019615,-48.));
#53863=CARTESIAN_POINT('',(70.61,18.0787611019615,-51.5));
#53864=CARTESIAN_POINT('',(70.61,1.35867816760341E-14,-51.5));
#53865=CARTESIAN_POINT('',(70.61,18.0787611019615,-54.5));
#53866=CARTESIAN_POINT('',(70.61,1.35867816760341E-14,-54.5));
#53867=CARTESIAN_POINT('Origin',(70.61,18.0787611019615,-53.));
#53868=CARTESIAN_POINT('',(70.61,18.0787611019615,-11.5));
#53869=CARTESIAN_POINT('',(70.61,1.35867816760341E-14,-11.5));
#53870=CARTESIAN_POINT('',(70.61,18.0787611019615,-14.5));
#53871=CARTESIAN_POINT('',(70.61,1.35867816760341E-14,-14.5));
#53872=CARTESIAN_POINT('Origin',(70.61,18.0787611019615,-13.));
#53873=CARTESIAN_POINT('',(70.61,18.0787611019615,-26.5));
#53874=CARTESIAN_POINT('',(70.61,1.35867816760341E-14,-26.5));
#53875=CARTESIAN_POINT('',(70.61,18.0787611019615,-29.5));
#53876=CARTESIAN_POINT('',(70.61,1.35867816760341E-14,-29.5));
#53877=CARTESIAN_POINT('Origin',(70.61,18.0787611019615,-28.));
#53878=CARTESIAN_POINT('',(70.61,18.0787611019615,-21.5));
#53879=CARTESIAN_POINT('',(70.61,1.35867816760341E-14,-21.5));
#53880=CARTESIAN_POINT('',(70.61,18.0787611019615,-24.5));
#53881=CARTESIAN_POINT('',(70.61,1.35867816760341E-14,-24.5));
#53882=CARTESIAN_POINT('Origin',(70.61,18.0787611019615,-23.));
#53883=CARTESIAN_POINT('',(70.61,18.0787611019615,-16.5));
#53884=CARTESIAN_POINT('',(70.61,1.35867816760341E-14,-16.5));
#53885=CARTESIAN_POINT('',(70.61,18.0787611019615,-19.5));
#53886=CARTESIAN_POINT('',(70.61,1.35867816760341E-14,-19.5));
#53887=CARTESIAN_POINT('Origin',(70.61,18.0787611019615,-18.));
#53888=CARTESIAN_POINT('Origin',(69.81,91.,80.));
#53889=CARTESIAN_POINT('',(69.81,91.,75.));
#53890=CARTESIAN_POINT('',(69.81,91.,-75.));
#53891=CARTESIAN_POINT('',(69.81,91.,80.));
#53892=CARTESIAN_POINT('',(69.81,86.,-80.));
#53893=CARTESIAN_POINT('',(69.81,86.,-80.));
#53894=CARTESIAN_POINT('',(69.81,-1.84247779607698,-80.));
#53895=CARTESIAN_POINT('',(69.81,91.,-80.));
#53896=CARTESIAN_POINT('',(69.81,-1.84247779607698,-70.));
#53897=CARTESIAN_POINT('',(69.81,-1.84247779607698,-70.));
#53898=CARTESIAN_POINT('',(69.81,-2.4,-68.8330657242578));
#53899=CARTESIAN_POINT('Origin',(69.81,-3.34247779607698,-70.));
#53900=CARTESIAN_POINT('',(69.81,-2.4,68.8330657242578));
#53901=CARTESIAN_POINT('',(69.81,-2.4,80.));
#53902=CARTESIAN_POINT('',(69.81,-1.84247779607698,70.));
#53903=CARTESIAN_POINT('Origin',(69.81,-3.34247779607698,70.));
#53904=CARTESIAN_POINT('',(69.81,-1.84247779607698,80.));
#53905=CARTESIAN_POINT('',(69.81,-1.84247779607698,70.));
#53906=CARTESIAN_POINT('',(69.81,86.,80.));
#53907=CARTESIAN_POINT('',(69.81,91.,80.));
#53908=CARTESIAN_POINT('',(69.81,91.,75.));
#53909=CARTESIAN_POINT('',(69.81,18.0787611019615,-16.5));
#53910=CARTESIAN_POINT('',(69.81,91.,-16.5));
#53911=CARTESIAN_POINT('',(69.81,18.0787611019615,-19.5));
#53912=CARTESIAN_POINT('Origin',(69.81,18.0787611019615,-18.));
#53913=CARTESIAN_POINT('',(69.81,91.,-19.5));
#53914=CARTESIAN_POINT('',(69.81,18.0787611019615,-21.5));
#53915=CARTESIAN_POINT('',(69.81,91.,-21.5));
#53916=CARTESIAN_POINT('',(69.81,18.0787611019615,-24.5));
#53917=CARTESIAN_POINT('Origin',(69.81,18.0787611019615,-23.));
#53918=CARTESIAN_POINT('',(69.81,91.,-24.5));
#53919=CARTESIAN_POINT('',(69.81,46.0787611019615,-21.5));
#53920=CARTESIAN_POINT('',(69.81,91.,-21.5));
#53921=CARTESIAN_POINT('',(69.81,46.0787611019615,-24.5));
#53922=CARTESIAN_POINT('Origin',(69.81,46.0787611019615,-23.));
#53923=CARTESIAN_POINT('',(69.81,91.,-24.5));
#53924=CARTESIAN_POINT('',(69.81,46.0787611019615,-11.5));
#53925=CARTESIAN_POINT('',(69.81,91.,-11.5));
#53926=CARTESIAN_POINT('',(69.81,46.0787611019615,-14.5));
#53927=CARTESIAN_POINT('Origin',(69.81,46.0787611019615,-13.));
#53928=CARTESIAN_POINT('',(69.81,91.,-14.5));
#53929=CARTESIAN_POINT('',(69.81,46.0787611019615,-46.5));
#53930=CARTESIAN_POINT('',(69.81,91.,-46.5));
#53931=CARTESIAN_POINT('',(69.81,46.0787611019615,-49.5));
#53932=CARTESIAN_POINT('Origin',(69.81,46.0787611019615,-48.));
#53933=CARTESIAN_POINT('',(69.81,91.,-49.5));
#53934=CARTESIAN_POINT('',(69.81,46.0787611019615,-56.5));
#53935=CARTESIAN_POINT('',(69.81,91.,-56.5));
#53936=CARTESIAN_POINT('',(69.81,46.0787611019615,-59.5));
#53937=CARTESIAN_POINT('Origin',(69.81,46.0787611019615,-58.));
#53938=CARTESIAN_POINT('',(69.81,91.,-59.5));
#53939=CARTESIAN_POINT('',(69.81,46.0787611019615,-26.5));
#53940=CARTESIAN_POINT('',(69.81,91.,-26.5));
#53941=CARTESIAN_POINT('',(69.81,46.0787611019615,-29.5));
#53942=CARTESIAN_POINT('Origin',(69.81,46.0787611019615,-28.));
#53943=CARTESIAN_POINT('',(69.81,91.,-29.5));
#53944=CARTESIAN_POINT('',(69.81,18.0787611019615,-31.5));
#53945=CARTESIAN_POINT('',(69.81,91.,-31.5));
#53946=CARTESIAN_POINT('',(69.81,18.0787611019615,-34.5));
#53947=CARTESIAN_POINT('Origin',(69.81,18.0787611019615,-33.));
#53948=CARTESIAN_POINT('',(69.81,91.,-34.5));
#53949=CARTESIAN_POINT('',(69.81,18.0787611019615,-36.5));
#53950=CARTESIAN_POINT('',(69.81,91.,-36.5));
#53951=CARTESIAN_POINT('',(69.81,18.0787611019615,-39.5));
#53952=CARTESIAN_POINT('Origin',(69.81,18.0787611019615,-38.));
#53953=CARTESIAN_POINT('',(69.81,91.,-39.5));
#53954=CARTESIAN_POINT('',(69.81,18.0787611019615,-56.5));
#53955=CARTESIAN_POINT('',(69.81,91.,-56.5));
#53956=CARTESIAN_POINT('',(69.81,18.0787611019615,-59.5));
#53957=CARTESIAN_POINT('Origin',(69.81,18.0787611019615,-58.));
#53958=CARTESIAN_POINT('',(69.81,91.,-59.5));
#53959=CARTESIAN_POINT('',(69.81,18.0787611019615,-61.5));
#53960=CARTESIAN_POINT('',(69.81,91.,-61.5));
#53961=CARTESIAN_POINT('',(69.81,18.0787611019615,-64.5));
#53962=CARTESIAN_POINT('Origin',(69.81,18.0787611019615,-63.));
#53963=CARTESIAN_POINT('',(69.81,91.,-64.5));
#53964=CARTESIAN_POINT('',(69.81,18.0787611019615,-66.5));
#53965=CARTESIAN_POINT('',(69.81,91.,-66.5));
#53966=CARTESIAN_POINT('',(69.81,18.0787611019615,-69.5));
#53967=CARTESIAN_POINT('Origin',(69.81,18.0787611019615,-68.));
#53968=CARTESIAN_POINT('',(69.81,91.,-69.5));
#53969=CARTESIAN_POINT('',(69.81,46.0787611019615,-36.5));
#53970=CARTESIAN_POINT('',(69.81,91.,-36.5));
#53971=CARTESIAN_POINT('',(69.81,46.0787611019615,-39.5));
#53972=CARTESIAN_POINT('Origin',(69.81,46.0787611019615,-38.));
#53973=CARTESIAN_POINT('',(69.81,91.,-39.5));
#53974=CARTESIAN_POINT('',(69.81,18.0787611019615,21.5));
#53975=CARTESIAN_POINT('',(69.81,91.,21.5));
#53976=CARTESIAN_POINT('',(69.81,18.0787611019615,24.5));
#53977=CARTESIAN_POINT('',(69.81,91.,24.5));
#53978=CARTESIAN_POINT('Origin',(69.81,18.0787611019615,23.));
#53979=CARTESIAN_POINT('',(69.81,46.0787611019615,16.5));
#53980=CARTESIAN_POINT('',(69.81,91.,16.5));
#53981=CARTESIAN_POINT('',(69.81,46.0787611019615,19.5));
#53982=CARTESIAN_POINT('',(69.81,91.,19.5));
#53983=CARTESIAN_POINT('Origin',(69.81,46.0787611019615,18.));
#53984=CARTESIAN_POINT('',(69.81,46.0787611019615,11.5));
#53985=CARTESIAN_POINT('',(69.81,91.,11.5));
#53986=CARTESIAN_POINT('',(69.81,46.0787611019615,14.5));
#53987=CARTESIAN_POINT('',(69.81,91.,14.5));
#53988=CARTESIAN_POINT('Origin',(69.81,46.0787611019615,13.));
#53989=CARTESIAN_POINT('',(69.81,18.0787611019615,11.5));
#53990=CARTESIAN_POINT('',(69.81,91.,11.5));
#53991=CARTESIAN_POINT('',(69.81,18.0787611019615,14.5));
#53992=CARTESIAN_POINT('',(69.81,91.,14.5));
#53993=CARTESIAN_POINT('Origin',(69.81,18.0787611019615,13.));
#53994=CARTESIAN_POINT('',(69.81,18.0787611019615,46.5));
#53995=CARTESIAN_POINT('',(69.81,91.,46.5));
#53996=CARTESIAN_POINT('',(69.81,18.0787611019615,49.5));
#53997=CARTESIAN_POINT('',(69.81,91.,49.5));
#53998=CARTESIAN_POINT('Origin',(69.81,18.0787611019615,48.));
#53999=CARTESIAN_POINT('',(69.81,46.0787611019615,41.5));
#54000=CARTESIAN_POINT('',(69.81,91.,41.5));
#54001=CARTESIAN_POINT('',(69.81,46.0787611019615,44.5));
#54002=CARTESIAN_POINT('',(69.81,91.,44.5));
#54003=CARTESIAN_POINT('Origin',(69.81,46.0787611019615,43.));
#54004=CARTESIAN_POINT('',(69.81,46.0787611019615,46.5));
#54005=CARTESIAN_POINT('',(69.81,91.,46.5));
#54006=CARTESIAN_POINT('',(69.81,46.0787611019615,49.5));
#54007=CARTESIAN_POINT('',(69.81,91.,49.5));
#54008=CARTESIAN_POINT('Origin',(69.81,46.0787611019615,48.));
#54009=CARTESIAN_POINT('',(69.81,46.0787611019615,51.5));
#54010=CARTESIAN_POINT('',(69.81,91.,51.5));
#54011=CARTESIAN_POINT('',(69.81,46.0787611019615,54.5));
#54012=CARTESIAN_POINT('',(69.81,91.,54.5));
#54013=CARTESIAN_POINT('Origin',(69.81,46.0787611019615,53.));
#54014=CARTESIAN_POINT('',(69.81,46.0787611019615,56.5));
#54015=CARTESIAN_POINT('',(69.81,91.,56.5));
#54016=CARTESIAN_POINT('',(69.81,46.0787611019615,59.5));
#54017=CARTESIAN_POINT('',(69.81,91.,59.5));
#54018=CARTESIAN_POINT('Origin',(69.81,46.0787611019615,58.));
#54019=CARTESIAN_POINT('',(69.81,46.0787611019615,61.5));
#54020=CARTESIAN_POINT('',(69.81,91.,61.5));
#54021=CARTESIAN_POINT('',(69.81,46.0787611019615,64.5));
#54022=CARTESIAN_POINT('',(69.81,91.,64.5));
#54023=CARTESIAN_POINT('Origin',(69.81,46.0787611019615,63.));
#54024=CARTESIAN_POINT('',(69.81,46.0787611019615,26.5));
#54025=CARTESIAN_POINT('',(69.81,91.,26.5));
#54026=CARTESIAN_POINT('',(69.81,46.0787611019615,29.5));
#54027=CARTESIAN_POINT('',(69.81,91.,29.5));
#54028=CARTESIAN_POINT('Origin',(69.81,46.0787611019615,28.));
#54029=CARTESIAN_POINT('',(69.81,46.0787611019615,31.5));
#54030=CARTESIAN_POINT('',(69.81,91.,31.5));
#54031=CARTESIAN_POINT('',(69.81,46.0787611019615,34.5));
#54032=CARTESIAN_POINT('',(69.81,91.,34.5));
#54033=CARTESIAN_POINT('Origin',(69.81,46.0787611019615,33.));
#54034=CARTESIAN_POINT('',(69.81,18.0787611019615,31.5));
#54035=CARTESIAN_POINT('',(69.81,91.,31.5));
#54036=CARTESIAN_POINT('',(69.81,18.0787611019615,34.5));
#54037=CARTESIAN_POINT('',(69.81,91.,34.5));
#54038=CARTESIAN_POINT('Origin',(69.81,18.0787611019615,33.));
#54039=CARTESIAN_POINT('',(69.81,18.0787611019615,56.5));
#54040=CARTESIAN_POINT('',(69.81,91.,56.5));
#54041=CARTESIAN_POINT('',(69.81,18.0787611019615,59.5));
#54042=CARTESIAN_POINT('',(69.81,91.,59.5));
#54043=CARTESIAN_POINT('Origin',(69.81,18.0787611019615,58.));
#54044=CARTESIAN_POINT('',(69.81,18.0787611019615,66.5));
#54045=CARTESIAN_POINT('',(69.81,91.,66.5));
#54046=CARTESIAN_POINT('',(69.81,18.0787611019615,69.5));
#54047=CARTESIAN_POINT('',(69.81,91.,69.5));
#54048=CARTESIAN_POINT('Origin',(69.81,18.0787611019615,68.));
#54049=CARTESIAN_POINT('',(69.81,46.0787611019615,36.5));
#54050=CARTESIAN_POINT('',(69.81,91.,36.5));
#54051=CARTESIAN_POINT('',(69.81,46.0787611019615,39.5));
#54052=CARTESIAN_POINT('',(69.81,91.,39.5));
#54053=CARTESIAN_POINT('Origin',(69.81,46.0787611019615,38.));
#54054=CARTESIAN_POINT('',(69.81,18.0787611019615,61.5));
#54055=CARTESIAN_POINT('',(69.81,91.,61.5));
#54056=CARTESIAN_POINT('',(69.81,18.0787611019615,64.5));
#54057=CARTESIAN_POINT('',(69.81,91.,64.5));
#54058=CARTESIAN_POINT('Origin',(69.81,18.0787611019615,63.));
#54059=CARTESIAN_POINT('',(69.81,18.0787611019615,36.5));
#54060=CARTESIAN_POINT('',(69.81,91.,36.5));
#54061=CARTESIAN_POINT('',(69.81,18.0787611019615,39.5));
#54062=CARTESIAN_POINT('',(69.81,91.,39.5));
#54063=CARTESIAN_POINT('Origin',(69.81,18.0787611019615,38.));
#54064=CARTESIAN_POINT('',(69.81,18.0787611019615,41.5));
#54065=CARTESIAN_POINT('',(69.81,91.,41.5));
#54066=CARTESIAN_POINT('',(69.81,18.0787611019615,44.5));
#54067=CARTESIAN_POINT('',(69.81,91.,44.5));
#54068=CARTESIAN_POINT('Origin',(69.81,18.0787611019615,43.));
#54069=CARTESIAN_POINT('',(69.81,18.0787611019615,51.5));
#54070=CARTESIAN_POINT('',(69.81,91.,51.5));
#54071=CARTESIAN_POINT('',(69.81,18.0787611019615,54.5));
#54072=CARTESIAN_POINT('',(69.81,91.,54.5));
#54073=CARTESIAN_POINT('Origin',(69.81,18.0787611019615,53.));
#54074=CARTESIAN_POINT('',(69.81,18.0787611019615,26.5));
#54075=CARTESIAN_POINT('',(69.81,91.,26.5));
#54076=CARTESIAN_POINT('',(69.81,18.0787611019615,29.5));
#54077=CARTESIAN_POINT('',(69.81,91.,29.5));
#54078=CARTESIAN_POINT('Origin',(69.81,18.0787611019615,28.));
#54079=CARTESIAN_POINT('',(69.81,46.0787611019615,21.5));
#54080=CARTESIAN_POINT('',(69.81,91.,21.5));
#54081=CARTESIAN_POINT('',(69.81,46.0787611019615,24.5));
#54082=CARTESIAN_POINT('',(69.81,91.,24.5));
#54083=CARTESIAN_POINT('Origin',(69.81,46.0787611019615,23.));
#54084=CARTESIAN_POINT('',(69.81,18.0787611019615,16.5));
#54085=CARTESIAN_POINT('',(69.81,91.,16.5));
#54086=CARTESIAN_POINT('',(69.81,18.0787611019615,19.5));
#54087=CARTESIAN_POINT('',(69.81,91.,19.5));
#54088=CARTESIAN_POINT('Origin',(69.81,18.0787611019615,18.));
#54089=CARTESIAN_POINT('',(69.81,46.0787611019615,66.5));
#54090=CARTESIAN_POINT('',(69.81,91.,66.5));
#54091=CARTESIAN_POINT('',(69.81,46.0787611019615,69.5));
#54092=CARTESIAN_POINT('',(69.81,91.,69.5));
#54093=CARTESIAN_POINT('Origin',(69.81,46.0787611019615,68.));
#54094=CARTESIAN_POINT('',(69.81,46.0787611019615,-31.5));
#54095=CARTESIAN_POINT('',(69.81,91.,-31.5));
#54096=CARTESIAN_POINT('',(69.81,46.0787611019615,-34.5));
#54097=CARTESIAN_POINT('Origin',(69.81,46.0787611019615,-33.));
#54098=CARTESIAN_POINT('',(69.81,91.,-34.5));
#54099=CARTESIAN_POINT('',(69.81,46.0787611019615,-61.5));
#54100=CARTESIAN_POINT('',(69.81,91.,-61.5));
#54101=CARTESIAN_POINT('',(69.81,46.0787611019615,-64.5));
#54102=CARTESIAN_POINT('Origin',(69.81,46.0787611019615,-63.));
#54103=CARTESIAN_POINT('',(69.81,91.,-64.5));
#54104=CARTESIAN_POINT('',(69.81,46.0787611019615,-51.5));
#54105=CARTESIAN_POINT('',(69.81,91.,-51.5));
#54106=CARTESIAN_POINT('',(69.81,46.0787611019615,-54.5));
#54107=CARTESIAN_POINT('Origin',(69.81,46.0787611019615,-53.));
#54108=CARTESIAN_POINT('',(69.81,91.,-54.5));
#54109=CARTESIAN_POINT('',(69.81,46.0787611019615,-41.5));
#54110=CARTESIAN_POINT('',(69.81,91.,-41.5));
#54111=CARTESIAN_POINT('',(69.81,46.0787611019615,-44.5));
#54112=CARTESIAN_POINT('Origin',(69.81,46.0787611019615,-43.));
#54113=CARTESIAN_POINT('',(69.81,91.,-44.5));
#54114=CARTESIAN_POINT('',(69.81,18.0787611019615,-41.5));
#54115=CARTESIAN_POINT('',(69.81,91.,-41.5));
#54116=CARTESIAN_POINT('',(69.81,18.0787611019615,-44.5));
#54117=CARTESIAN_POINT('Origin',(69.81,18.0787611019615,-43.));
#54118=CARTESIAN_POINT('',(69.81,91.,-44.5));
#54119=CARTESIAN_POINT('',(69.81,18.0787611019615,-46.5));
#54120=CARTESIAN_POINT('',(69.81,91.,-46.5));
#54121=CARTESIAN_POINT('',(69.81,18.0787611019615,-49.5));
#54122=CARTESIAN_POINT('Origin',(69.81,18.0787611019615,-48.));
#54123=CARTESIAN_POINT('',(69.81,91.,-49.5));
#54124=CARTESIAN_POINT('',(69.81,18.0787611019615,-51.5));
#54125=CARTESIAN_POINT('',(69.81,91.,-51.5));
#54126=CARTESIAN_POINT('',(69.81,18.0787611019615,-54.5));
#54127=CARTESIAN_POINT('Origin',(69.81,18.0787611019615,-53.));
#54128=CARTESIAN_POINT('',(69.81,91.,-54.5));
#54129=CARTESIAN_POINT('',(69.81,18.0787611019615,-11.5));
#54130=CARTESIAN_POINT('',(69.81,91.,-11.5));
#54131=CARTESIAN_POINT('',(69.81,18.0787611019615,-14.5));
#54132=CARTESIAN_POINT('Origin',(69.81,18.0787611019615,-13.));
#54133=CARTESIAN_POINT('',(69.81,91.,-14.5));
#54134=CARTESIAN_POINT('',(69.81,46.0787611019615,-16.5));
#54135=CARTESIAN_POINT('',(69.81,91.,-16.5));
#54136=CARTESIAN_POINT('',(69.81,46.0787611019615,-19.5));
#54137=CARTESIAN_POINT('Origin',(69.81,46.0787611019615,-18.));
#54138=CARTESIAN_POINT('',(69.81,91.,-19.5));
#54139=CARTESIAN_POINT('',(69.81,18.0787611019615,-26.5));
#54140=CARTESIAN_POINT('',(69.81,91.,-26.5));
#54141=CARTESIAN_POINT('',(69.81,18.0787611019615,-29.5));
#54142=CARTESIAN_POINT('Origin',(69.81,18.0787611019615,-28.));
#54143=CARTESIAN_POINT('',(69.81,91.,-29.5));
#54144=CARTESIAN_POINT('',(69.81,46.0787611019615,-66.5));
#54145=CARTESIAN_POINT('',(69.81,91.,-66.5));
#54146=CARTESIAN_POINT('',(69.81,46.0787611019615,-69.5));
#54147=CARTESIAN_POINT('Origin',(69.81,46.0787611019615,-68.));
#54148=CARTESIAN_POINT('',(69.81,91.,-69.5));
#54149=CARTESIAN_POINT('Origin',(913.61,45.8777992076386,-29.25));
#54150=CARTESIAN_POINT('',(-86.39,34.9805523949445,-10.3754148577966));
#54151=CARTESIAN_POINT('',(-86.39,45.8777992076382,-29.25));
#54152=CARTESIAN_POINT('',(-85.5900000000001,34.9805523949445,-10.3754148577966));
#54153=CARTESIAN_POINT('',(-85.5900000000001,45.8777992076382,-29.25));
#54154=CARTESIAN_POINT('',(-86.39,34.9805523949445,-10.3754148577966));
#54155=CARTESIAN_POINT('Origin',(913.61,45.8777992076386,-29.25));
#54156=CARTESIAN_POINT('',(-85.5900000000001,59.7971840033556,-53.3590816762843));
#54157=CARTESIAN_POINT('',(-85.5900000000001,45.8777992076382,-29.25));
#54158=CARTESIAN_POINT('',(-86.39,59.7971840033556,-53.3590816762843));
#54159=CARTESIAN_POINT('',(-86.3899999999996,59.7971840033556,-53.3590816762843));
#54160=CARTESIAN_POINT('',(-86.39,45.8777992076382,-29.25));
#54161=CARTESIAN_POINT('Origin',(913.61,43.2797229962853,-30.75));
#54162=CARTESIAN_POINT('',(-86.39,57.199123585184,-54.8591090308774));
#54163=CARTESIAN_POINT('',(-86.39,54.1769698089785,-49.6245851422034));
#54164=CARTESIAN_POINT('',(-86.39,43.2797229962849,-30.75));
#54165=CARTESIAN_POINT('',(-85.5900000000001,57.199123585184,-54.8591090308774));
#54166=CARTESIAN_POINT('',(-85.5899999999993,57.1991235851839,-54.8591090308774));
#54167=CARTESIAN_POINT('',(-85.5900000000001,54.1769698089785,-49.6245851422034));
#54168=CARTESIAN_POINT('',(-85.5900000000001,43.2797229962849,-30.75));
#54169=CARTESIAN_POINT('',(-86.39,54.1769698089785,-49.6245851422034));
#54170=CARTESIAN_POINT('Origin',(913.61,45.8777992076386,-30.75));
#54171=CARTESIAN_POINT('',(-85.5900000000001,34.9805523949445,-49.6245851422034));
#54172=CARTESIAN_POINT('',(-85.5900000000001,45.8777992076382,-30.75));
#54173=CARTESIAN_POINT('',(-86.39,34.9805523949445,-49.6245851422034));
#54174=CARTESIAN_POINT('',(-86.39,45.8777992076382,-30.75));
#54175=CARTESIAN_POINT('',(-85.5899999999994,34.9805523949445,-49.6245851422034));
#54176=CARTESIAN_POINT('Origin',(913.61,43.2797229962853,-29.25));
#54177=CARTESIAN_POINT('',(-86.39,29.3603382005674,-53.3590816762843));
#54178=CARTESIAN_POINT('',(-86.39,32.3825102482842,-48.1245261404244));
#54179=CARTESIAN_POINT('',(-86.39,43.2797229962849,-29.25));
#54180=CARTESIAN_POINT('',(-85.5900000000001,29.3603382005674,-53.3590816762843));
#54181=CARTESIAN_POINT('',(-85.5899999999992,29.3603382005674,-53.3590816762843));
#54182=CARTESIAN_POINT('',(-85.5900000000001,32.3825102482842,-48.1245261404244));
#54183=CARTESIAN_POINT('',(-85.5900000000001,43.2797229962849,-29.25));
#54184=CARTESIAN_POINT('',(-86.3900000000001,32.3825102482842,-48.1245261404244));
#54185=CARTESIAN_POINT('Origin',(913.61,4.00385864813601E-13,-31.5));
#54186=CARTESIAN_POINT('',(-85.5900000000001,22.7843241379305,-31.5));
#54187=CARTESIAN_POINT('',(-85.5900000000001,-3.75094692148686E-14,-31.5));
#54188=CARTESIAN_POINT('',(-86.39,22.7843241379305,-31.5));
#54189=CARTESIAN_POINT('',(-86.39,-3.78600659594871E-14,-31.5));
#54190=CARTESIAN_POINT('',(-85.5899999999993,22.7843241379305,-31.5));
#54191=CARTESIAN_POINT('Origin',(913.61,4.00385864813601E-13,-28.5));
#54192=CARTESIAN_POINT('',(-86.39,22.7843241379304,-28.5));
#54193=CARTESIAN_POINT('',(-86.39,-3.78600659594871E-14,-28.5));
#54194=CARTESIAN_POINT('',(-85.5900000000001,22.7843241379304,-28.5));
#54195=CARTESIAN_POINT('',(-85.5900000000001,-3.75094692148686E-14,-28.5));
#54196=CARTESIAN_POINT('',(-86.3899999999997,22.7843241379304,-28.5));
#54197=CARTESIAN_POINT('Origin',(913.61,43.2797229962853,-30.75));
#54198=CARTESIAN_POINT('',(-85.5900000000001,29.3603382005675,-6.64091832371568));
#54199=CARTESIAN_POINT('',(-85.5900000000001,32.3825102482842,-11.8754738595756));
#54200=CARTESIAN_POINT('',(-85.5900000000001,43.2797229962849,-30.75));
#54201=CARTESIAN_POINT('',(-86.39,29.3603382005675,-6.64091832371568));
#54202=CARTESIAN_POINT('',(-86.3899999999997,29.3603382005675,-6.64091832371568));
#54203=CARTESIAN_POINT('',(-86.39,32.3825102482842,-11.8754738595756));
#54204=CARTESIAN_POINT('',(-86.39,43.2797229962849,-30.75));
#54205=CARTESIAN_POINT('',(-85.5899999999993,32.3825102482842,-11.8754738595756));
#54206=CARTESIAN_POINT('Origin',(913.61,43.2797229962853,-29.25));
#54207=CARTESIAN_POINT('',(-85.5900000000001,57.199123585184,-5.14089096912262));
#54208=CARTESIAN_POINT('',(-85.5900000000001,54.1769698089785,-10.3754148577966));
#54209=CARTESIAN_POINT('',(-85.5900000000001,43.2797229962849,-29.25));
#54210=CARTESIAN_POINT('',(-86.39,57.199123585184,-5.14089096912262));
#54211=CARTESIAN_POINT('',(-86.3899999999997,57.199123585184,-5.14089096912262));
#54212=CARTESIAN_POINT('',(-86.39,54.1769698089785,-10.3754148577966));
#54213=CARTESIAN_POINT('',(-86.39,43.2797229962849,-29.25));
#54214=CARTESIAN_POINT('',(-85.5899999999995,54.1769698089785,-10.3754148577966));
#54215=CARTESIAN_POINT('Origin',(913.61,45.8777992076386,-30.75));
#54216=CARTESIAN_POINT('',(-86.39,59.7971840033556,-6.6409183237157));
#54217=CARTESIAN_POINT('',(-86.39,45.8777992076382,-30.75));
#54218=CARTESIAN_POINT('',(-85.5900000000001,59.7971840033556,-6.6409183237157));
#54219=CARTESIAN_POINT('',(-85.5899999999992,59.7971840033556,-6.64091832371569));
#54220=CARTESIAN_POINT('',(-85.5900000000001,45.8777992076382,-30.75));
#54221=CARTESIAN_POINT('Origin',(913.61,4.00385864813601E-13,-28.5));
#54222=CARTESIAN_POINT('',(-85.5900000000001,72.4174689786827,-28.5));
#54223=CARTESIAN_POINT('',(-85.5900000000001,66.3731980659926,-28.5));
#54224=CARTESIAN_POINT('',(-85.5900000000001,-3.75094692148686E-14,-28.5));
#54225=CARTESIAN_POINT('',(-86.39,72.4174689786827,-28.5));
#54226=CARTESIAN_POINT('',(-86.3899999999997,72.4174689786827,-28.5));
#54227=CARTESIAN_POINT('',(-86.39,66.3731980659926,-28.5));
#54228=CARTESIAN_POINT('',(-86.39,-3.78600659594871E-14,-28.5));
#54229=CARTESIAN_POINT('',(-85.5899999999993,66.3731980659926,-28.5));
#54230=CARTESIAN_POINT('Origin',(913.61,4.00385864813601E-13,-31.5));
#54231=CARTESIAN_POINT('',(-85.5900000000001,66.3731980659926,-31.5));
#54232=CARTESIAN_POINT('',(-85.5900000000001,72.4174689786827,-31.5));
#54233=CARTESIAN_POINT('',(-85.5900000000001,-3.75094692148686E-14,-31.5));
#54234=CARTESIAN_POINT('',(-86.39,66.3731980659926,-31.5));
#54235=CARTESIAN_POINT('',(-86.39,66.3731980659926,-31.5));
#54236=CARTESIAN_POINT('',(-86.39,72.4174689786827,-31.5));
#54237=CARTESIAN_POINT('',(-86.39,-3.78600659594871E-14,-31.5));
#54238=CARTESIAN_POINT('',(-85.5900000000001,72.4174689786827,-31.5));
#54239=CARTESIAN_POINT('Origin',(913.61,45.8777992076386,-29.25));
#54240=CARTESIAN_POINT('',(-86.39,28.9441343457475,0.0799678991386249));
#54241=CARTESIAN_POINT('',(-86.39,45.8777992076382,-29.25));
#54242=CARTESIAN_POINT('',(-85.59,28.9441343457475,0.0799678991386249));
#54243=CARTESIAN_POINT('',(-85.5900000000001,45.8777992076382,-29.25));
#54244=CARTESIAN_POINT('',(-86.3900000000001,28.9441343457475,0.0799678991386144));
#54245=CARTESIAN_POINT('Origin',(913.61,45.8777992076386,-29.25));
#54246=CARTESIAN_POINT('',(-85.5900000000001,65.0692781609549,-62.4906166195334));
#54247=CARTESIAN_POINT('',(-85.5900000000001,45.8777992076382,-29.25));
#54248=CARTESIAN_POINT('',(-86.39,65.0692781609549,-62.4906166195334));
#54249=CARTESIAN_POINT('',(913.61,65.0692781609553,-62.4906166195334));
#54250=CARTESIAN_POINT('',(-86.39,45.8777992076382,-29.25));
#54251=CARTESIAN_POINT('Origin',(913.61,43.2797229962853,-30.75));
#54252=CARTESIAN_POINT('',(-86.39,62.471318048616,-63.990817708925));
#54253=CARTESIAN_POINT('',(-86.39,60.2133878581756,-60.0799678991386));
#54254=CARTESIAN_POINT('',(-86.39,43.2797229962849,-30.75));
#54255=CARTESIAN_POINT('',(-85.5900000000001,62.471318048616,-63.990817708925));
#54256=CARTESIAN_POINT('',(913.61,62.4713180486164,-63.990817708925));
#54257=CARTESIAN_POINT('',(-85.5900000000001,60.2133878581756,-60.0799678991386));
#54258=CARTESIAN_POINT('',(-85.5900000000001,43.2797229962849,-30.75));
#54259=CARTESIAN_POINT('',(-86.39,60.2133878581756,-60.0799678991386));
#54260=CARTESIAN_POINT('Origin',(913.61,45.8777992076386,-30.75));
#54261=CARTESIAN_POINT('',(-85.59,28.9441343457474,-60.0799678991386));
#54262=CARTESIAN_POINT('',(-85.5900000000001,45.8777992076382,-30.75));
#54263=CARTESIAN_POINT('',(-86.39,28.9441343457474,-60.0799678991386));
#54264=CARTESIAN_POINT('',(-86.39,45.8777992076382,-30.75));
#54265=CARTESIAN_POINT('',(-85.5899999999991,28.9441343457474,-60.0799678991386));
#54266=CARTESIAN_POINT('Origin',(913.61,43.2797229962853,-29.25));
#54267=CARTESIAN_POINT('',(-86.39,24.0882440265733,-62.49061664793));
#54268=CARTESIAN_POINT('',(-86.39,26.3460395813141,-58.5800000340158));
#54269=CARTESIAN_POINT('',(-86.39,43.2797229962849,-29.25));
#54270=CARTESIAN_POINT('',(-85.59,24.0882440265733,-62.49061664793));
#54271=CARTESIAN_POINT('',(913.61,24.0882440265737,-62.49061664793));
#54272=CARTESIAN_POINT('',(-85.59,26.3460395813141,-58.5800000340159));
#54273=CARTESIAN_POINT('',(-85.5900000000001,43.2797229962849,-29.25));
#54274=CARTESIAN_POINT('',(-86.3899999999997,26.3460395813141,-58.5800000340158));
#54275=CARTESIAN_POINT('Origin',(913.61,4.00385864813601E-13,-31.5));
#54276=CARTESIAN_POINT('',(-85.5900000000001,10.7114976242099,-31.5));
#54277=CARTESIAN_POINT('',(-85.5900000000001,-3.75094692148686E-14,-31.5));
#54278=CARTESIAN_POINT('',(-86.39,10.7114976242099,-31.5));
#54279=CARTESIAN_POINT('',(-86.39,-3.78600659594871E-14,-31.5));
#54280=CARTESIAN_POINT('',(-85.5899999999991,10.7114976242099,-31.5));
#54281=CARTESIAN_POINT('Origin',(913.61,4.00385864813601E-13,-28.5));
#54282=CARTESIAN_POINT('',(-86.39,10.7114976242099,-28.5));
#54283=CARTESIAN_POINT('',(-86.39,-3.78600659594871E-14,-28.5));
#54284=CARTESIAN_POINT('',(-85.5900000000001,10.7114976242099,-28.5));
#54285=CARTESIAN_POINT('',(-85.5900000000001,-3.75094692148686E-14,-28.5));
#54286=CARTESIAN_POINT('',(-86.39,10.7114976242099,-28.5));
#54287=CARTESIAN_POINT('Origin',(913.61,43.2797229962853,-30.75));
#54288=CARTESIAN_POINT('',(-85.59,24.0882440453297,2.49061661544304));
#54289=CARTESIAN_POINT('',(-85.59,26.3460395813141,-1.41999996598413));
#54290=CARTESIAN_POINT('',(-85.5900000000001,43.2797229962849,-30.75));
#54291=CARTESIAN_POINT('',(-86.39,24.0882440453297,2.49061661544304));
#54292=CARTESIAN_POINT('',(913.61,24.0882440453301,2.49061661544304));
#54293=CARTESIAN_POINT('',(-86.39,26.3460395813141,-1.41999996598413));
#54294=CARTESIAN_POINT('',(-86.39,43.2797229962849,-30.75));
#54295=CARTESIAN_POINT('',(-85.5899999999992,26.3460395813141,-1.41999996598414));
#54296=CARTESIAN_POINT('Origin',(913.61,43.2797229962853,-29.25));
#54297=CARTESIAN_POINT('',(-85.5900000000001,62.4713181477978,3.99081788071295));
#54298=CARTESIAN_POINT('',(-85.5900000000001,60.2133878581756,0.0799678991385971));
#54299=CARTESIAN_POINT('',(-85.5900000000001,43.2797229962849,-29.25));
#54300=CARTESIAN_POINT('',(-86.39,62.4713181477978,3.99081788071295));
#54301=CARTESIAN_POINT('',(913.61,62.4713181477983,3.99081788071295));
#54302=CARTESIAN_POINT('',(-86.39,60.2133878581756,0.0799678991385971));
#54303=CARTESIAN_POINT('',(-86.39,43.2797229962849,-29.25));
#54304=CARTESIAN_POINT('',(-85.5899999999993,60.2133878581756,0.079967899138597));
#54305=CARTESIAN_POINT('Origin',(913.61,45.8777992076386,-30.75));
#54306=CARTESIAN_POINT('',(-86.39,65.0692781797092,2.49061665201677));
#54307=CARTESIAN_POINT('',(-86.39,45.8777992076382,-30.75));
#54308=CARTESIAN_POINT('',(-85.5900000000001,65.0692781797092,2.49061665201677));
#54309=CARTESIAN_POINT('',(913.61,65.0692781797097,2.49061665201678));
#54310=CARTESIAN_POINT('',(-85.5900000000001,45.8777992076382,-30.75));
#54311=CARTESIAN_POINT('Origin',(913.61,4.00385864813601E-13,-28.5));
#54312=CARTESIAN_POINT('',(-85.5900000000001,82.9621121574678,-28.5));
#54313=CARTESIAN_POINT('',(-85.5900000000001,78.4460245797131,-28.5));
#54314=CARTESIAN_POINT('',(-85.5900000000001,-3.75094692148686E-14,-28.5));
#54315=CARTESIAN_POINT('',(-86.39,82.9621121574678,-28.5));
#54316=CARTESIAN_POINT('',(913.61,82.9621121574682,-28.5));
#54317=CARTESIAN_POINT('',(-86.39,78.4460245797131,-28.5));
#54318=CARTESIAN_POINT('',(-86.39,-3.78600659594871E-14,-28.5));
#54319=CARTESIAN_POINT('',(-85.5899999999993,78.4460245797131,-28.5));
#54320=CARTESIAN_POINT('Origin',(913.61,4.00385864813601E-13,-31.5));
#54321=CARTESIAN_POINT('',(-85.5900000000001,78.4460245797131,-31.5));
#54322=CARTESIAN_POINT('',(-85.5900000000001,82.9621122252415,-31.5));
#54323=CARTESIAN_POINT('',(-85.5900000000001,-3.75094692148686E-14,-31.5));
#54324=CARTESIAN_POINT('',(-86.39,78.4460245797131,-31.5));
#54325=CARTESIAN_POINT('',(-86.39,78.4460245797131,-31.5));
#54326=CARTESIAN_POINT('',(-86.39,82.9621122252415,-31.5));
#54327=CARTESIAN_POINT('',(-86.39,-3.78600659594871E-14,-31.5));
#54328=CARTESIAN_POINT('',(913.61,82.962112225242,-31.5));
#54329=CARTESIAN_POINT('Ctrl Pts',(-85.5899999999994,67.2171660490139,2.97732764444334));
#54330=CARTESIAN_POINT('Ctrl Pts',(-86.5499999999997,67.2171660490139,2.97732764444334));
#54331=CARTESIAN_POINT('Ctrl Pts',(-85.5899999999994,68.1584024122484,2.33128481848304));
#54332=CARTESIAN_POINT('Ctrl Pts',(-86.5499999999997,68.1584024122484,2.33128481848304));
#54333=CARTESIAN_POINT('Ctrl Pts',(-85.5899999999996,70.1198842128573,0.858367843285162));
#54334=CARTESIAN_POINT('Ctrl Pts',(-86.5499999999999,70.1198842128573,0.858367843285162));
#54335=CARTESIAN_POINT('Ctrl Pts',(-85.5899999999993,72.908047301324,-1.67045379084889));
#54336=CARTESIAN_POINT('Ctrl Pts',(-86.5499999999996,72.908047301324,-1.67045379084889));
#54337=CARTESIAN_POINT('Ctrl Pts',(-85.5899999999995,75.549548273606,-4.58281161933925));
#54338=CARTESIAN_POINT('Ctrl Pts',(-86.5499999999998,75.549548273606,-4.58281161933925));
#54339=CARTESIAN_POINT('Ctrl Pts',(-85.5899999999994,77.890528302476,-7.7415676465901));
#54340=CARTESIAN_POINT('Ctrl Pts',(-86.5499999999997,77.890528302476,-7.7415676465901));
#54341=CARTESIAN_POINT('Ctrl Pts',(-85.5899999999993,79.9131007484785,-11.1132966089213));
#54342=CARTESIAN_POINT('Ctrl Pts',(-86.5499999999996,79.9131007484785,-11.1132966089213));
#54343=CARTESIAN_POINT('Ctrl Pts',(-85.5899999999992,81.5928567717819,-14.6680605730953));
#54344=CARTESIAN_POINT('Ctrl Pts',(-86.5499999999995,81.5928567717819,-14.6680605730953));
#54345=CARTESIAN_POINT('Ctrl Pts',(-85.5899999999995,82.9187743664602,-18.3695870184804));
#54346=CARTESIAN_POINT('Ctrl Pts',(-86.5499999999998,82.9187743664602,-18.3695870184804));
#54347=CARTESIAN_POINT('Ctrl Pts',(-85.5899999999994,83.8727543022822,-22.1837513334676));
#54348=CARTESIAN_POINT('Ctrl Pts',(-86.5499999999997,83.8727543022822,-22.1837513334676));
#54349=CARTESIAN_POINT('Ctrl Pts',(-85.5899999999993,84.2979204495417,-25.0429582798392));
#54350=CARTESIAN_POINT('Ctrl Pts',(-86.5499999999996,84.2979204495417,-25.0429582798392));
#54351=CARTESIAN_POINT('Ctrl Pts',(-85.5899999999994,84.4366282617325,-26.6149733080415));
#54352=CARTESIAN_POINT('Ctrl Pts',(-86.5499999999997,84.4366282617325,-26.6149733080415));
#54353=CARTESIAN_POINT('Ctrl Pts',(-85.5899999999994,84.4575664621194,-26.8833105716064));
#54354=CARTESIAN_POINT('Ctrl Pts',(-86.5499999999997,84.4575664621194,-26.8833105716064));
#54355=CARTESIAN_POINT('',(-85.5899999999998,84.45756646212,-26.8833105716133));
#54356=CARTESIAN_POINT('',(-85.5899999999998,67.2171660490092,2.97732764444655));
#54357=CARTESIAN_POINT('Ctrl Pts',(-85.5899999999998,84.45756646212,-26.8833105716133));
#54358=CARTESIAN_POINT('Ctrl Pts',(-85.5899999999998,84.4366282617329,-26.6149733080461));
#54359=CARTESIAN_POINT('Ctrl Pts',(-85.5899999999997,84.297920449542,-25.0429582798415));
#54360=CARTESIAN_POINT('Ctrl Pts',(-85.5899999999998,83.8727543022822,-22.1837513334676));
#54361=CARTESIAN_POINT('Ctrl Pts',(-85.59,82.9187743664602,-18.3695870184804));
#54362=CARTESIAN_POINT('Ctrl Pts',(-85.5899999999996,81.5928567717819,-14.6680605730953));
#54363=CARTESIAN_POINT('Ctrl Pts',(-85.5899999999997,79.9131007484785,-11.1132966089213));
#54364=CARTESIAN_POINT('Ctrl Pts',(-85.5899999999998,77.890528302476,-7.7415676465901));
#54365=CARTESIAN_POINT('Ctrl Pts',(-85.59,75.549548273606,-4.58281161933925));
#54366=CARTESIAN_POINT('Ctrl Pts',(-85.5899999999997,72.908047301324,-1.67045379084889));
#54367=CARTESIAN_POINT('Ctrl Pts',(-85.59,70.1198842128559,0.858367843286441));
#54368=CARTESIAN_POINT('Ctrl Pts',(-85.5899999999999,68.1584024122454,2.33128481848532));
#54369=CARTESIAN_POINT('Ctrl Pts',(-85.5899999999998,67.2171660490092,2.97732764444655));
#54370=CARTESIAN_POINT('',(-86.3899999999999,67.2171660490092,2.97732764444655));
#54371=CARTESIAN_POINT('',(-85.5899999999998,67.2171660490092,2.97732764444655));
#54372=CARTESIAN_POINT('',(-86.3899999999998,84.45756646212,-26.8833105716133));
#54373=CARTESIAN_POINT('Ctrl Pts',(-86.3899999999998,84.45756646212,-26.8833105716133));
#54374=CARTESIAN_POINT('Ctrl Pts',(-86.3899999999998,84.4366282617329,-26.6149733080461));
#54375=CARTESIAN_POINT('Ctrl Pts',(-86.3899999999998,84.297920449542,-25.0429582798415));
#54376=CARTESIAN_POINT('Ctrl Pts',(-86.3899999999999,83.8727543022822,-22.1837513334676));
#54377=CARTESIAN_POINT('Ctrl Pts',(-86.39,82.9187743664602,-18.3695870184804));
#54378=CARTESIAN_POINT('Ctrl Pts',(-86.3899999999996,81.5928567717819,-14.6680605730953));
#54379=CARTESIAN_POINT('Ctrl Pts',(-86.3899999999997,79.9131007484785,-11.1132966089213));
#54380=CARTESIAN_POINT('Ctrl Pts',(-86.3899999999999,77.890528302476,-7.7415676465901));
#54381=CARTESIAN_POINT('Ctrl Pts',(-86.39,75.549548273606,-4.58281161933925));
#54382=CARTESIAN_POINT('Ctrl Pts',(-86.3899999999997,72.908047301324,-1.67045379084889));
#54383=CARTESIAN_POINT('Ctrl Pts',(-86.3900000000001,70.1198842128559,0.858367843286441));
#54384=CARTESIAN_POINT('Ctrl Pts',(-86.3899999999999,68.1584024122454,2.33128481848532));
#54385=CARTESIAN_POINT('Ctrl Pts',(-86.3899999999999,67.2171660490092,2.97732764444655));
#54386=CARTESIAN_POINT('',(-86.39,84.45756646212,-26.8833105716133));
#54387=CARTESIAN_POINT('Origin',(-85.59,44.5787611019615,-30.));
#54388=CARTESIAN_POINT('Origin',(-85.59,55.9000854795073,-4.39089096912261));
#54389=CARTESIAN_POINT('',(-85.5900000000002,52.3121016227476,-11.0146003457498));
#54390=CARTESIAN_POINT('Origin',(-85.59,52.8779317033019,-9.62541485779658));
#54391=CARTESIAN_POINT('Ctrl Pts',(-85.5900000000002,52.3121016227476,-11.0146003457498));
#54392=CARTESIAN_POINT('Ctrl Pts',(-85.5900000000002,51.1067797000298,-10.5236598582919));
#54393=CARTESIAN_POINT('Ctrl Pts',(-85.59,48.5636521071369,-9.76033053440373));
#54394=CARTESIAN_POINT('Ctrl Pts',(-85.5900000000001,45.9204718342386,-9.5));
#54395=CARTESIAN_POINT('Ctrl Pts',(-85.5900000000001,44.5787611019615,-9.5));
#54396=CARTESIAN_POINT('Origin',(-85.59,36.2795905006212,-9.62541485779656));
#54397=CARTESIAN_POINT('Ctrl Pts',(-85.5900000000003,44.5787611019615,-0.5));
#54398=CARTESIAN_POINT('Ctrl Pts',(-85.5900000000003,42.6480066335628,-0.5));
#54399=CARTESIAN_POINT('Ctrl Pts',(-85.5899999999998,38.7864976967653,-0.880325434261422));
#54400=CARTESIAN_POINT('Ctrl Pts',(-85.59,34.8506764348827,-2.07424376132475));
#54401=CARTESIAN_POINT('Ctrl Pts',(-85.59,32.8626902557764,-2.92534739713371));
#54402=CARTESIAN_POINT('Ctrl Pts',(-85.59,32.6508629759237,-3.01900602947195));
#54403=CARTESIAN_POINT('',(-85.5900000000001,51.1378158375422,-15.6393839483491));
#54404=CARTESIAN_POINT('Origin',(-85.59,49.8387777318655,-14.8893839483491));
#54405=CARTESIAN_POINT('',(-85.5900000000001,47.7866618629516,-21.4437528963263));
#54406=CARTESIAN_POINT('',(-85.5900000000001,43.2797229962849,-29.25));
#54407=CARTESIAN_POINT('',(-85.5900000000003,46.1862026525626,-22.1631559443816));
#54408=CARTESIAN_POINT('Origin',(-85.59,46.487623757275,-20.6937528963263));
#54409=CARTESIAN_POINT('Ctrl Pts',(-85.5900000000003,46.1862026525626,-22.1631559443815));
#54410=CARTESIAN_POINT('Ctrl Pts',(-85.5900000000003,46.1706391043624,-22.1599633677104));
#54411=CARTESIAN_POINT('Ctrl Pts',(-85.5900000000003,46.1550660227809,-22.1568172778458));
#54412=CARTESIAN_POINT('Ctrl Pts',(-85.5900000000003,46.1394836780905,-22.1537177567742));
#54413=CARTESIAN_POINT('Ctrl Pts',(-85.5900000000004,45.6259499661778,-22.0515695504083));
#54414=CARTESIAN_POINT('Ctrl Pts',(-85.5900000000005,45.1023555340697,-22.));
#54415=CARTESIAN_POINT('Ctrl Pts',(-85.5900000000004,44.5787611019615,-22.));
#54416=CARTESIAN_POINT('',(-85.5900000000001,41.3708603409714,-21.4437528963263));
#54417=CARTESIAN_POINT('Origin',(-85.59,42.6698984466481,-20.6937528963263));
#54418=CARTESIAN_POINT('',(-85.5900000000001,45.8777992076382,-29.25));
#54419=CARTESIAN_POINT('Ctrl Pts',(-85.5899999999998,44.5787611019615,-12.5));
#54420=CARTESIAN_POINT('Ctrl Pts',(-85.5899999999998,43.433398281725,-12.5));
#54421=CARTESIAN_POINT('Ctrl Pts',(-85.5900000000001,41.4793849628696,-12.6924535139527));
#54422=CARTESIAN_POINT('Ctrl Pts',(-85.59,39.5894256076692,-13.2069280490151));
#54423=CARTESIAN_POINT('Ctrl Pts',(-85.59,38.8257009268133,-13.4727301224294));
#54424=CARTESIAN_POINT('',(-85.5900000000001,60.2949931567668,-28.5));
#54425=CARTESIAN_POINT('',(-85.5900000000001,53.5926110635042,-28.5));
#54426=CARTESIAN_POINT('',(-85.5900000000001,-3.75094692148686E-14,-28.5));
#54427=CARTESIAN_POINT('',(-85.5900000000001,52.1693515320421,-27.4736373149388));
#54428=CARTESIAN_POINT('Origin',(-85.59,53.5926110635042,-27.));
#54429=CARTESIAN_POINT('Ctrl Pts',(-85.5900000000001,52.1693515320421,-27.4736373149388));
#54430=CARTESIAN_POINT('Ctrl Pts',(-85.5900000000001,52.1092282262333,-27.2929693959288));
#54431=CARTESIAN_POINT('Ctrl Pts',(-85.5900000000001,51.8596181813086,-26.6235312275074));
#54432=CARTESIAN_POINT('Ctrl Pts',(-85.5900000000001,51.3485297861122,-25.6673520933024));
#54433=CARTESIAN_POINT('Ctrl Pts',(-85.5900000000002,50.8041422375675,-24.9624237973926));
#54434=CARTESIAN_POINT('Ctrl Pts',(-85.5900000000003,50.5618748736031,-24.689445144648));
#54435=CARTESIAN_POINT('',(-85.5900000000001,53.7358855886589,-17.139395137807));
#54436=CARTESIAN_POINT('',(-85.5900000000001,45.8777992076382,-30.75));
#54437=CARTESIAN_POINT('',(-85.5900000000001,56.0151454704897,-16.7539809977007));
#54438=CARTESIAN_POINT('Origin',(-85.59,55.0349236943356,-17.889395137807));
#54439=CARTESIAN_POINT('',(-85.5900000000001,61.7683968689589,-26.7187856673305));
#54440=CARTESIAN_POINT('Ctrl Pts',(-85.5900000000001,61.7683968689589,-26.7187856673305));
#54441=CARTESIAN_POINT('Ctrl Pts',(-85.5900000000001,61.7599375519114,-26.6744636407038));
#54442=CARTESIAN_POINT('Ctrl Pts',(-85.5900000000001,61.5322159292861,-25.5059524219445));
#54443=CARTESIAN_POINT('Ctrl Pts',(-85.5900000000002,60.8508742849282,-23.2598700311452));
#54444=CARTESIAN_POINT('Ctrl Pts',(-85.5900000000001,59.2232760668162,-20.2148479377946));
#54445=CARTESIAN_POINT('Ctrl Pts',(-85.59,57.4908812316918,-18.1039187234852));
#54446=CARTESIAN_POINT('Ctrl Pts',(-85.5900000000001,56.3382988733575,-17.0329646666021));
#54447=CARTESIAN_POINT('Ctrl Pts',(-85.5900000000001,56.0151454704897,-16.7539809977007));
#54448=CARTESIAN_POINT('Origin',(-85.59,60.2949931567668,-27.));
#54449=CARTESIAN_POINT('',(-85.5900000000001,53.7358855886589,-42.860604862193));
#54450=CARTESIAN_POINT('',(-85.5900000000001,45.8777992076382,-29.25));
#54451=CARTESIAN_POINT('',(-85.5900000000003,52.1693515320421,-32.5263626850612));
#54452=CARTESIAN_POINT('Ctrl Pts',(-85.5900000000003,50.5618748736031,-35.310554855352));
#54453=CARTESIAN_POINT('Ctrl Pts',(-85.5900000000003,50.8041422375675,-35.0375762026074));
#54454=CARTESIAN_POINT('Ctrl Pts',(-85.5900000000005,51.3485297861122,-34.3326479066976));
#54455=CARTESIAN_POINT('Ctrl Pts',(-85.5900000000003,51.8596181813085,-33.3764687724926));
#54456=CARTESIAN_POINT('Ctrl Pts',(-85.5900000000003,52.1092282262332,-32.7070306040712));
#54457=CARTESIAN_POINT('Ctrl Pts',(-85.5900000000003,52.1693515320421,-32.5263626850612));
#54458=CARTESIAN_POINT('',(-85.5900000000001,53.5926110635042,-31.5));
#54459=CARTESIAN_POINT('Origin',(-85.59,53.5926110635042,-32.9999999999999));
#54460=CARTESIAN_POINT('',(-85.5900000000001,60.2949931567668,-31.5));
#54461=CARTESIAN_POINT('',(-85.5900000000001,-3.75094692148686E-14,-31.5));
#54462=CARTESIAN_POINT('',(-85.5900000000002,61.7683968689589,-33.2812143326695));
#54463=CARTESIAN_POINT('Origin',(-85.59,60.2949931567668,-33.));
#54464=CARTESIAN_POINT('',(-85.5900000000001,56.0151454704896,-43.2460190022993));
#54465=CARTESIAN_POINT('Ctrl Pts',(-85.5900000000001,56.0151454704896,-43.2460190022993));
#54466=CARTESIAN_POINT('Ctrl Pts',(-85.5900000000001,56.3382988733575,-42.9670353333979));
#54467=CARTESIAN_POINT('Ctrl Pts',(-85.59,57.4908812316918,-41.8960812765148));
#54468=CARTESIAN_POINT('Ctrl Pts',(-85.59,59.2232760668162,-39.7851520622054));
#54469=CARTESIAN_POINT('Ctrl Pts',(-85.59,60.8508742849283,-36.7401299688548));
#54470=CARTESIAN_POINT('Ctrl Pts',(-85.5900000000002,61.5322159292861,-34.4940475780555));
#54471=CARTESIAN_POINT('Ctrl Pts',(-85.5900000000002,61.7599375519113,-33.3255363592962));
#54472=CARTESIAN_POINT('Ctrl Pts',(-85.5900000000002,61.7683968689589,-33.2812143326695));
#54473=CARTESIAN_POINT('Origin',(-85.59,55.0349236943356,-42.110604862193));
#54474=CARTESIAN_POINT('',(-85.5900000000001,41.3708603409714,-38.5562471036737));
#54475=CARTESIAN_POINT('',(-85.5900000000001,45.8777992076382,-30.75));
#54476=CARTESIAN_POINT('',(-85.5900000000002,42.9713195513605,-37.8368440556185));
#54477=CARTESIAN_POINT('Origin',(-85.59,42.6698984466481,-39.3062471036737));
#54478=CARTESIAN_POINT('',(-85.5900000000002,46.1862026525626,-37.8368440556185));
#54479=CARTESIAN_POINT('Ctrl Pts',(-85.5900000000002,42.9713195513605,-37.8368440556185));
#54480=CARTESIAN_POINT('Ctrl Pts',(-85.5900000000002,42.9868830995607,-37.8400366322896));
#54481=CARTESIAN_POINT('Ctrl Pts',(-85.5900000000001,43.5156846168748,-37.9468656555161));
#54482=CARTESIAN_POINT('Ctrl Pts',(-85.5900000000003,44.5787611019615,-38.0515695504083));
#54483=CARTESIAN_POINT('Ctrl Pts',(-85.5900000000001,45.6418375870482,-37.9468656555161));
#54484=CARTESIAN_POINT('Ctrl Pts',(-85.5900000000002,46.1706391043624,-37.8400366322896));
#54485=CARTESIAN_POINT('Ctrl Pts',(-85.5900000000002,46.1862026525626,-37.8368440556185));
#54486=CARTESIAN_POINT('',(-85.5900000000001,47.7866618629516,-38.5562471036737));
#54487=CARTESIAN_POINT('Origin',(-85.59,46.4876237572749,-39.3062471036737));
#54488=CARTESIAN_POINT('',(-85.5900000000001,51.1378158375422,-44.3606160516509));
#54489=CARTESIAN_POINT('',(-85.5900000000001,43.2797229962849,-30.75));
#54490=CARTESIAN_POINT('',(-85.59,50.3318212771098,-46.5272698775706));
#54491=CARTESIAN_POINT('Origin',(-85.59,49.8387777318655,-45.1106160516509));
#54492=CARTESIAN_POINT('Ctrl Pts',(-85.59,38.8257009268133,-46.5272698775706));
#54493=CARTESIAN_POINT('Ctrl Pts',(-85.5900000000001,39.5894256076692,-46.793071950985));
#54494=CARTESIAN_POINT('Ctrl Pts',(-85.5900000000001,41.4793849628696,-47.3075464860474));
#54495=CARTESIAN_POINT('Ctrl Pts',(-85.59,44.5787611019615,-47.6128083915182));
#54496=CARTESIAN_POINT('Ctrl Pts',(-85.5900000000002,47.6781372410534,-47.3075464860473));
#54497=CARTESIAN_POINT('Ctrl Pts',(-85.5900000000001,49.5680965962538,-46.793071950985));
#54498=CARTESIAN_POINT('Ctrl Pts',(-85.59,50.3318212771098,-46.5272698775706));
#54499=CARTESIAN_POINT('',(-85.5900000000001,35.5649111404189,-31.5));
#54500=CARTESIAN_POINT('',(-85.5900000000001,-3.75094692148686E-14,-31.5));
#54501=CARTESIAN_POINT('',(-85.5900000000004,36.988170671881,-32.5263626850613));
#54502=CARTESIAN_POINT('Origin',(-85.59,35.5649111404189,-33.));
#54503=CARTESIAN_POINT('',(-85.5900000000003,38.5956473303199,-35.3105548553519));
#54504=CARTESIAN_POINT('Ctrl Pts',(-85.5900000000004,36.988170671881,-32.5263626850613));
#54505=CARTESIAN_POINT('Ctrl Pts',(-85.5900000000004,37.0482939776898,-32.7070306040712));
#54506=CARTESIAN_POINT('Ctrl Pts',(-85.5900000000004,37.2979040226145,-33.3764687724926));
#54507=CARTESIAN_POINT('Ctrl Pts',(-85.5900000000002,37.8089924178108,-34.3326479066976));
#54508=CARTESIAN_POINT('Ctrl Pts',(-85.5900000000003,38.3533799663555,-35.0375762026073));
#54509=CARTESIAN_POINT('Ctrl Pts',(-85.5900000000003,38.5956473303199,-35.3105548553519));
#54510=CARTESIAN_POINT('',(-85.5900000000001,38.7727956517265,-37.0562271467965));
#54511=CARTESIAN_POINT('Origin',(-85.59,37.4737575460498,-36.3062271467965));
#54512=CARTESIAN_POINT('',(-85.5900000000001,35.4216366152641,-42.860604862193));
#54513=CARTESIAN_POINT('',(-85.5900000000001,43.2797229962849,-29.25));
#54514=CARTESIAN_POINT('',(-85.5900000000001,33.1423767334334,-43.2460190022993));
#54515=CARTESIAN_POINT('Origin',(-85.59,34.1225985095874,-42.110604862193));
#54516=CARTESIAN_POINT('Ctrl Pts',(-85.5900000000001,27.3891253349642,-33.2812143326694));
#54517=CARTESIAN_POINT('Ctrl Pts',(-85.5900000000001,27.3975846520117,-33.3255363592962));
#54518=CARTESIAN_POINT('Ctrl Pts',(-85.59,27.625306274637,-34.4940475780555));
#54519=CARTESIAN_POINT('Ctrl Pts',(-85.59,28.3066479189948,-36.7401299688549));
#54520=CARTESIAN_POINT('Ctrl Pts',(-85.59,29.9342461371069,-39.7851520622054));
#54521=CARTESIAN_POINT('Ctrl Pts',(-85.59,31.6666409722312,-41.8960812765148));
#54522=CARTESIAN_POINT('Ctrl Pts',(-85.5900000000001,32.8192233305655,-42.9670353333979));
#54523=CARTESIAN_POINT('Ctrl Pts',(-85.5900000000001,33.1423767334334,-43.2460190022993));
#54524=CARTESIAN_POINT('',(-85.5900000000001,35.4216366152641,-17.139395137807));
#54525=CARTESIAN_POINT('',(-85.5900000000001,38.7727956517265,-22.9437728532035));
#54526=CARTESIAN_POINT('',(-85.5900000000001,43.2797229962849,-30.75));
#54527=CARTESIAN_POINT('',(-85.5900000000003,38.5956473303199,-24.6894451446481));
#54528=CARTESIAN_POINT('Origin',(-85.59,37.4737575460499,-23.6937728532035));
#54529=CARTESIAN_POINT('',(-85.5900000000003,36.988170671881,-27.4736373149387));
#54530=CARTESIAN_POINT('Ctrl Pts',(-85.5900000000003,38.5956473303199,-24.6894451446481));
#54531=CARTESIAN_POINT('Ctrl Pts',(-85.5900000000003,38.3533799663555,-24.9624237973927));
#54532=CARTESIAN_POINT('Ctrl Pts',(-85.5900000000002,37.8089924178108,-25.6673520933024));
#54533=CARTESIAN_POINT('Ctrl Pts',(-85.5900000000004,37.2979040226145,-26.6235312275074));
#54534=CARTESIAN_POINT('Ctrl Pts',(-85.5900000000003,37.0482939776898,-27.2929693959288));
#54535=CARTESIAN_POINT('Ctrl Pts',(-85.5900000000003,36.988170671881,-27.4736373149387));
#54536=CARTESIAN_POINT('',(-85.5900000000001,35.5649111404189,-28.5));
#54537=CARTESIAN_POINT('Origin',(-85.59,35.5649111404189,-27.));
#54538=CARTESIAN_POINT('',(-85.5900000000001,-3.75094692148686E-14,-28.5));
#54539=CARTESIAN_POINT('',(-85.5900000000001,33.1423767334334,-16.7539809977007));
#54540=CARTESIAN_POINT('Ctrl Pts',(-85.5900000000001,33.1423767334334,-16.7539809977007));
#54541=CARTESIAN_POINT('Ctrl Pts',(-85.5900000000001,32.8192233305655,-17.0329646666021));
#54542=CARTESIAN_POINT('Ctrl Pts',(-85.5900000000001,31.6666409722312,-18.1039187234852));
#54543=CARTESIAN_POINT('Ctrl Pts',(-85.59,29.9342461371069,-20.2148479377946));
#54544=CARTESIAN_POINT('Ctrl Pts',(-85.5900000000004,28.3066479189948,-23.2598700311452));
#54545=CARTESIAN_POINT('Ctrl Pts',(-85.5900000000002,27.625306274637,-25.5059524219445));
#54546=CARTESIAN_POINT('Ctrl Pts',(-85.5900000000002,27.3975846520117,-26.6744636407038));
#54547=CARTESIAN_POINT('Ctrl Pts',(-85.5900000000002,27.3891253349642,-26.7187856673305));
#54548=CARTESIAN_POINT('Origin',(-85.59,34.1225985095875,-17.889395137807));
#54549=CARTESIAN_POINT('',(-85.59,64.8871997650542,-27.204472613345));
#54550=CARTESIAN_POINT('Origin',(-85.59,66.3731980659926,-27.));
#54551=CARTESIAN_POINT('Ctrl Pts',(-85.59,64.8871997650542,-27.204472613345));
#54552=CARTESIAN_POINT('Ctrl Pts',(-85.59,64.8317241956999,-26.8013056539391));
#54553=CARTESIAN_POINT('Ctrl Pts',(-85.59,64.5418111191102,-25.0760413061512));
#54554=CARTESIAN_POINT('Ctrl Pts',(-85.59,63.6403794020083,-22.1044191793415));
#54555=CARTESIAN_POINT('Ctrl Pts',(-85.5900000000001,61.7337643465056,-18.5373932985594));
#54556=CARTESIAN_POINT('Ctrl Pts',(-85.5900000000001,59.4786368856789,-15.7895125368918));
#54557=CARTESIAN_POINT('Ctrl Pts',(-85.5900000000001,57.8284952042271,-14.334111510217));
#54558=CARTESIAN_POINT('Ctrl Pts',(-85.5900000000001,57.1538693431447,-13.8100697594109));
#54559=CARTESIAN_POINT('',(-85.5900000000001,61.9811659354668,-6.17977241010521));
#54560=CARTESIAN_POINT('Origin',(-85.59,61.0962221090323,-7.39091832371568));
#54561=CARTESIAN_POINT('',(-85.59,73.9088368640223,-26.8393082747068));
#54562=CARTESIAN_POINT('Ctrl Pts',(-85.59,73.9088368640223,-26.8393082747068));
#54563=CARTESIAN_POINT('Ctrl Pts',(-85.59,73.81508077238,-25.9691649995929));
#54564=CARTESIAN_POINT('Ctrl Pts',(-85.5900000000001,73.3905329456488,-23.1927173488711));
#54565=CARTESIAN_POINT('Ctrl Pts',(-85.59,72.0088947532483,-18.6380666239304));
#54566=CARTESIAN_POINT('Ctrl Pts',(-85.59,69.2652291855737,-13.5050293808538));
#54567=CARTESIAN_POINT('Ctrl Pts',(-85.5900000000002,65.8355371052187,-9.32593748926008));
#54568=CARTESIAN_POINT('Ctrl Pts',(-85.5900000000001,63.2074283898593,-7.07576138749285));
#54569=CARTESIAN_POINT('Ctrl Pts',(-85.5900000000001,61.9811659354668,-6.17977241010521));
#54570=CARTESIAN_POINT('Origin',(-85.59,72.4174689786827,-27.));
#54571=CARTESIAN_POINT('',(-85.5900000000001,64.8871997650542,-32.795527386655));
#54572=CARTESIAN_POINT('Ctrl Pts',(-85.59,57.1538693431447,-46.1899302405891));
#54573=CARTESIAN_POINT('Ctrl Pts',(-85.59,57.8284952042271,-45.665888489783));
#54574=CARTESIAN_POINT('Ctrl Pts',(-85.5900000000001,59.4786368856789,-44.2104874631082));
#54575=CARTESIAN_POINT('Ctrl Pts',(-85.5900000000001,61.7337643465056,-41.4626067014406));
#54576=CARTESIAN_POINT('Ctrl Pts',(-85.59,63.6403794020083,-37.8955808206585));
#54577=CARTESIAN_POINT('Ctrl Pts',(-85.59,64.5418111191102,-34.9239586938488));
#54578=CARTESIAN_POINT('Ctrl Pts',(-85.5900000000001,64.8317241956999,-33.1986943460608));
#54579=CARTESIAN_POINT('Ctrl Pts',(-85.5900000000001,64.8871997650542,-32.795527386655));
#54580=CARTESIAN_POINT('Origin',(-85.59,66.3731980659926,-33.));
#54581=CARTESIAN_POINT('',(-85.5899999999999,73.9088368640223,-33.1606917252932));
#54582=CARTESIAN_POINT('Origin',(-85.59,72.4174689786827,-33.));
#54583=CARTESIAN_POINT('',(-85.5900000000001,61.9811659354668,-53.8202275898948));
#54584=CARTESIAN_POINT('Ctrl Pts',(-85.5900000000001,61.9811659354668,-53.8202275898948));
#54585=CARTESIAN_POINT('Ctrl Pts',(-85.5900000000001,63.2074283898592,-52.9242386125072));
#54586=CARTESIAN_POINT('Ctrl Pts',(-85.5900000000001,65.8355371052187,-50.6740625107399));
#54587=CARTESIAN_POINT('Ctrl Pts',(-85.5900000000001,69.2652291855737,-46.4949706191462));
#54588=CARTESIAN_POINT('Ctrl Pts',(-85.5900000000003,72.0088947532483,-41.3619333760696));
#54589=CARTESIAN_POINT('Ctrl Pts',(-85.59,73.3905329456488,-36.8072826511288));
#54590=CARTESIAN_POINT('Ctrl Pts',(-85.5899999999999,73.81508077238,-34.0308350004071));
#54591=CARTESIAN_POINT('Ctrl Pts',(-85.5899999999999,73.9088368640223,-33.1606917252932));
#54592=CARTESIAN_POINT('Origin',(-85.59,61.0962221090322,-52.6090816762843));
#54593=CARTESIAN_POINT('',(-85.59,36.8454205811755,-48.9853996542502));
#54594=CARTESIAN_POINT('Origin',(-85.59,36.2795905006212,-50.3745851422034));
#54595=CARTESIAN_POINT('',(-85.59,52.3121016227475,-48.9853996542502));
#54596=CARTESIAN_POINT('Ctrl Pts',(-85.59,36.8454205811755,-48.9853996542502));
#54597=CARTESIAN_POINT('Ctrl Pts',(-85.59,38.0507425038933,-49.4763401417081));
#54598=CARTESIAN_POINT('Ctrl Pts',(-85.5900000000002,40.5938700967861,-50.2396694655963));
#54599=CARTESIAN_POINT('Ctrl Pts',(-85.59,44.5787611019615,-50.6321469729213));
#54600=CARTESIAN_POINT('Ctrl Pts',(-85.5900000000001,48.563652107137,-50.2396694655963));
#54601=CARTESIAN_POINT('Ctrl Pts',(-85.5900000000001,51.1067797000298,-49.4763401417081));
#54602=CARTESIAN_POINT('Ctrl Pts',(-85.59,52.3121016227475,-48.9853996542502));
#54603=CARTESIAN_POINT('Origin',(-85.59,52.8779317033019,-50.3745851422034));
#54604=CARTESIAN_POINT('',(-85.5900000000001,56.5066592279994,-56.980993970528));
#54605=CARTESIAN_POINT('Origin',(-85.59,55.9000854795073,-55.6091090308774));
#54606=CARTESIAN_POINT('Ctrl Pts',(-85.59,32.6508629759236,-56.980993970528));
#54607=CARTESIAN_POINT('Ctrl Pts',(-85.59,32.8626902557763,-57.0746526028663));
#54608=CARTESIAN_POINT('Ctrl Pts',(-85.59,34.8506764348827,-57.9257562386752));
#54609=CARTESIAN_POINT('Ctrl Pts',(-85.5900000000003,38.7864976967653,-59.1196745657386));
#54610=CARTESIAN_POINT('Ctrl Pts',(-85.59,44.5787611019615,-59.6901627171307));
#54611=CARTESIAN_POINT('Ctrl Pts',(-85.5900000000001,50.3710245071578,-59.1196745657386));
#54612=CARTESIAN_POINT('Ctrl Pts',(-85.5900000000001,54.3068457690403,-57.9257562386753));
#54613=CARTESIAN_POINT('Ctrl Pts',(-85.5900000000001,56.2948319481467,-57.0746526028663));
#54614=CARTESIAN_POINT('Ctrl Pts',(-85.5900000000001,56.5066592279994,-56.980993970528));
#54615=CARTESIAN_POINT('',(-85.5900000000001,24.2703224388689,-32.7955273866549));
#54616=CARTESIAN_POINT('Origin',(-85.59,22.7843241379305,-33.));
#54617=CARTESIAN_POINT('',(-85.5900000000001,32.0036528607783,-46.189930240589));
#54618=CARTESIAN_POINT('Ctrl Pts',(-85.5900000000001,24.2703224388689,-32.7955273866549));
#54619=CARTESIAN_POINT('Ctrl Pts',(-85.5900000000001,24.3257980082232,-33.1986943460608));
#54620=CARTESIAN_POINT('Ctrl Pts',(-85.5900000000001,24.6157110848129,-34.9239586938488));
#54621=CARTESIAN_POINT('Ctrl Pts',(-85.5899999999997,25.5171428019148,-37.8955808206585));
#54622=CARTESIAN_POINT('Ctrl Pts',(-85.5900000000001,27.4237578574175,-41.4626067014406));
#54623=CARTESIAN_POINT('Ctrl Pts',(-85.5899999999999,29.6788853182442,-44.2104874631082));
#54624=CARTESIAN_POINT('Ctrl Pts',(-85.5900000000001,31.3290269996959,-45.665888489783));
#54625=CARTESIAN_POINT('Ctrl Pts',(-85.5900000000001,32.0036528607783,-46.189930240589));
#54626=CARTESIAN_POINT('Origin',(-85.59,31.0834721426076,-47.3745261404244));
#54627=CARTESIAN_POINT('',(-85.5900000000001,27.1763562684562,-53.8202275898948));
#54628=CARTESIAN_POINT('Origin',(-85.59,28.0613000948908,-52.6090816762843));
#54629=CARTESIAN_POINT('Ctrl Pts',(-85.59,15.2486853399007,-33.1606917252932));
#54630=CARTESIAN_POINT('Ctrl Pts',(-85.59,15.3424414315431,-34.0308350004071));
#54631=CARTESIAN_POINT('Ctrl Pts',(-85.59,15.7669892582742,-36.8072826511289));
#54632=CARTESIAN_POINT('Ctrl Pts',(-85.5900000000001,17.1486274506748,-41.3619333760696));
#54633=CARTESIAN_POINT('Ctrl Pts',(-85.59,19.8922930183494,-46.4949706191462));
#54634=CARTESIAN_POINT('Ctrl Pts',(-85.5900000000001,23.3219850987043,-50.6740625107399));
#54635=CARTESIAN_POINT('Ctrl Pts',(-85.5900000000001,25.9500938140638,-52.9242386125072));
#54636=CARTESIAN_POINT('Ctrl Pts',(-85.5900000000001,27.1763562684562,-53.8202275898948));
#54637=CARTESIAN_POINT('',(-85.59,32.0036528607784,-13.8100697594109));
#54638=CARTESIAN_POINT('Origin',(-85.59,31.0834721426076,-12.6254738595756));
#54639=CARTESIAN_POINT('',(-85.59,24.2703224388689,-27.2044726133451));
#54640=CARTESIAN_POINT('Ctrl Pts',(-85.59,32.0036528607784,-13.8100697594109));
#54641=CARTESIAN_POINT('Ctrl Pts',(-85.59,31.3290269996959,-14.334111510217));
#54642=CARTESIAN_POINT('Ctrl Pts',(-85.59,29.6788853182442,-15.7895125368918));
#54643=CARTESIAN_POINT('Ctrl Pts',(-85.59,27.4237578574175,-18.5373932985594));
#54644=CARTESIAN_POINT('Ctrl Pts',(-85.5900000000001,25.5171428019148,-22.1044191793415));
#54645=CARTESIAN_POINT('Ctrl Pts',(-85.59,24.6157110848129,-25.0760413061512));
#54646=CARTESIAN_POINT('Ctrl Pts',(-85.59,24.3257980082232,-26.8013056539392));
#54647=CARTESIAN_POINT('Ctrl Pts',(-85.59,24.2703224388689,-27.2044726133451));
#54648=CARTESIAN_POINT('Origin',(-85.59,22.7843241379304,-27.));
#54649=CARTESIAN_POINT('',(-85.5900000000001,27.1763562684563,-6.17977241010519));
#54650=CARTESIAN_POINT('Ctrl Pts',(-85.5900000000001,27.1763562684563,-6.17977241010519));
#54651=CARTESIAN_POINT('Ctrl Pts',(-85.5900000000001,25.9500938140638,-7.07576138749284));
#54652=CARTESIAN_POINT('Ctrl Pts',(-85.5900000000001,23.3219850987044,-9.32593748926008));
#54653=CARTESIAN_POINT('Ctrl Pts',(-85.5900000000001,19.8922930183494,-13.5050293808538));
#54654=CARTESIAN_POINT('Ctrl Pts',(-85.59,17.1486274506748,-18.6380666239304));
#54655=CARTESIAN_POINT('Ctrl Pts',(-85.59,15.7669892582742,-23.1927173488712));
#54656=CARTESIAN_POINT('Ctrl Pts',(-85.5900000000001,15.3424414315431,-25.9691649995929));
#54657=CARTESIAN_POINT('Ctrl Pts',(-85.59,15.2486853399007,-26.8393082747068));
#54658=CARTESIAN_POINT('Origin',(-85.59,28.0613000948908,-7.39091832371568));
#54659=CARTESIAN_POINT('',(-85.59,76.9518771315568,-27.1323759916595));
#54660=CARTESIAN_POINT('Origin',(-85.59,78.4460245797131,-27.));
#54661=CARTESIAN_POINT('Ctrl Pts',(-85.59,76.9518771315568,-27.1323759916595));
#54662=CARTESIAN_POINT('Ctrl Pts',(-85.59,76.8486238665202,-25.9669410775617));
#54663=CARTESIAN_POINT('Ctrl Pts',(-85.5900000000001,76.3805781139122,-22.6983584490168));
#54664=CARTESIAN_POINT('Ctrl Pts',(-85.5899999999998,74.7983998703283,-17.4826157721267));
#54665=CARTESIAN_POINT('Ctrl Pts',(-85.5900000000003,71.775717465263,-11.8275747416186));
#54666=CARTESIAN_POINT('Ctrl Pts',(-85.5900000000001,67.8660024791103,-7.06357324694729));
#54667=CARTESIAN_POINT('Ctrl Pts',(-85.5899999999999,64.7867667693647,-4.47726951084222));
#54668=CARTESIAN_POINT('Ctrl Pts',(-85.5899999999999,63.2487659305948,-3.39775347082817));
#54669=CARTESIAN_POINT('Origin',(-85.59,66.3683162853859,1.74061665201678));
#54670=CARTESIAN_POINT('Origin',(-85.59,82.9621121574678,-27.));
#54671=CARTESIAN_POINT('',(-85.5900000000001,76.9518771315568,-32.8676240083405));
#54672=CARTESIAN_POINT('Ctrl Pts',(-85.5900000000001,63.2487659305946,-56.6022465291719));
#54673=CARTESIAN_POINT('Ctrl Pts',(-85.5900000000001,64.7867667693646,-55.5227304891579));
#54674=CARTESIAN_POINT('Ctrl Pts',(-85.5900000000001,67.8660024791103,-52.9364267530528));
#54675=CARTESIAN_POINT('Ctrl Pts',(-85.59,71.7757174652631,-48.1724252583814));
#54676=CARTESIAN_POINT('Ctrl Pts',(-85.59,74.7983998703283,-42.5173842278733));
#54677=CARTESIAN_POINT('Ctrl Pts',(-85.5900000000002,76.3805781139122,-37.3016415509832));
#54678=CARTESIAN_POINT('Ctrl Pts',(-85.5900000000001,76.8486238665201,-34.0330589224383));
#54679=CARTESIAN_POINT('Ctrl Pts',(-85.5900000000001,76.9518771315568,-32.8676240083405));
#54680=CARTESIAN_POINT('Origin',(-85.59,78.4460245797131,-33.));
#54681=CARTESIAN_POINT('',(-85.5899999999998,84.4575665229983,-33.1166895167565));
#54682=CARTESIAN_POINT('Origin',(-85.59,82.9621122252415,-33.));
#54683=CARTESIAN_POINT('',(-85.5899999999999,67.2171661194344,-62.9773275507524));
#54684=CARTESIAN_POINT('Ctrl Pts',(-85.5899999999999,67.2171661194344,-62.9773275507524));
#54685=CARTESIAN_POINT('Ctrl Pts',(-85.59,68.1585542512634,-62.3311804544817));
#54686=CARTESIAN_POINT('Ctrl Pts',(-85.59,70.120027043277,-60.8582491474625));
#54687=CARTESIAN_POINT('Ctrl Pts',(-85.5899999999998,72.9083073089528,-58.329286199092));
#54688=CARTESIAN_POINT('Ctrl Pts',(-85.5899999999998,75.5496661779346,-55.41704471446));
#54689=CARTESIAN_POINT('Ctrl Pts',(-85.5900000000001,77.8907325893732,-52.2581266162731));
#54690=CARTESIAN_POINT('Ctrl Pts',(-85.5899999999996,79.9131883593013,-48.8865394828812));
#54691=CARTESIAN_POINT('Ctrl Pts',(-85.5899999999997,81.5929974870803,-45.3315997101041));
#54692=CARTESIAN_POINT('Ctrl Pts',(-85.59,82.9188283169055,-41.6302351306666));
#54693=CARTESIAN_POINT('Ctrl Pts',(-85.5899999999998,83.8728260383109,-37.8158880252114));
#54694=CARTESIAN_POINT('Ctrl Pts',(-85.5899999999997,84.2979456369875,-34.9568586727847));
#54695=CARTESIAN_POINT('Ctrl Pts',(-85.5899999999998,84.4366426410887,-33.3848430749953));
#54696=CARTESIAN_POINT('Ctrl Pts',(-85.5899999999998,84.4575665229983,-33.1166895167565));
#54697=CARTESIAN_POINT('Origin',(-85.59,66.3683162666315,-61.7406166195334));
#54698=CARTESIAN_POINT('',(-85.5899999999999,30.8757056257995,-59.4698569539159));
#54699=CARTESIAN_POINT('Origin',(-85.59,30.2431724514241,-60.8299678991386));
#54700=CARTESIAN_POINT('',(-85.5900000000001,58.2818165781235,-59.469856953916));
#54701=CARTESIAN_POINT('Ctrl Pts',(-85.5899999999999,30.8757056257995,-59.4698569539159));
#54702=CARTESIAN_POINT('Ctrl Pts',(-85.59,31.2936434644635,-59.6642231184655));
#54703=CARTESIAN_POINT('Ctrl Pts',(-85.59,33.6635280544172,-60.7056460155572));
#54704=CARTESIAN_POINT('Ctrl Pts',(-85.5900000000002,38.1974539606436,-62.0809974029323));
#54705=CARTESIAN_POINT('Ctrl Pts',(-85.5900000000001,44.5787611019615,-62.7095012985338));
#54706=CARTESIAN_POINT('Ctrl Pts',(-85.59,50.9600682432795,-62.0809974029323));
#54707=CARTESIAN_POINT('Ctrl Pts',(-85.5900000000001,55.4939941495058,-60.7056460155572));
#54708=CARTESIAN_POINT('Ctrl Pts',(-85.5900000000001,57.8638787394595,-59.6642231184655));
#54709=CARTESIAN_POINT('Ctrl Pts',(-85.5900000000001,58.2818165781235,-59.469856953916));
#54710=CARTESIAN_POINT('Origin',(-85.59,58.9143497524989,-60.8299678991386));
#54711=CARTESIAN_POINT('',(-85.5899999999997,61.8185254276963,-66.0944671367427));
#54712=CARTESIAN_POINT('Origin',(-85.59,61.1722799429393,-64.740817708925));
#54713=CARTESIAN_POINT('Ctrl Pts',(-85.5899999999997,27.338996733446,-66.0944672200995));
#54714=CARTESIAN_POINT('Ctrl Pts',(-85.5899999999998,27.9754117244437,-66.3982979628585));
#54715=CARTESIAN_POINT('Ctrl Pts',(-85.59,29.8161761061956,-67.2180577690146));
#54716=CARTESIAN_POINT('Ctrl Pts',(-85.5899999999995,32.9485259712089,-68.3400672149224));
#54717=CARTESIAN_POINT('Ctrl Pts',(-85.5900000000001,36.7628730766652,-69.2940649363253));
#54718=CARTESIAN_POINT('Ctrl Pts',(-85.5899999999996,40.6517737371936,-69.8723198908768));
#54719=CARTESIAN_POINT('Ctrl Pts',(-85.5900000000001,44.5789449552911,-70.0638446084523));
#54720=CARTESIAN_POINT('Ctrl Pts',(-85.5899999999997,48.5059334253501,-69.8723016740253));
#54721=CARTESIAN_POINT('Ctrl Pts',(-85.5900000000001,52.3950097685034,-69.2939932003241));
#54722=CARTESIAN_POINT('Ctrl Pts',(-85.5899999999998,56.2091740834478,-68.3400132644924));
#54723=CARTESIAN_POINT('Ctrl Pts',(-85.5899999999997,59.3415140239783,-67.2179830153801));
#54724=CARTESIAN_POINT('Ctrl Pts',(-85.5899999999997,61.1821104057502,-66.398297896696));
#54725=CARTESIAN_POINT('Ctrl Pts',(-85.5899999999997,61.8185254276963,-66.0944671367427));
#54726=CARTESIAN_POINT('',(-85.59,12.2056450723663,-32.8676240083405));
#54727=CARTESIAN_POINT('Origin',(-85.59,10.7114976242099,-33.));
#54728=CARTESIAN_POINT('',(-85.5899999999998,25.9087562733282,-56.6022465291718));
#54729=CARTESIAN_POINT('Ctrl Pts',(-85.59,12.2056450723663,-32.8676240083405));
#54730=CARTESIAN_POINT('Ctrl Pts',(-85.59,12.3088983374029,-34.0330589224383));
#54731=CARTESIAN_POINT('Ctrl Pts',(-85.59,12.7769440900109,-37.3016415509832));
#54732=CARTESIAN_POINT('Ctrl Pts',(-85.5900000000001,14.3591223335948,-42.5173842278733));
#54733=CARTESIAN_POINT('Ctrl Pts',(-85.5900000000002,17.38180473866,-48.1724252583814));
#54734=CARTESIAN_POINT('Ctrl Pts',(-85.5899999999998,21.2915197248128,-52.9364267530527));
#54735=CARTESIAN_POINT('Ctrl Pts',(-85.5899999999998,24.3707554345583,-55.5227304891578));
#54736=CARTESIAN_POINT('Ctrl Pts',(-85.5899999999998,25.9087562733282,-56.6022465291718));
#54737=CARTESIAN_POINT('Origin',(-85.59,25.0470014756374,-57.8300000340158));
#54738=CARTESIAN_POINT('',(-85.5899999999999,21.9403561483044,-62.9773276342038));
#54739=CARTESIAN_POINT('Origin',(-85.59,22.7892059208967,-61.7406166479301));
#54740=CARTESIAN_POINT('Ctrl Pts',(-85.5899999999999,4.69995574181559,-33.1166894283889));
#54741=CARTESIAN_POINT('Ctrl Pts',(-85.5899999999999,4.72089394220625,-33.3850266919971));
#54742=CARTESIAN_POINT('Ctrl Pts',(-85.5899999999999,4.85960175440013,-34.9570417202001));
#54743=CARTESIAN_POINT('Ctrl Pts',(-85.5899999999997,5.28476790164041,-37.8162486665527));
#54744=CARTESIAN_POINT('Ctrl Pts',(-85.5900000000001,6.23874783746636,-41.6304129814993));
#54745=CARTESIAN_POINT('Ctrl Pts',(-85.5899999999996,7.56466543214173,-45.3319394268853));
#54746=CARTESIAN_POINT('Ctrl Pts',(-85.59,9.2444214554221,-48.8867033911447));
#54747=CARTESIAN_POINT('Ctrl Pts',(-85.5899999999996,11.2669939014917,-52.2584323532902));
#54748=CARTESIAN_POINT('Ctrl Pts',(-85.59,13.6079739302738,-55.4171883812443));
#54749=CARTESIAN_POINT('Ctrl Pts',(-85.59,16.2494749028876,-58.3295462070146));
#54750=CARTESIAN_POINT('Ctrl Pts',(-85.59,19.0376379878578,-60.8583678488589));
#54751=CARTESIAN_POINT('Ctrl Pts',(-85.59,20.9991197888157,-62.3312848007728));
#54752=CARTESIAN_POINT('Ctrl Pts',(-85.5899999999999,21.9403561483044,-62.9773276342038));
#54753=CARTESIAN_POINT('',(-85.5900000000001,25.9087562733283,-3.39775347082815));
#54754=CARTESIAN_POINT('Origin',(-85.59,25.0470014756374,-2.16999996598413));
#54755=CARTESIAN_POINT('',(-85.59,12.2056450723663,-27.1323759916595));
#54756=CARTESIAN_POINT('Ctrl Pts',(-85.5900000000001,25.9087562733283,-3.39775347082815));
#54757=CARTESIAN_POINT('Ctrl Pts',(-85.5900000000001,24.3707554345584,-4.4772695108422));
#54758=CARTESIAN_POINT('Ctrl Pts',(-85.5900000000001,21.2915197248128,-7.06357324694729));
#54759=CARTESIAN_POINT('Ctrl Pts',(-85.59,17.38180473866,-11.8275747416186));
#54760=CARTESIAN_POINT('Ctrl Pts',(-85.5900000000001,14.3591223335948,-17.4826157721267));
#54761=CARTESIAN_POINT('Ctrl Pts',(-85.59,12.7769440900109,-22.6983584490168));
#54762=CARTESIAN_POINT('Ctrl Pts',(-85.59,12.3088983374029,-25.9669410775617));
#54763=CARTESIAN_POINT('Ctrl Pts',(-85.59,12.2056450723663,-27.1323759916595));
#54764=CARTESIAN_POINT('Origin',(-85.59,10.7114976242099,-27.));
#54765=CARTESIAN_POINT('',(-85.59,21.9403560778721,2.9773275404997));
#54766=CARTESIAN_POINT('Ctrl Pts',(-85.59,21.9403560778721,2.9773275404997));
#54767=CARTESIAN_POINT('Ctrl Pts',(-85.59,20.9989679497993,2.33118043675338));
#54768=CARTESIAN_POINT('Ctrl Pts',(-85.5899999999998,19.0374951574427,0.85824915302959));
#54769=CARTESIAN_POINT('Ctrl Pts',(-85.5899999999997,16.2492148952407,-1.67071380306776));
#54770=CARTESIAN_POINT('Ctrl Pts',(-85.5900000000001,13.607856025903,-4.58295528496318));
#54771=CARTESIAN_POINT('Ctrl Pts',(-85.59,11.2667896145647,-7.74187338388924));
#54772=CARTESIAN_POINT('Ctrl Pts',(-85.5899999999998,9.24433384462075,-11.1134605170863));
#54773=CARTESIAN_POINT('Ctrl Pts',(-85.59,7.56452471684338,-14.6684002899082));
#54774=CARTESIAN_POINT('Ctrl Pts',(-85.5899999999997,6.23869388701356,-18.3697648693255));
#54775=CARTESIAN_POINT('Ctrl Pts',(-85.59,5.284696165608,-22.1841119748295));
#54776=CARTESIAN_POINT('Ctrl Pts',(-85.59,4.85957656691687,-25.0431413272591));
#54777=CARTESIAN_POINT('Ctrl Pts',(-85.59,4.72087956281877,-26.6151569250498));
#54778=CARTESIAN_POINT('Ctrl Pts',(-85.59,4.69995568091292,-26.8833104832455));
#54779=CARTESIAN_POINT('Origin',(-85.59,22.789205939653,1.74061661544304));
#54780=CARTESIAN_POINT('Origin',(-85.59,61.1722800421212,4.74081788071294));
#54781=CARTESIAN_POINT('',(-85.59,58.2818165781235,-0.530143046084078));
#54782=CARTESIAN_POINT('Origin',(-85.59,58.914349752499,0.829967899138591));
#54783=CARTESIAN_POINT('Ctrl Pts',(-85.59,58.2818165781235,-0.530143046084078));
#54784=CARTESIAN_POINT('Ctrl Pts',(-85.5900000000001,57.8638787394595,-0.335776881534524));
#54785=CARTESIAN_POINT('Ctrl Pts',(-85.5900000000001,55.4939941495058,0.70564601555715));
#54786=CARTESIAN_POINT('Ctrl Pts',(-85.59,50.9600682432795,2.08099740293233));
#54787=CARTESIAN_POINT('Ctrl Pts',(-85.59,46.7058634824008,2.5));
#54788=CARTESIAN_POINT('Ctrl Pts',(-85.59,44.5787611019615,2.5));
#54789=CARTESIAN_POINT('Origin',(-85.59,30.2431724514241,0.829967899138609));
#54790=CARTESIAN_POINT('Ctrl Pts',(-85.5899999999999,44.5787611019615,10.));
#54791=CARTESIAN_POINT('Ctrl Pts',(-85.5899999999999,43.2696882485426,10.0000072420571));
#54792=CARTESIAN_POINT('Ctrl Pts',(-85.5899999999996,40.651632580144,9.87232797964218));
#54793=CARTESIAN_POINT('Ctrl Pts',(-85.5899999999998,36.7625581228083,9.29399863504675));
#54794=CARTESIAN_POINT('Ctrl Pts',(-85.5899999999998,32.9483479139013,8.34001481829751));
#54795=CARTESIAN_POINT('Ctrl Pts',(-85.5899999999998,29.8160082284385,7.21798291392161));
#54796=CARTESIAN_POINT('Ctrl Pts',(-85.5899999999998,27.9754118813548,6.39829778738203));
#54797=CARTESIAN_POINT('Ctrl Pts',(-85.5899999999998,27.3389968866617,6.09446707403308));
#54798=CARTESIAN_POINT('Ctrl Pts',(-85.5899999999998,27.3389968866527,6.0944670740288));
#54799=CARTESIAN_POINT('Ctrl Pts',(-86.5500000000004,27.3389968866527,6.0944670740288));
#54800=CARTESIAN_POINT('Ctrl Pts',(-85.5899999999998,27.9754118813487,6.39829778737934));
#54801=CARTESIAN_POINT('Ctrl Pts',(-86.5500000000004,27.9754118813487,6.39829778737934));
#54802=CARTESIAN_POINT('Ctrl Pts',(-85.5899999999998,29.8160082284354,7.21798291392049));
#54803=CARTESIAN_POINT('Ctrl Pts',(-86.5500000000004,29.8160082284354,7.21798291392049));
#54804=CARTESIAN_POINT('Ctrl Pts',(-85.5899999999998,32.9483479139013,8.34001481829751));
#54805=CARTESIAN_POINT('Ctrl Pts',(-86.5500000000004,32.9483479139013,8.34001481829751));
#54806=CARTESIAN_POINT('Ctrl Pts',(-85.5899999999998,36.7625581228083,9.29399863504675));
#54807=CARTESIAN_POINT('Ctrl Pts',(-86.5500000000004,36.7625581228083,9.29399863504675));
#54808=CARTESIAN_POINT('Ctrl Pts',(-85.5899999999996,40.651632580144,9.87232797964218));
#54809=CARTESIAN_POINT('Ctrl Pts',(-86.5500000000002,40.651632580144,9.87232797964218));
#54810=CARTESIAN_POINT('Ctrl Pts',(-85.59,43.2696882485426,10.0000072420571));
#54811=CARTESIAN_POINT('Ctrl Pts',(-86.5500000000005,43.2696882485426,10.0000072420571));
#54812=CARTESIAN_POINT('Ctrl Pts',(-85.5899999999998,44.5787611019615,10.));
#54813=CARTESIAN_POINT('Ctrl Pts',(-86.5500000000004,44.5787611019615,10.));
#54814=CARTESIAN_POINT('Ctrl Pts',(-86.3899999999999,44.5787611019615,10.));
#54815=CARTESIAN_POINT('Ctrl Pts',(-86.3899999999999,43.2696882485426,10.0000072420571));
#54816=CARTESIAN_POINT('Ctrl Pts',(-86.3899999999996,40.6516325801439,9.87232797964218));
#54817=CARTESIAN_POINT('Ctrl Pts',(-86.3899999999999,36.7625581228083,9.29399863504675));
#54818=CARTESIAN_POINT('Ctrl Pts',(-86.3899999999999,32.9483479139013,8.34001481829751));
#54819=CARTESIAN_POINT('Ctrl Pts',(-86.3899999999999,29.8160082284385,7.21798291392161));
#54820=CARTESIAN_POINT('Ctrl Pts',(-86.3899999999999,27.9754118813548,6.39829778738203));
#54821=CARTESIAN_POINT('Ctrl Pts',(-86.3899999999999,27.3389968866617,6.09446707403308));
#54822=CARTESIAN_POINT('Origin',(913.61,45.8777992076386,-29.25));
#54823=CARTESIAN_POINT('',(-86.39,41.3708603409714,-21.4437528963263));
#54824=CARTESIAN_POINT('',(-86.39,45.8777992076382,-29.25));
#54825=CARTESIAN_POINT('',(-86.3899999999997,41.3708603409714,-21.4437528963263));
#54826=CARTESIAN_POINT('Ctrl Pts',(-85.59,4.69995568091346,-26.8833104832386));
#54827=CARTESIAN_POINT('Ctrl Pts',(-86.5500000000002,4.69995568091346,-26.8833104832386));
#54828=CARTESIAN_POINT('Ctrl Pts',(-85.59,4.72087956281917,-26.6151569250452));
#54829=CARTESIAN_POINT('Ctrl Pts',(-86.5500000000002,4.72087956281917,-26.6151569250452));
#54830=CARTESIAN_POINT('Ctrl Pts',(-85.59,4.85957656691721,-25.0431413272568));
#54831=CARTESIAN_POINT('Ctrl Pts',(-86.5500000000003,4.85957656691721,-25.0431413272568));
#54832=CARTESIAN_POINT('Ctrl Pts',(-85.59,5.284696165608,-22.1841119748295));
#54833=CARTESIAN_POINT('Ctrl Pts',(-86.5500000000002,5.284696165608,-22.1841119748295));
#54834=CARTESIAN_POINT('Ctrl Pts',(-85.5899999999997,6.23869388701356,-18.3697648693255));
#54835=CARTESIAN_POINT('Ctrl Pts',(-86.55,6.23869388701356,-18.3697648693255));
#54836=CARTESIAN_POINT('Ctrl Pts',(-85.59,7.56452471684338,-14.6684002899082));
#54837=CARTESIAN_POINT('Ctrl Pts',(-86.5500000000002,7.56452471684338,-14.6684002899082));
#54838=CARTESIAN_POINT('Ctrl Pts',(-85.5899999999998,9.24433384462075,-11.1134605170863));
#54839=CARTESIAN_POINT('Ctrl Pts',(-86.5500000000001,9.24433384462075,-11.1134605170863));
#54840=CARTESIAN_POINT('Ctrl Pts',(-85.59,11.2667896145647,-7.74187338388924));
#54841=CARTESIAN_POINT('Ctrl Pts',(-86.5500000000002,11.2667896145647,-7.74187338388924));
#54842=CARTESIAN_POINT('Ctrl Pts',(-85.5900000000001,13.607856025903,-4.58295528496318));
#54843=CARTESIAN_POINT('Ctrl Pts',(-86.5500000000003,13.607856025903,-4.58295528496318));
#54844=CARTESIAN_POINT('Ctrl Pts',(-85.5899999999997,16.2492148952407,-1.67071380306776));
#54845=CARTESIAN_POINT('Ctrl Pts',(-86.55,16.2492148952407,-1.67071380306776));
#54846=CARTESIAN_POINT('Ctrl Pts',(-85.5899999999998,19.0374951574414,0.858249153028345));
#54847=CARTESIAN_POINT('Ctrl Pts',(-86.5500000000001,19.0374951574414,0.858249153028345));
#54848=CARTESIAN_POINT('Ctrl Pts',(-85.59,20.9989679497964,2.33118043675116));
#54849=CARTESIAN_POINT('Ctrl Pts',(-86.5500000000002,20.9989679497964,2.33118043675116));
#54850=CARTESIAN_POINT('Ctrl Pts',(-85.59,21.9403560778675,2.97732754049656));
#54851=CARTESIAN_POINT('Ctrl Pts',(-86.5500000000002,21.9403560778675,2.97732754049656));
#54852=CARTESIAN_POINT('',(-86.39,21.9403560778721,2.9773275404997));
#54853=CARTESIAN_POINT('Ctrl Pts',(-86.39,21.9403560778721,2.9773275404997));
#54854=CARTESIAN_POINT('Ctrl Pts',(-86.39,20.9989679497993,2.33118043675338));
#54855=CARTESIAN_POINT('Ctrl Pts',(-86.3899999999999,19.0374951574427,0.85824915302959));
#54856=CARTESIAN_POINT('Ctrl Pts',(-86.3899999999997,16.2492148952407,-1.67071380306776));
#54857=CARTESIAN_POINT('Ctrl Pts',(-86.3900000000001,13.607856025903,-4.58295528496318));
#54858=CARTESIAN_POINT('Ctrl Pts',(-86.39,11.2667896145647,-7.74187338388924));
#54859=CARTESIAN_POINT('Ctrl Pts',(-86.3899999999999,9.24433384462075,-11.1134605170863));
#54860=CARTESIAN_POINT('Ctrl Pts',(-86.39,7.56452471684338,-14.6684002899082));
#54861=CARTESIAN_POINT('Ctrl Pts',(-86.3899999999997,6.23869388701356,-18.3697648693255));
#54862=CARTESIAN_POINT('Ctrl Pts',(-86.39,5.284696165608,-22.1841119748295));
#54863=CARTESIAN_POINT('Ctrl Pts',(-86.39,4.85957656691687,-25.0431413272591));
#54864=CARTESIAN_POINT('Ctrl Pts',(-86.39,4.72087956281877,-26.6151569250498));
#54865=CARTESIAN_POINT('Ctrl Pts',(-86.39,4.69995568091292,-26.8833104832455));
#54866=CARTESIAN_POINT('',(-86.39,21.9403560778721,2.9773275404997));
#54867=CARTESIAN_POINT('Ctrl Pts',(-85.5899999999998,21.9403561482997,-62.9773276342005));
#54868=CARTESIAN_POINT('Ctrl Pts',(-86.55,21.9403561482997,-62.9773276342005));
#54869=CARTESIAN_POINT('Ctrl Pts',(-85.5899999999998,20.9991197888127,-62.3312848007705));
#54870=CARTESIAN_POINT('Ctrl Pts',(-86.55,20.9991197888127,-62.3312848007705));
#54871=CARTESIAN_POINT('Ctrl Pts',(-85.5899999999998,19.0376379878564,-60.8583678488576));
#54872=CARTESIAN_POINT('Ctrl Pts',(-86.55,19.0376379878564,-60.8583678488576));
#54873=CARTESIAN_POINT('Ctrl Pts',(-85.5899999999998,16.2494749028876,-58.3295462070146));
#54874=CARTESIAN_POINT('Ctrl Pts',(-86.55,16.2494749028876,-58.3295462070146));
#54875=CARTESIAN_POINT('Ctrl Pts',(-85.5899999999998,13.6079739302738,-55.4171883812443));
#54876=CARTESIAN_POINT('Ctrl Pts',(-86.55,13.6079739302738,-55.4171883812443));
#54877=CARTESIAN_POINT('Ctrl Pts',(-85.5899999999995,11.2669939014917,-52.2584323532902));
#54878=CARTESIAN_POINT('Ctrl Pts',(-86.5499999999997,11.2669939014917,-52.2584323532902));
#54879=CARTESIAN_POINT('Ctrl Pts',(-85.5899999999998,9.2444214554221,-48.8867033911447));
#54880=CARTESIAN_POINT('Ctrl Pts',(-86.55,9.2444214554221,-48.8867033911447));
#54881=CARTESIAN_POINT('Ctrl Pts',(-85.5899999999995,7.56466543214173,-45.3319394268853));
#54882=CARTESIAN_POINT('Ctrl Pts',(-86.5499999999997,7.56466543214173,-45.3319394268853));
#54883=CARTESIAN_POINT('Ctrl Pts',(-85.59,6.23874783746636,-41.6304129814993));
#54884=CARTESIAN_POINT('Ctrl Pts',(-86.5500000000002,6.23874783746636,-41.6304129814993));
#54885=CARTESIAN_POINT('Ctrl Pts',(-85.5899999999996,5.28476790164041,-37.8162486665527));
#54886=CARTESIAN_POINT('Ctrl Pts',(-86.5499999999998,5.28476790164041,-37.8162486665527));
#54887=CARTESIAN_POINT('Ctrl Pts',(-85.5899999999998,4.85960175440047,-34.9570417202024));
#54888=CARTESIAN_POINT('Ctrl Pts',(-86.55,4.85960175440047,-34.9570417202024));
#54889=CARTESIAN_POINT('Ctrl Pts',(-85.5899999999997,4.72089394220665,-33.3850266920016));
#54890=CARTESIAN_POINT('Ctrl Pts',(-86.55,4.72089394220665,-33.3850266920016));
#54891=CARTESIAN_POINT('Ctrl Pts',(-85.5899999999997,4.69995574181612,-33.1166894283958));
#54892=CARTESIAN_POINT('Ctrl Pts',(-86.55,4.69995574181612,-33.1166894283958));
#54893=CARTESIAN_POINT('',(-86.3899999999999,21.9403561483044,-62.9773276342038));
#54894=CARTESIAN_POINT('',(-85.5899999999997,21.9403561483044,-62.9773276342038));
#54895=CARTESIAN_POINT('Ctrl Pts',(-86.3899999999999,4.69995574181559,-33.1166894283889));
#54896=CARTESIAN_POINT('Ctrl Pts',(-86.3899999999999,4.72089394220625,-33.3850266919971));
#54897=CARTESIAN_POINT('Ctrl Pts',(-86.3899999999999,4.85960175440013,-34.9570417202001));
#54898=CARTESIAN_POINT('Ctrl Pts',(-86.3899999999997,5.28476790164041,-37.8162486665527));
#54899=CARTESIAN_POINT('Ctrl Pts',(-86.3900000000001,6.23874783746636,-41.6304129814993));
#54900=CARTESIAN_POINT('Ctrl Pts',(-86.3899999999996,7.56466543214173,-45.3319394268853));
#54901=CARTESIAN_POINT('Ctrl Pts',(-86.39,9.2444214554221,-48.8867033911447));
#54902=CARTESIAN_POINT('Ctrl Pts',(-86.3899999999996,11.2669939014917,-52.2584323532902));
#54903=CARTESIAN_POINT('Ctrl Pts',(-86.39,13.6079739302738,-55.4171883812443));
#54904=CARTESIAN_POINT('Ctrl Pts',(-86.39,16.2494749028876,-58.3295462070146));
#54905=CARTESIAN_POINT('Ctrl Pts',(-86.39,19.0376379878578,-60.8583678488589));
#54906=CARTESIAN_POINT('Ctrl Pts',(-86.39,20.9991197888157,-62.3312848007728));
#54907=CARTESIAN_POINT('Ctrl Pts',(-86.3899999999999,21.9403561483044,-62.9773276342038));
#54908=CARTESIAN_POINT('Ctrl Pts',(-85.5899999999997,61.8185254277052,-66.0944671367384));
#54909=CARTESIAN_POINT('Ctrl Pts',(-86.55,61.8185254277052,-66.0944671367384));
#54910=CARTESIAN_POINT('Ctrl Pts',(-85.5899999999997,61.1821104057562,-66.3982978966933));
#54911=CARTESIAN_POINT('Ctrl Pts',(-86.55,61.1821104057562,-66.3982978966933));
#54912=CARTESIAN_POINT('Ctrl Pts',(-85.5899999999997,59.3415140239815,-67.217983015379));
#54913=CARTESIAN_POINT('Ctrl Pts',(-86.55,59.3415140239815,-67.217983015379));
#54914=CARTESIAN_POINT('Ctrl Pts',(-85.5899999999998,56.2091740834478,-68.3400132644924));
#54915=CARTESIAN_POINT('Ctrl Pts',(-86.5500000000001,56.2091740834478,-68.3400132644924));
#54916=CARTESIAN_POINT('Ctrl Pts',(-85.5900000000001,52.3950097685034,-69.2939932003241));
#54917=CARTESIAN_POINT('Ctrl Pts',(-86.5500000000004,52.3950097685034,-69.2939932003241));
#54918=CARTESIAN_POINT('Ctrl Pts',(-85.5899999999997,48.5059334253501,-69.8723016740253));
#54919=CARTESIAN_POINT('Ctrl Pts',(-86.55,48.5059334253501,-69.8723016740253));
#54920=CARTESIAN_POINT('Ctrl Pts',(-85.5900000000001,44.5789449552911,-70.0638446084523));
#54921=CARTESIAN_POINT('Ctrl Pts',(-86.5500000000004,44.5789449552911,-70.0638446084523));
#54922=CARTESIAN_POINT('Ctrl Pts',(-85.5899999999996,40.6517737371936,-69.8723198908768));
#54923=CARTESIAN_POINT('Ctrl Pts',(-86.5499999999999,40.6517737371936,-69.8723198908768));
#54924=CARTESIAN_POINT('Ctrl Pts',(-85.5900000000001,36.7628730766652,-69.2940649363253));
#54925=CARTESIAN_POINT('Ctrl Pts',(-86.5500000000004,36.7628730766652,-69.2940649363253));
#54926=CARTESIAN_POINT('Ctrl Pts',(-85.5899999999995,32.9485259712089,-68.3400672149224));
#54927=CARTESIAN_POINT('Ctrl Pts',(-86.5499999999998,32.9485259712089,-68.3400672149224));
#54928=CARTESIAN_POINT('Ctrl Pts',(-85.59,29.8161761061925,-67.2180577690135));
#54929=CARTESIAN_POINT('Ctrl Pts',(-86.5500000000003,29.8161761061925,-67.2180577690135));
#54930=CARTESIAN_POINT('Ctrl Pts',(-85.5899999999998,27.9754117244376,-66.3982979628559));
#54931=CARTESIAN_POINT('Ctrl Pts',(-86.5500000000001,27.9754117244376,-66.3982979628559));
#54932=CARTESIAN_POINT('Ctrl Pts',(-85.5899999999998,27.3389967334371,-66.0944672200952));
#54933=CARTESIAN_POINT('Ctrl Pts',(-86.5500000000001,27.3389967334371,-66.0944672200952));
#54934=CARTESIAN_POINT('',(-86.3899999999997,61.8185254276963,-66.0944671367427));
#54935=CARTESIAN_POINT('',(-85.5899999999998,61.8185254276963,-66.0944671367427));
#54936=CARTESIAN_POINT('Ctrl Pts',(-86.3899999999998,27.338996733446,-66.0944672200995));
#54937=CARTESIAN_POINT('Ctrl Pts',(-86.3899999999998,27.9754117244437,-66.3982979628585));
#54938=CARTESIAN_POINT('Ctrl Pts',(-86.39,29.8161761061956,-67.2180577690146));
#54939=CARTESIAN_POINT('Ctrl Pts',(-86.3899999999995,32.9485259712089,-68.3400672149224));
#54940=CARTESIAN_POINT('Ctrl Pts',(-86.3900000000001,36.7628730766652,-69.2940649363253));
#54941=CARTESIAN_POINT('Ctrl Pts',(-86.3899999999996,40.6517737371936,-69.8723198908768));
#54942=CARTESIAN_POINT('Ctrl Pts',(-86.3900000000001,44.5789449552911,-70.0638446084523));
#54943=CARTESIAN_POINT('Ctrl Pts',(-86.3899999999997,48.50593342535,-69.8723016740253));
#54944=CARTESIAN_POINT('Ctrl Pts',(-86.3900000000001,52.3950097685034,-69.2939932003241));
#54945=CARTESIAN_POINT('Ctrl Pts',(-86.3899999999999,56.2091740834477,-68.3400132644924));
#54946=CARTESIAN_POINT('Ctrl Pts',(-86.3899999999998,59.3415140239783,-67.2179830153801));
#54947=CARTESIAN_POINT('Ctrl Pts',(-86.3899999999998,61.1821104057502,-66.398297896696));
#54948=CARTESIAN_POINT('Ctrl Pts',(-86.3899999999997,61.8185254276963,-66.0944671367427));
#54949=CARTESIAN_POINT('Origin',(-84.39,91.,80.));
#54950=CARTESIAN_POINT('',(-84.39,91.,75.));
#54951=CARTESIAN_POINT('',(-84.39,91.,-75.));
#54952=CARTESIAN_POINT('',(-84.39,91.,80.));
#54953=CARTESIAN_POINT('',(-84.39,86.,-80.));
#54954=CARTESIAN_POINT('',(-84.3900000000001,168.5,2.50000000000003));
#54955=CARTESIAN_POINT('',(-84.39,-1.84247779607695,-80.));
#54956=CARTESIAN_POINT('',(-84.39,91.,-80.));
#54957=CARTESIAN_POINT('',(-84.39,-1.84247779607695,-70.));
#54958=CARTESIAN_POINT('',(-84.39,-1.84247779607695,80.));
#54959=CARTESIAN_POINT('',(-84.39,-2.4,-68.8330657242578));
#54960=CARTESIAN_POINT('Origin',(-84.39,-3.34247779607695,-70.));
#54961=CARTESIAN_POINT('',(-84.39,-2.40000000000001,68.8330657242578));
#54962=CARTESIAN_POINT('',(-84.39,-2.40000000000001,80.));
#54963=CARTESIAN_POINT('',(-84.39,-1.84247779607695,70.));
#54964=CARTESIAN_POINT('Origin',(-84.39,-3.34247779607695,70.));
#54965=CARTESIAN_POINT('',(-84.39,-1.84247779607695,80.));
#54966=CARTESIAN_POINT('',(-84.39,-1.84247779607695,80.));
#54967=CARTESIAN_POINT('',(-84.39,86.,80.));
#54968=CARTESIAN_POINT('',(-84.39,91.,80.));
#54969=CARTESIAN_POINT('',(-84.39,88.5,77.5));
#54970=CARTESIAN_POINT('',(-84.39,64.417,65.));
#54971=CARTESIAN_POINT('',(-84.39,64.417,75.));
#54972=CARTESIAN_POINT('',(-84.39,64.417,65.));
#54973=CARTESIAN_POINT('',(-84.39,78.6669999999999,65.));
#54974=CARTESIAN_POINT('',(-84.39,64.6169999999999,65.));
#54975=CARTESIAN_POINT('',(-84.39,78.667,75.));
#54976=CARTESIAN_POINT('',(-84.39,78.667,75.));
#54977=CARTESIAN_POINT('',(-84.39,78.467,75.));
#54978=CARTESIAN_POINT('',(-84.39,76.,47.667));
#54979=CARTESIAN_POINT('',(-84.39,78.667,45.));
#54980=CARTESIAN_POINT('Origin',(-84.39,76.,45.));
#54981=CARTESIAN_POINT('',(-84.39,70.792807570849,47.667));
#54982=CARTESIAN_POINT('',(-84.39,70.792807570849,47.667));
#54983=CARTESIAN_POINT('',(-84.39,68.9069537854245,46.8858537854245));
#54984=CARTESIAN_POINT('Origin',(-84.39,70.792807570849,45.));
#54985=CARTESIAN_POINT('',(-84.39,66.0242462145755,44.0031462145755));
#54986=CARTESIAN_POINT('',(-84.39,66.0242462145755,44.0031462145755));
#54987=CARTESIAN_POINT('',(-84.39,65.2431,42.117292429151));
#54988=CARTESIAN_POINT('Origin',(-84.39,67.9101,42.117292429151));
#54989=CARTESIAN_POINT('',(-84.39,65.2431,34.547707570849));
#54990=CARTESIAN_POINT('',(-84.39,65.2431,34.547707570849));
#54991=CARTESIAN_POINT('',(-84.39,66.0242462145755,32.6618537854245));
#54992=CARTESIAN_POINT('Origin',(-84.39,67.9101,34.547707570849));
#54993=CARTESIAN_POINT('',(-84.39,68.9069537854245,29.7791462145755));
#54994=CARTESIAN_POINT('',(-84.39,68.9069537854245,29.7791462145755));
#54995=CARTESIAN_POINT('',(-84.39,70.792807570849,28.998));
#54996=CARTESIAN_POINT('Origin',(-84.39,70.792807570849,31.665));
#54997=CARTESIAN_POINT('',(-84.39,76.,28.998));
#54998=CARTESIAN_POINT('',(-84.39,76.,28.998));
#54999=CARTESIAN_POINT('',(-84.39,78.667,31.665));
#55000=CARTESIAN_POINT('Origin',(-84.39,76.,31.665));
#55001=CARTESIAN_POINT('',(-84.39,78.667,45.));
#55002=CARTESIAN_POINT('Origin',(-83.59,91.,80.));
#55003=CARTESIAN_POINT('',(-83.59,-1.84247779607695,-80.));
#55004=CARTESIAN_POINT('',(-83.59,86.,-80.));
#55005=CARTESIAN_POINT('',(-83.59,91.,-80.));
#55006=CARTESIAN_POINT('',(-83.59,91.,-75.));
#55007=CARTESIAN_POINT('',(-83.59,86.,-80.));
#55008=CARTESIAN_POINT('',(-83.59,91.,75.));
#55009=CARTESIAN_POINT('',(-83.59,91.,80.));
#55010=CARTESIAN_POINT('',(-83.59,86.,80.));
#55011=CARTESIAN_POINT('',(-83.59,91.,75.));
#55012=CARTESIAN_POINT('',(-83.59,-1.84247779607695,80.));
#55013=CARTESIAN_POINT('',(-83.59,91.,80.));
#55014=CARTESIAN_POINT('',(-83.59,-1.84247779607695,70.));
#55015=CARTESIAN_POINT('',(-83.59,-1.84247779607695,70.));
#55016=CARTESIAN_POINT('',(-83.59,-2.40000000000001,68.8330657242578));
#55017=CARTESIAN_POINT('Origin',(-83.59,-3.34247779607695,70.));
#55018=CARTESIAN_POINT('',(-83.59,-2.40000000000001,-68.8330657242578));
#55019=CARTESIAN_POINT('',(-83.59,-2.40000000000001,80.));
#55020=CARTESIAN_POINT('',(-83.59,-1.84247779607695,-70.));
#55021=CARTESIAN_POINT('Origin',(-83.59,-3.34247779607695,-70.));
#55022=CARTESIAN_POINT('',(-83.59,-1.84247779607695,-70.));
#55023=CARTESIAN_POINT('',(-83.59,78.6669999999999,65.));
#55024=CARTESIAN_POINT('',(-83.59,64.417,65.));
#55025=CARTESIAN_POINT('',(-83.59,91.,65.));
#55026=CARTESIAN_POINT('',(-83.59,64.417,75.));
#55027=CARTESIAN_POINT('',(-83.59,64.417,80.0000000000001));
#55028=CARTESIAN_POINT('',(-83.59,78.667,75.));
#55029=CARTESIAN_POINT('',(-83.59,91.,75.));
#55030=CARTESIAN_POINT('',(-83.59,78.667,80.0000000000001));
#55031=CARTESIAN_POINT('',(-83.59,70.792807570849,47.667));
#55032=CARTESIAN_POINT('',(-83.59,76.,47.667));
#55033=CARTESIAN_POINT('',(-83.59,91.,47.667));
#55034=CARTESIAN_POINT('',(-83.59,78.667,45.));
#55035=CARTESIAN_POINT('Origin',(-83.59,76.,45.));
#55036=CARTESIAN_POINT('',(-83.59,78.667,31.665));
#55037=CARTESIAN_POINT('',(-83.59,78.667,80.));
#55038=CARTESIAN_POINT('',(-83.59,76.,28.998));
#55039=CARTESIAN_POINT('Origin',(-83.59,76.,31.665));
#55040=CARTESIAN_POINT('',(-83.59,70.792807570849,28.998));
#55041=CARTESIAN_POINT('',(-83.59,91.0000000000001,28.998));
#55042=CARTESIAN_POINT('',(-83.59,68.9069537854245,29.7791462145755));
#55043=CARTESIAN_POINT('Origin',(-83.59,70.792807570849,31.665));
#55044=CARTESIAN_POINT('',(-83.59,66.0242462145755,32.6618537854245));
#55045=CARTESIAN_POINT('',(-83.59,54.8430500000001,43.8430499999998));
#55046=CARTESIAN_POINT('',(-83.59,65.2431,34.547707570849));
#55047=CARTESIAN_POINT('Origin',(-83.59,67.9101,34.547707570849));
#55048=CARTESIAN_POINT('',(-83.59,65.2431,42.117292429151));
#55049=CARTESIAN_POINT('',(-83.59,65.2431000000001,80.0000000000001));
#55050=CARTESIAN_POINT('',(-83.59,66.0242462145755,44.0031462145755));
#55051=CARTESIAN_POINT('Origin',(-83.59,67.9101,42.117292429151));
#55052=CARTESIAN_POINT('',(-83.59,68.9069537854245,46.8858537854245));
#55053=CARTESIAN_POINT('',(-83.59,96.5105500000001,74.4894499999998));
#55054=CARTESIAN_POINT('Origin',(-83.59,70.792807570849,45.));
#55055=CARTESIAN_POINT('Origin',(69.9524777960769,-13.2,70.));
#55056=CARTESIAN_POINT('',(69.01,-3.24056285356845,68.8330657242578));
#55057=CARTESIAN_POINT('',(69.01,-3.2,68.8330657242578));
#55058=CARTESIAN_POINT('',(68.4524777960769,-13.2,70.));
#55059=CARTESIAN_POINT('',(69.01,-3.2,68.8330657242578));
#55060=CARTESIAN_POINT('Origin',(68.4524777960769,-13.2,70.));
#55061=CARTESIAN_POINT('Origin',(69.9524777960769,-13.2,-70.));
#55062=CARTESIAN_POINT('',(69.01,-3.36366990003729,-68.8330657242578));
#55063=CARTESIAN_POINT('',(69.01,-4.,-68.8330657242578));
#55064=CARTESIAN_POINT('',(68.4524777960769,-13.2,-70.));
#55065=CARTESIAN_POINT('',(69.01,-4.,-68.8330657242578));
#55066=CARTESIAN_POINT('Origin',(68.4524777960769,-13.2,-70.));
#55067=CARTESIAN_POINT('Origin',(-83.7324777960769,-13.2,-70.));
#55068=CARTESIAN_POINT('',(-82.79,-3.24056285356836,-68.8330657242578));
#55069=CARTESIAN_POINT('',(-82.79,-3.2,-68.8330657242578));
#55070=CARTESIAN_POINT('',(-82.2324777960769,-13.2,-70.));
#55071=CARTESIAN_POINT('',(-82.79,-3.2,-68.8330657242578));
#55072=CARTESIAN_POINT('Origin',(-82.2324777960769,-13.2,-70.));
#55073=CARTESIAN_POINT('Origin',(-83.7324777960769,-13.2,70.));
#55074=CARTESIAN_POINT('',(-82.79,-3.36366990003701,68.8330657242578));
#55075=CARTESIAN_POINT('',(-82.79,-4.,68.8330657242578));
#55076=CARTESIAN_POINT('',(-82.2324777960769,-13.2,70.));
#55077=CARTESIAN_POINT('',(-82.79,-4.,68.8330657242578));
#55078=CARTESIAN_POINT('Origin',(-82.2324777960769,-13.2,70.));
#55079=CARTESIAN_POINT('Ctrl Pts',(-82.79,-4.,68.8330657242578));
#55080=CARTESIAN_POINT('Ctrl Pts',(-83.0279413156566,-4.,68.7173110465017));
#55081=CARTESIAN_POINT('Ctrl Pts',(-83.2497639817604,-3.94677923887688,
68.6312955463483));
#55082=CARTESIAN_POINT('Ctrl Pts',(-83.5368725214139,-3.81885822756997,
68.5460136539507));
#55083=CARTESIAN_POINT('Ctrl Pts',(-83.6251250918969,-3.76825636386172,
68.5249247721554));
#55084=CARTESIAN_POINT('Ctrl Pts',(-83.7454145055013,-3.6843570265968,68.5042990729681));
#55085=CARTESIAN_POINT('Ctrl Pts',(-83.783508253167,-3.65505504190423,68.4992584438234));
#55086=CARTESIAN_POINT('Ctrl Pts',(-83.8376288357695,-3.60955747043879,
68.4944494059826));
#55087=CARTESIAN_POINT('Ctrl Pts',(-83.8551663111009,-3.59413389138064,
68.4933050443484));
#55088=CARTESIAN_POINT('Ctrl Pts',(-83.8807216791802,-3.57066646564186,
68.4922764783663));
#55089=CARTESIAN_POINT('Ctrl Pts',(-83.8891150287393,-3.56278862689171,
68.4920482857838));
#55090=CARTESIAN_POINT('Ctrl Pts',(-83.9015180955293,-3.55089544816994,
68.4918779910273));
#55091=CARTESIAN_POINT('Ctrl Pts',(-83.9056212935433,-3.54691831714174,
68.4918498917946));
#55092=CARTESIAN_POINT('Ctrl Pts',(-83.9137655150753,-3.53893966650135,
68.4918510247018));
#55093=CARTESIAN_POINT('Ctrl Pts',(-83.918406027794,-3.53433818508778,68.4918889124519));
#55094=CARTESIAN_POINT('Ctrl Pts',(-84.0309533559687,-3.4217021285415,68.4935139055717));
#55095=CARTESIAN_POINT('Ctrl Pts',(-84.1449446474647,-3.27632522988999,
68.5227290784896));
#55096=CARTESIAN_POINT('Ctrl Pts',(-84.3247858753762,-2.89825016104428,
68.636438268353));
#55097=CARTESIAN_POINT('Ctrl Pts',(-84.39,-2.66511752285694,68.7205706579524));
#55098=CARTESIAN_POINT('Ctrl Pts',(-84.39,-2.4,68.8330657242578));
#55099=CARTESIAN_POINT('Ctrl Pts',(-82.79,-3.2,68.8330657242578));
#55100=CARTESIAN_POINT('Ctrl Pts',(-82.9088984009137,-3.2,68.7173813501885));
#55101=CARTESIAN_POINT('Ctrl Pts',(-83.0198819908802,-3.17338961943844,
68.6312955463483));
#55102=CARTESIAN_POINT('Ctrl Pts',(-83.163436260707,-3.10942911378499,68.5460136539507));
#55103=CARTESIAN_POINT('Ctrl Pts',(-83.2075625459484,-3.08412818193086,
68.5249247721554));
#55104=CARTESIAN_POINT('Ctrl Pts',(-83.2677072527507,-3.0421785132984,68.5042990729681));
#55105=CARTESIAN_POINT('Ctrl Pts',(-83.2867541265835,-3.02752752095212,
68.4992584438234));
#55106=CARTESIAN_POINT('Ctrl Pts',(-83.3138144178847,-3.0047787352194,68.4944494059826));
#55107=CARTESIAN_POINT('Ctrl Pts',(-83.3225831555504,-2.99706694569032,
68.4933050443484));
#55108=CARTESIAN_POINT('Ctrl Pts',(-83.3353608395901,-2.98533323282093,
68.4922764783663));
#55109=CARTESIAN_POINT('Ctrl Pts',(-83.3395575143696,-2.98139431344585,
68.4920482857838));
#55110=CARTESIAN_POINT('Ctrl Pts',(-83.3457590477646,-2.97544772408497,
68.4918779910273));
#55111=CARTESIAN_POINT('Ctrl Pts',(-83.3478106467717,-2.97345915857087,
68.4918498917946));
#55112=CARTESIAN_POINT('Ctrl Pts',(-83.3518827575376,-2.96946983325068,
68.4918510247018));
#55113=CARTESIAN_POINT('Ctrl Pts',(-83.354203013897,-2.96716909254389,68.4918889124519));
#55114=CARTESIAN_POINT('Ctrl Pts',(-83.4104766779843,-2.91085106427075,
68.4935139055717));
#55115=CARTESIAN_POINT('Ctrl Pts',(-83.4674723237323,-2.838162614945,68.5227290784896));
#55116=CARTESIAN_POINT('Ctrl Pts',(-83.5573929376881,-2.64912508052214,
68.636438268353));
#55117=CARTESIAN_POINT('Ctrl Pts',(-83.59,-2.53242495718233,68.7206842099906));
#55118=CARTESIAN_POINT('Ctrl Pts',(-83.59,-2.4,68.8330657242578));
#55119=CARTESIAN_POINT('Ctrl Pts',(-82.79,-3.2,68.8330657242578));
#55120=CARTESIAN_POINT('Ctrl Pts',(-82.9088984009137,-3.2,68.7173813501885));
#55121=CARTESIAN_POINT('Ctrl Pts',(-83.0198819908802,-3.17338961943844,
68.6312955463483));
#55122=CARTESIAN_POINT('Ctrl Pts',(-83.163436260707,-3.10942911378499,68.5460136539507));
#55123=CARTESIAN_POINT('Ctrl Pts',(-83.2075625459484,-3.08412818193086,
68.5249247721554));
#55124=CARTESIAN_POINT('Ctrl Pts',(-83.2677072527507,-3.0421785132984,68.5042990729681));
#55125=CARTESIAN_POINT('Ctrl Pts',(-83.2867541265835,-3.02752752095212,
68.4992584438234));
#55126=CARTESIAN_POINT('Ctrl Pts',(-83.3138144178847,-3.0047787352194,68.4944494059826));
#55127=CARTESIAN_POINT('Ctrl Pts',(-83.3225831555504,-2.99706694569032,
68.4933050443484));
#55128=CARTESIAN_POINT('Ctrl Pts',(-83.3353608395901,-2.98533323282093,
68.4922764783663));
#55129=CARTESIAN_POINT('Ctrl Pts',(-83.3395575143696,-2.98139431344585,
68.4920482857838));
#55130=CARTESIAN_POINT('Ctrl Pts',(-83.3457590477646,-2.97544772408497,
68.4918779910273));
#55131=CARTESIAN_POINT('Ctrl Pts',(-83.3478106467717,-2.97345915857087,
68.4918498917946));
#55132=CARTESIAN_POINT('Ctrl Pts',(-83.3518827575376,-2.96946983325068,
68.4918510247018));
#55133=CARTESIAN_POINT('Ctrl Pts',(-83.354203013897,-2.96716909254389,68.4918889124519));
#55134=CARTESIAN_POINT('Ctrl Pts',(-83.4104766779843,-2.91085106427075,
68.4935139055717));
#55135=CARTESIAN_POINT('Ctrl Pts',(-83.4674723237323,-2.838162614945,68.5227290784896));
#55136=CARTESIAN_POINT('Ctrl Pts',(-83.5573929376881,-2.64912508052214,
68.636438268353));
#55137=CARTESIAN_POINT('Ctrl Pts',(-83.59,-2.53242495718233,68.7206842099906));
#55138=CARTESIAN_POINT('Ctrl Pts',(-83.59,-2.40000000000001,68.8330657242578));
#55139=CARTESIAN_POINT('',(-83.6305628535685,-2.40000000000001,68.8330657242578));
#55140=CARTESIAN_POINT('',(-83.59,-2.40000000000001,68.8330657242578));
#55141=CARTESIAN_POINT('',(-83.59,-2.40000000000001,68.8330657242578));
#55142=CARTESIAN_POINT('Ctrl Pts',(-82.79,-4.,68.8330657242578));
#55143=CARTESIAN_POINT('Ctrl Pts',(-82.8781350353569,-4.,68.7901894268455));
#55144=CARTESIAN_POINT('Ctrl Pts',(-82.9641672156171,-3.99269386732363,
68.7513422007487));
#55145=CARTESIAN_POINT('Ctrl Pts',(-83.047294945123,-3.97912863028611,68.7165431137518));
#55146=CARTESIAN_POINT('Ctrl Pts',(-83.1352801201528,-3.9647707287512,68.6797105937432));
#55147=CARTESIAN_POINT('Ctrl Pts',(-83.2200105423739,-3.94340160709907,
68.6474133539507));
#55148=CARTESIAN_POINT('Ctrl Pts',(-83.3005498664581,-3.91631302891331,
68.6196465072808));
#55149=CARTESIAN_POINT('Ctrl Pts',(-83.3490063626748,-3.90001518185163,
68.6029405798855));
#55150=CARTESIAN_POINT('Ctrl Pts',(-83.3959460898563,-3.88164790169975,
68.5878740346506));
#55151=CARTESIAN_POINT('Ctrl Pts',(-83.4411696748627,-3.86149856467227,
68.5744409514166));
#55152=CARTESIAN_POINT('Ctrl Pts',(-83.5368725214139,-3.81885822756997,
68.5460136539507));
#55153=CARTESIAN_POINT('Ctrl Pts',(-83.6251250918968,-3.76825636386172,
68.5249247721554));
#55154=CARTESIAN_POINT('Ctrl Pts',(-83.7053180342998,-3.71232347235178,
68.5111743060306));
#55155=CARTESIAN_POINT('Ctrl Pts',(-83.7454145055013,-3.6843570265968,68.5042990729681));
#55156=CARTESIAN_POINT('Ctrl Pts',(-83.783508253167,-3.65505504190423,68.4992584438234));
#55157=CARTESIAN_POINT('Ctrl Pts',(-83.8195886415687,-3.62472332759394,
68.4960524185962));
#55158=CARTESIAN_POINT('Ctrl Pts',(-83.8376288312364,-3.60955747424959,
68.4944494063854));
#55159=CARTESIAN_POINT('Ctrl Pts',(-83.8551663023162,-3.59413389910499,
68.4933050446952));
#55160=CARTESIAN_POINT('Ctrl Pts',(-83.8722032230969,-3.57848894082617,
68.4926193336937));
#55161=CARTESIAN_POINT('Ctrl Pts',(-83.8807216899086,-3.57066645578996,
68.4922764779345));
#55162=CARTESIAN_POINT('Ctrl Pts',(-83.8891150245838,-3.56278863087633,
68.4920482858408));
#55163=CARTESIAN_POINT('Ctrl Pts',(-83.8973837399326,-3.5548598410772,68.4919347559461));
#55164=CARTESIAN_POINT('Ctrl Pts',(-83.9015180955293,-3.55089544816994,
68.4918779910273));
#55165=CARTESIAN_POINT('Ctrl Pts',(-83.9056212935433,-3.54691831714174,
68.4918498917946));
#55166=CARTESIAN_POINT('Ctrl Pts',(-83.9096934043093,-3.54292899182155,
68.4918504582482));
#55167=CARTESIAN_POINT('Ctrl Pts',(-83.9137655150753,-3.53893966650135,
68.4918510247018));
#55168=CARTESIAN_POINT('Ctrl Pts',(-83.918406027794,-3.53433818508778,68.4918889124519));
#55169=CARTESIAN_POINT('Ctrl Pts',(-83.9218165528902,-3.53092497125305,
68.4919381546676));
#55170=CARTESIAN_POINT('Ctrl Pts',(-84.0309533559686,-3.42170212854153,
68.4935139055717));
#55171=CARTESIAN_POINT('Ctrl Pts',(-84.1449446474647,-3.27632522988999,
68.5227290784896));
#55172=CARTESIAN_POINT('Ctrl Pts',(-84.2348652614204,-3.08728769546713,
68.5795836734213));
#55173=CARTESIAN_POINT('Ctrl Pts',(-84.2643083303775,-3.02539037385596,
68.5981998025318));
#55174=CARTESIAN_POINT('Ctrl Pts',(-84.2911322238605,-2.95869691731586,
68.6197620638144));
#55175=CARTESIAN_POINT('Ctrl Pts',(-84.3138741189653,-2.88768751153503,
68.6442957957497));
#55176=CARTESIAN_POINT('Ctrl Pts',(-84.3355816359095,-2.81990785323989,
68.6677136507366));
#55177=CARTESIAN_POINT('Ctrl Pts',(-84.3535685888622,-2.7481966656002,68.6938386980911));
#55178=CARTESIAN_POINT('Ctrl Pts',(-84.3665908505951,-2.67300199653487,
68.7226721477159));
#55179=CARTESIAN_POINT('Ctrl Pts',(-84.3786851920698,-2.603165433317,68.7494510278218));
#55180=CARTESIAN_POINT('Ctrl Pts',(-84.3864964753952,-2.5303247318545,68.7785659004214));
#55181=CARTESIAN_POINT('Ctrl Pts',(-84.3890669981752,-2.45485641144071,
68.8100015749531));
#55182=CARTESIAN_POINT('Ctrl Pts',(-84.3896847131035,-2.43672083664923,
68.8175557913908));
#55183=CARTESIAN_POINT('Ctrl Pts',(-84.39,-2.41843358706486,68.8252439568516));
#55184=CARTESIAN_POINT('Ctrl Pts',(-84.39,-2.40000000000001,68.8330657242578));
#55185=CARTESIAN_POINT('Ctrl Pts',(-84.39,-2.4,-68.8330657242578));
#55186=CARTESIAN_POINT('Ctrl Pts',(-84.39,-2.63794131567597,-68.7173110464923));
#55187=CARTESIAN_POINT('Ctrl Pts',(-84.3367792388686,-2.85976398178808,
-68.6312955463343));
#55188=CARTESIAN_POINT('Ctrl Pts',(-84.2088582275566,-3.14687252143927,
-68.5460136539367));
#55189=CARTESIAN_POINT('Ctrl Pts',(-84.1582563638478,-3.23512509191915,
-68.5249247721426));
#55190=CARTESIAN_POINT('Ctrl Pts',(-84.0743570265853,-3.35541450551661,
-68.5042990729588));
#55191=CARTESIAN_POINT('Ctrl Pts',(-84.0450550418941,-3.39350825317956,
-68.4992584438155));
#55192=CARTESIAN_POINT('Ctrl Pts',(-83.9995574704317,-3.44762883577759,
-68.4944494059773));
#55193=CARTESIAN_POINT('Ctrl Pts',(-83.9841338913747,-3.46516631110745,
-68.4933050443442));
#55194=CARTESIAN_POINT('Ctrl Pts',(-83.960666465638,-3.49072167918432,-68.4922764783636));
#55195=CARTESIAN_POINT('Ctrl Pts',(-83.9527886268885,-3.49911502874262,
-68.4920482857816));
#55196=CARTESIAN_POINT('Ctrl Pts',(-83.9408954481679,-3.51151809553136,
-68.4918779910258));
#55197=CARTESIAN_POINT('Ctrl Pts',(-83.9369183171401,-3.51562129354503,
-68.4918498917935));
#55198=CARTESIAN_POINT('Ctrl Pts',(-83.9289396665005,-3.52376551507611,
-68.4918510247012));
#55199=CARTESIAN_POINT('Ctrl Pts',(-83.9243381850882,-3.52840602779358,
-68.4918889124516));
#55200=CARTESIAN_POINT('Ctrl Pts',(-83.8117021285277,-3.64095335598249,
-68.49351390558));
#55201=CARTESIAN_POINT('Ctrl Pts',(-83.6663252298652,-3.7549446474807,-68.522729078502));
#55202=CARTESIAN_POINT('Ctrl Pts',(-83.2882501610162,-3.9347858753853,-68.6364382683655));
#55203=CARTESIAN_POINT('Ctrl Pts',(-83.055117522837,-4.,-68.7205706579609));
#55204=CARTESIAN_POINT('Ctrl Pts',(-82.79,-4.,-68.8330657242578));
#55205=CARTESIAN_POINT('Ctrl Pts',(-83.59,-2.4,-68.8330657242578));
#55206=CARTESIAN_POINT('Ctrl Pts',(-83.59,-2.51889840092331,-68.7173813501791));
#55207=CARTESIAN_POINT('Ctrl Pts',(-83.5633896194343,-2.62988199089404,
-68.6312955463343));
#55208=CARTESIAN_POINT('Ctrl Pts',(-83.4994291137783,-2.77343626071964,
-68.5460136539367));
#55209=CARTESIAN_POINT('Ctrl Pts',(-83.4741281819239,-2.81756254595958,
-68.5249247721426));
#55210=CARTESIAN_POINT('Ctrl Pts',(-83.4321785132927,-2.87770725275831,
-68.5042990729588));
#55211=CARTESIAN_POINT('Ctrl Pts',(-83.4175275209471,-2.89675412658978,
-68.4992584438155));
#55212=CARTESIAN_POINT('Ctrl Pts',(-83.3947787352159,-2.92381441788879,
-68.4944494059773));
#55213=CARTESIAN_POINT('Ctrl Pts',(-83.3870669456874,-2.93258315555372,
-68.4933050443442));
#55214=CARTESIAN_POINT('Ctrl Pts',(-83.375333232819,-2.94536083959216,-68.4922764783636));
#55215=CARTESIAN_POINT('Ctrl Pts',(-83.3713943134443,-2.94955751437131,
-68.4920482857816));
#55216=CARTESIAN_POINT('Ctrl Pts',(-83.3654477240839,-2.95575904776568,
-68.4918779910258));
#55217=CARTESIAN_POINT('Ctrl Pts',(-83.3634591585701,-2.95781064677251,
-68.4918498917935));
#55218=CARTESIAN_POINT('Ctrl Pts',(-83.3594698332502,-2.96188275753805,
-68.4918510247012));
#55219=CARTESIAN_POINT('Ctrl Pts',(-83.3571690925441,-2.96420301389679,
-68.4918889124516));
#55220=CARTESIAN_POINT('Ctrl Pts',(-83.3008510642638,-3.02047667799125,
-68.49351390558));
#55221=CARTESIAN_POINT('Ctrl Pts',(-83.2281626149326,-3.07747232374035,
-68.522729078502));
#55222=CARTESIAN_POINT('Ctrl Pts',(-83.0391250805081,-3.16739293769265,
-68.6364382683655));
#55223=CARTESIAN_POINT('Ctrl Pts',(-82.9224249571724,-3.2,-68.720684209999));
#55224=CARTESIAN_POINT('Ctrl Pts',(-82.79,-3.2,-68.8330657242578));
#55225=CARTESIAN_POINT('',(-83.7536699000375,-2.40000000000001,-68.8330657242578));
#55226=CARTESIAN_POINT('',(-84.39,-2.4,-68.8330657242578));
#55227=CARTESIAN_POINT('',(-84.39,-2.4,-68.8330657242578));
#55228=CARTESIAN_POINT('Ctrl Pts',(-83.59,-2.40000000000001,-68.8330657242578));
#55229=CARTESIAN_POINT('Ctrl Pts',(-83.59,-2.51889840092331,-68.7173813501791));
#55230=CARTESIAN_POINT('Ctrl Pts',(-83.5633896194343,-2.62988199089404,
-68.6312955463343));
#55231=CARTESIAN_POINT('Ctrl Pts',(-83.4994291137783,-2.77343626071964,
-68.5460136539367));
#55232=CARTESIAN_POINT('Ctrl Pts',(-83.4741281819239,-2.81756254595958,
-68.5249247721426));
#55233=CARTESIAN_POINT('Ctrl Pts',(-83.4321785132927,-2.87770725275831,
-68.5042990729588));
#55234=CARTESIAN_POINT('Ctrl Pts',(-83.4175275209471,-2.89675412658978,
-68.4992584438155));
#55235=CARTESIAN_POINT('Ctrl Pts',(-83.3947787352159,-2.92381441788879,
-68.4944494059773));
#55236=CARTESIAN_POINT('Ctrl Pts',(-83.3870669456874,-2.93258315555372,
-68.4933050443442));
#55237=CARTESIAN_POINT('Ctrl Pts',(-83.375333232819,-2.94536083959216,-68.4922764783636));
#55238=CARTESIAN_POINT('Ctrl Pts',(-83.3713943134443,-2.94955751437131,
-68.4920482857816));
#55239=CARTESIAN_POINT('Ctrl Pts',(-83.3654477240839,-2.95575904776568,
-68.4918779910258));
#55240=CARTESIAN_POINT('Ctrl Pts',(-83.3634591585701,-2.95781064677251,
-68.4918498917935));
#55241=CARTESIAN_POINT('Ctrl Pts',(-83.3594698332502,-2.96188275753805,
-68.4918510247012));
#55242=CARTESIAN_POINT('Ctrl Pts',(-83.3571690925441,-2.96420301389679,
-68.4918889124516));
#55243=CARTESIAN_POINT('Ctrl Pts',(-83.3008510642638,-3.02047667799125,
-68.49351390558));
#55244=CARTESIAN_POINT('Ctrl Pts',(-83.2281626149326,-3.07747232374035,
-68.522729078502));
#55245=CARTESIAN_POINT('Ctrl Pts',(-83.0391250805081,-3.16739293769265,
-68.6364382683655));
#55246=CARTESIAN_POINT('Ctrl Pts',(-82.9224249571724,-3.2,-68.720684209999));
#55247=CARTESIAN_POINT('Ctrl Pts',(-82.79,-3.2,-68.8330657242578));
#55248=CARTESIAN_POINT('Ctrl Pts',(-84.39,-2.4,-68.8330657242578));
#55249=CARTESIAN_POINT('Ctrl Pts',(-84.39,-2.48813503534456,-68.7901894268515));
#55250=CARTESIAN_POINT('Ctrl Pts',(-84.3826938673257,-2.57416721559184,
-68.7513422007595));
#55251=CARTESIAN_POINT('Ctrl Pts',(-84.3691286302924,-2.65729494508488,
-68.7165431137664));
#55252=CARTESIAN_POINT('Ctrl Pts',(-84.3547707287616,-2.74528012010299,
-68.6797105937609));
#55253=CARTESIAN_POINT('Ctrl Pts',(-84.3334016071155,-2.83001054231243,
-68.6474133539704));
#55254=CARTESIAN_POINT('Ctrl Pts',(-84.3063130289378,-2.91054986638528,
-68.6196465073015));
#55255=CARTESIAN_POINT('Ctrl Pts',(-84.2900151818667,-2.9590063626376,-68.6029405798922));
#55256=CARTESIAN_POINT('Ctrl Pts',(-84.2716479017026,-3.00594608985223,
-68.5878740346456));
#55257=CARTESIAN_POINT('Ctrl Pts',(-84.2514985646606,-3.05116967488887,
-68.5744409514026));
#55258=CARTESIAN_POINT('Ctrl Pts',(-84.2088582275566,-3.14687252143927,
-68.5460136539367));
#55259=CARTESIAN_POINT('Ctrl Pts',(-84.1582563638478,-3.23512509191915,
-68.5249247721426));
#55260=CARTESIAN_POINT('Ctrl Pts',(-84.1023234723395,-3.31531803431746,
-68.5111743060201));
#55261=CARTESIAN_POINT('Ctrl Pts',(-84.0743570265853,-3.35541450551661,
-68.5042990729588));
#55262=CARTESIAN_POINT('Ctrl Pts',(-84.0450550418941,-3.39350825317956,
-68.4992584438155));
#55263=CARTESIAN_POINT('Ctrl Pts',(-84.0147233275859,-3.42958864157825,
-68.4960524185901));
#55264=CARTESIAN_POINT('Ctrl Pts',(-83.9995574742425,-3.44762883124453,
-68.4944494063801));
#55265=CARTESIAN_POINT('Ctrl Pts',(-83.9841338990991,-3.46516630232284,
-68.4933050446909));
#55266=CARTESIAN_POINT('Ctrl Pts',(-83.9684889408216,-3.48220322310181,
-68.4926193336904));
#55267=CARTESIAN_POINT('Ctrl Pts',(-83.9606664557861,-3.49072168991274,
-68.4922764779317));
#55268=CARTESIAN_POINT('Ctrl Pts',(-83.9527886308731,-3.49911502458717,
-68.4920482858386));
#55269=CARTESIAN_POINT('Ctrl Pts',(-83.9448598410748,-3.50738373993511,
-68.4919347559444));
#55270=CARTESIAN_POINT('Ctrl Pts',(-83.9408954481679,-3.51151809553136,
-68.4918779910258));
#55271=CARTESIAN_POINT('Ctrl Pts',(-83.9369183171401,-3.51562129354502,
-68.4918498917935));
#55272=CARTESIAN_POINT('Ctrl Pts',(-83.9329289918203,-3.51969340431057,
-68.4918504582473));
#55273=CARTESIAN_POINT('Ctrl Pts',(-83.9289396665005,-3.5237655150761,-68.4918510247012));
#55274=CARTESIAN_POINT('Ctrl Pts',(-83.9243381850882,-3.52840602779357,
-68.4918889124516));
#55275=CARTESIAN_POINT('Ctrl Pts',(-83.920924971253,-3.5318165528902,-68.4919381546676));
#55276=CARTESIAN_POINT('Ctrl Pts',(-83.8117021285274,-3.64095335598243,
-68.49351390558));
#55277=CARTESIAN_POINT('Ctrl Pts',(-83.6663252298652,-3.75494464748069,
-68.522729078502));
#55278=CARTESIAN_POINT('Ctrl Pts',(-83.4772876954407,-3.84486526143299,
-68.5795836734338));
#55279=CARTESIAN_POINT('Ctrl Pts',(-83.4153903738218,-3.87430833039238,
-68.5981998025465));
#55280=CARTESIAN_POINT('Ctrl Pts',(-83.3486969172739,-3.90113222387641,
-68.6197620638315));
#55281=CARTESIAN_POINT('Ctrl Pts',(-83.2776875114855,-3.92387411898109,
-68.6442957957694));
#55282=CARTESIAN_POINT('Ctrl Pts',(-83.2099078531827,-3.94558163592534,
-68.667713650759));
#55283=CARTESIAN_POINT('Ctrl Pts',(-83.1381966655355,-3.96356858887681,
-68.6938386981164));
#55284=CARTESIAN_POINT('Ctrl Pts',(-83.063001996463,-3.97659085060749,-68.7226721477443));
#55285=CARTESIAN_POINT('Ctrl Pts',(-82.9931654332377,-3.9886851920802,-68.7494510278535));
#55286=CARTESIAN_POINT('Ctrl Pts',(-82.920324731768,-3.99649647540249,-68.7785659004566));
#55287=CARTESIAN_POINT('Ctrl Pts',(-82.8448564113475,-3.99906699817842,
-68.810001574992));
#55288=CARTESIAN_POINT('Ctrl Pts',(-82.8267208365865,-3.9996847131046,-68.8175557914172));
#55289=CARTESIAN_POINT('Ctrl Pts',(-82.8084335870332,-4.,-68.825243956865));
#55290=CARTESIAN_POINT('Ctrl Pts',(-82.79,-4.,-68.8330657242578));
#55291=CARTESIAN_POINT('Origin',(-82.79,-2.4,137.681359688174));
#55292=CARTESIAN_POINT('Origin',(-82.79,-2.4,137.681359688174));
#55293=CARTESIAN_POINT('Origin',(-93.59,-1.84247779607695,-70.));
#55294=CARTESIAN_POINT('',(-82.79,-1.84247779607695,-80.));
#55295=CARTESIAN_POINT('',(-93.59,-1.84247779607695,-70.));
#55296=CARTESIAN_POINT('Origin',(-82.79,-2.40000000000001,-80.));
#55297=CARTESIAN_POINT('',(-82.79,86.,-80.));
#55298=CARTESIAN_POINT('Origin',(-84.39,91.,80.));
#55299=CARTESIAN_POINT('',(-84.39,91.,-75.));
#55300=CARTESIAN_POINT('',(-84.39,91.,75.));
#55301=CARTESIAN_POINT('Origin',(-82.79,-3.20000000000001,80.));
#55302=CARTESIAN_POINT('',(-82.79,86.,80.));
#55303=CARTESIAN_POINT('',(-82.79,-1.84247779607695,80.));
#55304=CARTESIAN_POINT('Origin',(-93.59,-1.84247779607695,70.));
#55305=CARTESIAN_POINT('',(-93.59,-1.84247779607695,70.));
#55306=CARTESIAN_POINT('Origin',(-93.59,-3.34247779607695,70.));
#55307=CARTESIAN_POINT('Origin',(-93.59,-3.34247779607695,-70.));
#55308=CARTESIAN_POINT('Ctrl Pts',(70.61,-2.4,68.8330657242578));
#55309=CARTESIAN_POINT('Ctrl Pts',(70.61,-2.63794131567576,68.7173110464924));
#55310=CARTESIAN_POINT('Ctrl Pts',(70.5567792388688,-2.8597639817878,68.6312955463345));
#55311=CARTESIAN_POINT('Ctrl Pts',(70.4288582275568,-3.146872521439,68.5460136539369));
#55312=CARTESIAN_POINT('Ctrl Pts',(70.378256363848,-3.23512509191891,68.5249247721427));
#55313=CARTESIAN_POINT('Ctrl Pts',(70.2943570265855,-3.35541450551644,68.5042990729589));
#55314=CARTESIAN_POINT('Ctrl Pts',(70.2650550418943,-3.39350825317942,68.4992584438156));
#55315=CARTESIAN_POINT('Ctrl Pts',(70.2195574704318,-3.44762883577749,68.4944494059775));
#55316=CARTESIAN_POINT('Ctrl Pts',(70.2041338913749,-3.46516631110737,68.4933050443442));
#55317=CARTESIAN_POINT('Ctrl Pts',(70.1806664656381,-3.49072167918427,68.4922764783636));
#55318=CARTESIAN_POINT('Ctrl Pts',(70.1727886268886,-3.49911502874257,68.4920482857815));
#55319=CARTESIAN_POINT('Ctrl Pts',(70.160895448168,-3.51151809553133,68.4918779910258));
#55320=CARTESIAN_POINT('Ctrl Pts',(70.1569183171401,-3.515621293545,68.4918498917935));
#55321=CARTESIAN_POINT('Ctrl Pts',(70.1489396665006,-3.52376551507609,68.4918510247012));
#55322=CARTESIAN_POINT('Ctrl Pts',(70.1443381850882,-3.52840602779357,68.4918889124516));
#55323=CARTESIAN_POINT('Ctrl Pts',(70.0317021285279,-3.64095335598228,68.4935139055799));
#55324=CARTESIAN_POINT('Ctrl Pts',(69.8863252298656,-3.75494464748045,68.5227290785018));
#55325=CARTESIAN_POINT('Ctrl Pts',(69.5082501610166,-3.93478587538516,68.6364382683652));
#55326=CARTESIAN_POINT('Ctrl Pts',(69.2751175228373,-4.,68.7205706579607));
#55327=CARTESIAN_POINT('Ctrl Pts',(69.01,-4.,68.8330657242578));
#55328=CARTESIAN_POINT('Ctrl Pts',(69.81,-2.4,68.8330657242578));
#55329=CARTESIAN_POINT('Ctrl Pts',(69.81,-2.51889840092321,68.7173813501793));
#55330=CARTESIAN_POINT('Ctrl Pts',(69.7833896194344,-2.6298819908939,68.6312955463345));
#55331=CARTESIAN_POINT('Ctrl Pts',(69.7194291137784,-2.7734362607195,68.5460136539369));
#55332=CARTESIAN_POINT('Ctrl Pts',(69.694128181924,-2.81756254595946,68.5249247721427));
#55333=CARTESIAN_POINT('Ctrl Pts',(69.6521785132928,-2.87770725275822,68.5042990729589));
#55334=CARTESIAN_POINT('Ctrl Pts',(69.6375275209471,-2.89675412658971,68.4992584438156));
#55335=CARTESIAN_POINT('Ctrl Pts',(69.6147787352159,-2.92381441788875,68.4944494059775));
#55336=CARTESIAN_POINT('Ctrl Pts',(69.6070669456874,-2.93258315555369,68.4933050443442));
#55337=CARTESIAN_POINT('Ctrl Pts',(69.595333232819,-2.94536083959214,68.4922764783636));
#55338=CARTESIAN_POINT('Ctrl Pts',(69.5913943134443,-2.94955751437128,68.4920482857815));
#55339=CARTESIAN_POINT('Ctrl Pts',(69.585447724084,-2.95575904776566,68.4918779910258));
#55340=CARTESIAN_POINT('Ctrl Pts',(69.5834591585701,-2.9578106467725,68.4918498917935));
#55341=CARTESIAN_POINT('Ctrl Pts',(69.5794698332503,-2.96188275753804,68.4918510247012));
#55342=CARTESIAN_POINT('Ctrl Pts',(69.5771690925441,-2.96420301389679,68.4918889124516));
#55343=CARTESIAN_POINT('Ctrl Pts',(69.520851064264,-3.02047667799114,68.4935139055799));
#55344=CARTESIAN_POINT('Ctrl Pts',(69.4481626149328,-3.07747232374023,68.5227290785018));
#55345=CARTESIAN_POINT('Ctrl Pts',(69.2591250805083,-3.16739293769258,68.6364382683652));
#55346=CARTESIAN_POINT('Ctrl Pts',(69.1424249571726,-3.2,68.7206842099989));
#55347=CARTESIAN_POINT('Ctrl Pts',(69.01,-3.2,68.8330657242578));
#55348=CARTESIAN_POINT('',(69.9736699000372,-2.4,68.8330657242578));
#55349=CARTESIAN_POINT('',(70.61,-2.4,68.8330657242578));
#55350=CARTESIAN_POINT('',(70.61,-2.4,68.8330657242578));
#55351=CARTESIAN_POINT('Ctrl Pts',(69.81,-2.4,68.8330657242578));
#55352=CARTESIAN_POINT('Ctrl Pts',(69.81,-2.51889840092321,68.7173813501793));
#55353=CARTESIAN_POINT('Ctrl Pts',(69.7833896194344,-2.6298819908939,68.6312955463345));
#55354=CARTESIAN_POINT('Ctrl Pts',(69.7194291137784,-2.7734362607195,68.5460136539369));
#55355=CARTESIAN_POINT('Ctrl Pts',(69.694128181924,-2.81756254595946,68.5249247721427));
#55356=CARTESIAN_POINT('Ctrl Pts',(69.6521785132928,-2.87770725275822,68.5042990729589));
#55357=CARTESIAN_POINT('Ctrl Pts',(69.6375275209471,-2.89675412658971,68.4992584438156));
#55358=CARTESIAN_POINT('Ctrl Pts',(69.6147787352159,-2.92381441788875,68.4944494059775));
#55359=CARTESIAN_POINT('Ctrl Pts',(69.6070669456874,-2.93258315555369,68.4933050443442));
#55360=CARTESIAN_POINT('Ctrl Pts',(69.595333232819,-2.94536083959214,68.4922764783636));
#55361=CARTESIAN_POINT('Ctrl Pts',(69.5913943134443,-2.94955751437128,68.4920482857815));
#55362=CARTESIAN_POINT('Ctrl Pts',(69.585447724084,-2.95575904776566,68.4918779910258));
#55363=CARTESIAN_POINT('Ctrl Pts',(69.5834591585701,-2.9578106467725,68.4918498917935));
#55364=CARTESIAN_POINT('Ctrl Pts',(69.5794698332503,-2.96188275753804,68.4918510247012));
#55365=CARTESIAN_POINT('Ctrl Pts',(69.5771690925441,-2.96420301389679,68.4918889124516));
#55366=CARTESIAN_POINT('Ctrl Pts',(69.520851064264,-3.02047667799114,68.4935139055799));
#55367=CARTESIAN_POINT('Ctrl Pts',(69.4481626149328,-3.07747232374023,68.5227290785018));
#55368=CARTESIAN_POINT('Ctrl Pts',(69.2591250805083,-3.16739293769258,68.6364382683652));
#55369=CARTESIAN_POINT('Ctrl Pts',(69.1424249571726,-3.2,68.7206842099989));
#55370=CARTESIAN_POINT('Ctrl Pts',(69.01,-3.2,68.8330657242578));
#55371=CARTESIAN_POINT('Ctrl Pts',(70.61,-2.4,68.8330657242578));
#55372=CARTESIAN_POINT('Ctrl Pts',(70.61,-2.48813503534593,68.7901894268509));
#55373=CARTESIAN_POINT('Ctrl Pts',(70.6026938673255,-2.57416721559453,68.7513422007584));
#55374=CARTESIAN_POINT('Ctrl Pts',(70.5891286302918,-2.65729494508879,68.7165431137648));
#55375=CARTESIAN_POINT('Ctrl Pts',(70.5747707287605,-2.7452801201082,68.6797105937589));
#55376=CARTESIAN_POINT('Ctrl Pts',(70.5534016071138,-2.83001054231882,68.6474133539681));
#55377=CARTESIAN_POINT('Ctrl Pts',(70.5263130289353,-2.91054986639271,68.619646507299));
#55378=CARTESIAN_POINT('Ctrl Pts',(70.5100151818649,-2.9590063626423,68.6029405798908));
#55379=CARTESIAN_POINT('Ctrl Pts',(70.4916479017016,-3.00594608985435,68.5878740346451));
#55380=CARTESIAN_POINT('Ctrl Pts',(70.4714985646607,-3.0511696748886,68.5744409514028));
#55381=CARTESIAN_POINT('Ctrl Pts',(70.4288582275567,-3.14687252143901,68.5460136539369));
#55382=CARTESIAN_POINT('Ctrl Pts',(70.3782563638479,-3.23512509191891,68.5249247721427));
#55383=CARTESIAN_POINT('Ctrl Pts',(70.3223234723396,-3.31531803431726,68.5111743060202));
#55384=CARTESIAN_POINT('Ctrl Pts',(70.2943570265855,-3.35541450551644,68.5042990729589));
#55385=CARTESIAN_POINT('Ctrl Pts',(70.2650550418943,-3.39350825317941,68.4992584438156));
#55386=CARTESIAN_POINT('Ctrl Pts',(70.234723327586,-3.42958864157812,68.4960524185902));
#55387=CARTESIAN_POINT('Ctrl Pts',(70.2195574742427,-3.44762883124441,68.4944494063803));
#55388=CARTESIAN_POINT('Ctrl Pts',(70.2041338990992,-3.46516630232275,68.4933050446909));
#55389=CARTESIAN_POINT('Ctrl Pts',(70.1884889408217,-3.48220322310175,68.4926193336904));
#55390=CARTESIAN_POINT('Ctrl Pts',(70.1806664557862,-3.4907216899127,68.4922764779317));
#55391=CARTESIAN_POINT('Ctrl Pts',(70.1727886308732,-3.49911502458712,68.4920482858386));
#55392=CARTESIAN_POINT('Ctrl Pts',(70.1648598410748,-3.50738373993507,68.4919347559444));
#55393=CARTESIAN_POINT('Ctrl Pts',(70.160895448168,-3.51151809553132,68.4918779910258));
#55394=CARTESIAN_POINT('Ctrl Pts',(70.1569183171401,-3.51562129354499,68.4918498917935));
#55395=CARTESIAN_POINT('Ctrl Pts',(70.1529289918203,-3.51969340431054,68.4918504582473));
#55396=CARTESIAN_POINT('Ctrl Pts',(70.1489396665006,-3.52376551507608,68.4918510247012));
#55397=CARTESIAN_POINT('Ctrl Pts',(70.1443381850882,-3.52840602779357,68.4918889124516));
#55398=CARTESIAN_POINT('Ctrl Pts',(70.1409249712531,-3.5318165528902,68.4919381546676));
#55399=CARTESIAN_POINT('Ctrl Pts',(70.0317021285278,-3.64095335598229,68.4935139055799));
#55400=CARTESIAN_POINT('Ctrl Pts',(69.8863252298656,-3.75494464748044,68.5227290785018));
#55401=CARTESIAN_POINT('Ctrl Pts',(69.6972876954411,-3.8448652614328,68.5795836734335));
#55402=CARTESIAN_POINT('Ctrl Pts',(69.6353903738228,-3.87430833039194,68.5981998025461));
#55403=CARTESIAN_POINT('Ctrl Pts',(69.5686969172756,-3.90113222387577,68.6197620638309));
#55404=CARTESIAN_POINT('Ctrl Pts',(69.4976875114879,-3.92387411898034,68.6442957957685));
#55405=CARTESIAN_POINT('Ctrl Pts',(69.4299078531858,-3.94558163592449,68.6677136507578));
#55406=CARTESIAN_POINT('Ctrl Pts',(69.3581966655392,-3.96356858887595,68.693838698115));
#55407=CARTESIAN_POINT('Ctrl Pts',(69.2830019964674,-3.97659085060672,68.7226721477426));
#55408=CARTESIAN_POINT('Ctrl Pts',(69.2131654332428,-3.98868519207953,68.7494510278515));
#55409=CARTESIAN_POINT('Ctrl Pts',(69.1403247317738,-3.99649647540199,68.7785659004542));
#55410=CARTESIAN_POINT('Ctrl Pts',(69.0648564113539,-3.9990669981782,68.8100015749893));
#55411=CARTESIAN_POINT('Ctrl Pts',(69.0467208365909,-3.99968471310452,68.8175557914153));
#55412=CARTESIAN_POINT('Ctrl Pts',(69.0284335870354,-4.,68.825243956864));
#55413=CARTESIAN_POINT('Ctrl Pts',(69.01,-4.,68.8330657242578));
#55414=CARTESIAN_POINT('Ctrl Pts',(69.01,-4.,-68.8330657242578));
#55415=CARTESIAN_POINT('Ctrl Pts',(69.2479413156758,-4.,-68.7173110464924));
#55416=CARTESIAN_POINT('Ctrl Pts',(69.4697639817879,-3.94677923886873,-68.6312955463344));
#55417=CARTESIAN_POINT('Ctrl Pts',(69.7568725214391,-3.81885822755673,-68.5460136539369));
#55418=CARTESIAN_POINT('Ctrl Pts',(69.845125091919,-3.76825636384791,-68.5249247721427));
#55419=CARTESIAN_POINT('Ctrl Pts',(69.9654145055165,-3.68435702658545,-68.5042990729589));
#55420=CARTESIAN_POINT('Ctrl Pts',(70.0035082531795,-3.65505504189424,-68.4992584438156));
#55421=CARTESIAN_POINT('Ctrl Pts',(70.0576288357775,-3.6095574704318,-68.4944494059774));
#55422=CARTESIAN_POINT('Ctrl Pts',(70.0751663111074,-3.59413389137481,-68.4933050443442));
#55423=CARTESIAN_POINT('Ctrl Pts',(70.1007216791843,-3.57066646563801,-68.4922764783636));
#55424=CARTESIAN_POINT('Ctrl Pts',(70.1091150287426,-3.56278862688857,-68.4920482857816));
#55425=CARTESIAN_POINT('Ctrl Pts',(70.1215180955314,-3.55089544816793,-68.4918779910258));
#55426=CARTESIAN_POINT('Ctrl Pts',(70.125621293545,-3.54691831714011,-68.4918498917935));
#55427=CARTESIAN_POINT('Ctrl Pts',(70.1337655150761,-3.53893966650051,-68.4918510247012));
#55428=CARTESIAN_POINT('Ctrl Pts',(70.1384060277936,-3.5343381850882,-68.4918889124516));
#55429=CARTESIAN_POINT('Ctrl Pts',(70.2509533559824,-3.42170212852781,-68.4935139055799));
#55430=CARTESIAN_POINT('Ctrl Pts',(70.3649446474806,-3.27632522986542,-68.5227290785019));
#55431=CARTESIAN_POINT('Ctrl Pts',(70.5447858753852,-2.89825016101646,-68.6364382683653));
#55432=CARTESIAN_POINT('Ctrl Pts',(70.61,-2.66511752283727,-68.7205706579607));
#55433=CARTESIAN_POINT('Ctrl Pts',(70.61,-2.4,-68.8330657242578));
#55434=CARTESIAN_POINT('Ctrl Pts',(69.01,-3.2,-68.8330657242578));
#55435=CARTESIAN_POINT('Ctrl Pts',(69.1288984009232,-3.2,-68.7173813501792));
#55436=CARTESIAN_POINT('Ctrl Pts',(69.2398819908939,-3.17338961943437,-68.6312955463344));
#55437=CARTESIAN_POINT('Ctrl Pts',(69.3834362607195,-3.10942911377837,-68.5460136539369));
#55438=CARTESIAN_POINT('Ctrl Pts',(69.4275625459595,-3.08412818192396,-68.5249247721427));
#55439=CARTESIAN_POINT('Ctrl Pts',(69.4877072527583,-3.04217851329272,-68.5042990729589));
#55440=CARTESIAN_POINT('Ctrl Pts',(69.5067541265897,-3.02752752094712,-68.4992584438156));
#55441=CARTESIAN_POINT('Ctrl Pts',(69.5338144178888,-3.0047787352159,-68.4944494059774));
#55442=CARTESIAN_POINT('Ctrl Pts',(69.5425831555537,-2.99706694568741,-68.4933050443442));
#55443=CARTESIAN_POINT('Ctrl Pts',(69.5553608395922,-2.98533323281901,-68.4922764783636));
#55444=CARTESIAN_POINT('Ctrl Pts',(69.5595575143713,-2.98139431344429,-68.4920482857816));
#55445=CARTESIAN_POINT('Ctrl Pts',(69.5657590477657,-2.97544772408396,-68.4918779910258));
#55446=CARTESIAN_POINT('Ctrl Pts',(69.5678106467725,-2.97345915857006,-68.4918498917935));
#55447=CARTESIAN_POINT('Ctrl Pts',(69.5718827575381,-2.96946983325026,-68.4918510247012));
#55448=CARTESIAN_POINT('Ctrl Pts',(69.5742030138968,-2.9671690925441,-68.4918889124516));
#55449=CARTESIAN_POINT('Ctrl Pts',(69.6304766779912,-2.9108510642639,-68.4935139055799));
#55450=CARTESIAN_POINT('Ctrl Pts',(69.6874723237403,-2.83816261493271,-68.5227290785019));
#55451=CARTESIAN_POINT('Ctrl Pts',(69.7773929376926,-2.64912508050823,-68.6364382683653));
#55452=CARTESIAN_POINT('Ctrl Pts',(69.81,-2.53242495717256,-68.7206842099989));
#55453=CARTESIAN_POINT('Ctrl Pts',(69.81,-2.4,-68.8330657242578));
#55454=CARTESIAN_POINT('Ctrl Pts',(69.01,-3.2,-68.8330657242578));
#55455=CARTESIAN_POINT('Ctrl Pts',(69.1288984009232,-3.2,-68.7173813501792));
#55456=CARTESIAN_POINT('Ctrl Pts',(69.2398819908939,-3.17338961943437,-68.6312955463344));
#55457=CARTESIAN_POINT('Ctrl Pts',(69.3834362607195,-3.10942911377837,-68.5460136539369));
#55458=CARTESIAN_POINT('Ctrl Pts',(69.4275625459595,-3.08412818192396,-68.5249247721427));
#55459=CARTESIAN_POINT('Ctrl Pts',(69.4877072527583,-3.04217851329272,-68.5042990729589));
#55460=CARTESIAN_POINT('Ctrl Pts',(69.5067541265897,-3.02752752094712,-68.4992584438156));
#55461=CARTESIAN_POINT('Ctrl Pts',(69.5338144178888,-3.0047787352159,-68.4944494059774));
#55462=CARTESIAN_POINT('Ctrl Pts',(69.5425831555537,-2.99706694568741,-68.4933050443442));
#55463=CARTESIAN_POINT('Ctrl Pts',(69.5553608395922,-2.98533323281901,-68.4922764783636));
#55464=CARTESIAN_POINT('Ctrl Pts',(69.5595575143713,-2.98139431344429,-68.4920482857816));
#55465=CARTESIAN_POINT('Ctrl Pts',(69.5657590477657,-2.97544772408396,-68.4918779910258));
#55466=CARTESIAN_POINT('Ctrl Pts',(69.5678106467725,-2.97345915857006,-68.4918498917935));
#55467=CARTESIAN_POINT('Ctrl Pts',(69.5718827575381,-2.96946983325026,-68.4918510247012));
#55468=CARTESIAN_POINT('Ctrl Pts',(69.5742030138968,-2.9671690925441,-68.4918889124516));
#55469=CARTESIAN_POINT('Ctrl Pts',(69.6304766779912,-2.9108510642639,-68.4935139055799));
#55470=CARTESIAN_POINT('Ctrl Pts',(69.6874723237403,-2.83816261493271,-68.5227290785019));
#55471=CARTESIAN_POINT('Ctrl Pts',(69.7773929376926,-2.64912508050823,-68.6364382683653));
#55472=CARTESIAN_POINT('Ctrl Pts',(69.81,-2.53242495717256,-68.7206842099989));
#55473=CARTESIAN_POINT('Ctrl Pts',(69.81,-2.4,-68.8330657242578));
#55474=CARTESIAN_POINT('',(69.8505628535685,-2.4,-68.8330657242578));
#55475=CARTESIAN_POINT('',(69.81,-2.4,-68.8330657242578));
#55476=CARTESIAN_POINT('',(69.81,-2.4,-68.8330657242578));
#55477=CARTESIAN_POINT('Ctrl Pts',(69.01,-4.,-68.8330657242578));
#55478=CARTESIAN_POINT('Ctrl Pts',(69.0981350353444,-4.,-68.7901894268517));
#55479=CARTESIAN_POINT('Ctrl Pts',(69.1841672155914,-3.99269386732579,-68.7513422007598));
#55480=CARTESIAN_POINT('Ctrl Pts',(69.2672949450843,-3.97912863029249,-68.7165431137667));
#55481=CARTESIAN_POINT('Ctrl Pts',(69.3552801201021,-3.96477072876174,-68.6797105937613));
#55482=CARTESIAN_POINT('Ctrl Pts',(69.4400105423113,-3.9434016071158,-68.6474133539709));
#55483=CARTESIAN_POINT('Ctrl Pts',(69.520549866384,-3.91631302893826,-68.619646507302));
#55484=CARTESIAN_POINT('Ctrl Pts',(69.5690063626367,-3.90001518186709,-68.6029405798925));
#55485=CARTESIAN_POINT('Ctrl Pts',(69.6159460898517,-3.88164790170279,-68.5878740346459));
#55486=CARTESIAN_POINT('Ctrl Pts',(69.6611696748886,-3.86149856466073,-68.5744409514027));
#55487=CARTESIAN_POINT('Ctrl Pts',(69.756872521439,-3.81885822755673,-68.5460136539369));
#55488=CARTESIAN_POINT('Ctrl Pts',(69.845125091919,-3.76825636384791,-68.5249247721427));
#55489=CARTESIAN_POINT('Ctrl Pts',(69.9253180343173,-3.7123234723396,-68.5111743060202));
#55490=CARTESIAN_POINT('Ctrl Pts',(69.9654145055165,-3.68435702658545,-68.5042990729589));
#55491=CARTESIAN_POINT('Ctrl Pts',(70.0035082531795,-3.65505504189424,-68.4992584438156));
#55492=CARTESIAN_POINT('Ctrl Pts',(70.0395886415782,-3.62472332758594,-68.4960524185901));
#55493=CARTESIAN_POINT('Ctrl Pts',(70.0576288312445,-3.6095574742426,-68.4944494063802));
#55494=CARTESIAN_POINT('Ctrl Pts',(70.0751663023228,-3.59413389909915,-68.4933050446909));
#55495=CARTESIAN_POINT('Ctrl Pts',(70.0922032231018,-3.57848894082167,-68.4926193336904));
#55496=CARTESIAN_POINT('Ctrl Pts',(70.1007216899127,-3.57066645578614,-68.4922764779317));
#55497=CARTESIAN_POINT('Ctrl Pts',(70.1091150245872,-3.56278863087319,-68.4920482858386));
#55498=CARTESIAN_POINT('Ctrl Pts',(70.1173837399351,-3.55485984107481,-68.4919347559444));
#55499=CARTESIAN_POINT('Ctrl Pts',(70.1215180955314,-3.55089544816793,-68.4918779910258));
#55500=CARTESIAN_POINT('Ctrl Pts',(70.125621293545,-3.54691831714011,-68.4918498917935));
#55501=CARTESIAN_POINT('Ctrl Pts',(70.1296934043106,-3.54292899182031,-68.4918504582473));
#55502=CARTESIAN_POINT('Ctrl Pts',(70.1337655150761,-3.53893966650051,-68.4918510247012));
#55503=CARTESIAN_POINT('Ctrl Pts',(70.1384060277936,-3.53433818508819,-68.4918889124516));
#55504=CARTESIAN_POINT('Ctrl Pts',(70.1418165528902,-3.53092497125303,-68.4919381546676));
#55505=CARTESIAN_POINT('Ctrl Pts',(70.2509533559824,-3.42170212852774,-68.4935139055799));
#55506=CARTESIAN_POINT('Ctrl Pts',(70.3649446474806,-3.27632522986542,-68.5227290785019));
#55507=CARTESIAN_POINT('Ctrl Pts',(70.4548652614329,-3.08728769544094,-68.5795836734336));
#55508=CARTESIAN_POINT('Ctrl Pts',(70.4843083303921,-3.02539037382255,-68.5981998025462));
#55509=CARTESIAN_POINT('Ctrl Pts',(70.5111322238759,-2.95869691727524,-68.619762063831));
#55510=CARTESIAN_POINT('Ctrl Pts',(70.5338741189805,-2.88768751148745,-68.6442957957687));
#55511=CARTESIAN_POINT('Ctrl Pts',(70.5555816359246,-2.81990785318532,-68.667713650758));
#55512=CARTESIAN_POINT('Ctrl Pts',(70.573568588876,-2.74819666553881,-68.6938386981152));
#55513=CARTESIAN_POINT('Ctrl Pts',(70.5865908506068,-2.67300199646701,-68.7226721477428));
#55514=CARTESIAN_POINT('Ctrl Pts',(70.5986851920796,-2.60316543324227,-68.7494510278517));
#55515=CARTESIAN_POINT('Ctrl Pts',(70.6064964754021,-2.53032473177313,-68.7785659004545));
#55516=CARTESIAN_POINT('Ctrl Pts',(70.6090669981782,-2.45485641135309,-68.8100015749897));
#55517=CARTESIAN_POINT('Ctrl Pts',(70.6096847131045,-2.4367208365903,-68.8175557914156));
#55518=CARTESIAN_POINT('Ctrl Pts',(70.61,-2.41843358703513,-68.8252439568642));
#55519=CARTESIAN_POINT('Ctrl Pts',(70.61,-2.4,-68.8330657242578));
#55520=CARTESIAN_POINT('Origin',(69.01,-2.4,-137.681359688174));
#55521=CARTESIAN_POINT('Origin',(69.01,-2.4,-137.681359688174));
#55522=CARTESIAN_POINT('Origin',(79.81,-1.84247779607689,70.));
#55523=CARTESIAN_POINT('',(-82.79,-1.84247779607832,80.));
#55524=CARTESIAN_POINT('',(79.81,-1.84247779607689,70.));
#55525=CARTESIAN_POINT('Origin',(-82.79,-2.4,80.));
#55526=CARTESIAN_POINT('',(69.81,86.,80.));
#55527=CARTESIAN_POINT('Origin',(69.81,91.,80.));
#55528=CARTESIAN_POINT('',(69.81,91.,-75.));
#55529=CARTESIAN_POINT('',(70.61,91.,75.));
#55530=CARTESIAN_POINT('Origin',(69.01,-3.19999999999999,-80.));
#55531=CARTESIAN_POINT('',(69.01,86.,-80.));
#55532=CARTESIAN_POINT('',(69.01,-1.84247779607698,-80.));
#55533=CARTESIAN_POINT('Origin',(79.81,-1.84247779607689,-70.));
#55534=CARTESIAN_POINT('',(79.81,-1.84247779607689,-70.));
#55535=CARTESIAN_POINT('Origin',(79.81,-3.3424777960769,-70.));
#55536=CARTESIAN_POINT('Origin',(79.81,-3.3424777960769,70.));
#55537=CARTESIAN_POINT('Origin',(61.61,-4.,-68.39));
#55538=CARTESIAN_POINT('Origin',(56.338675369116,-2.,-68.39));
#55539=CARTESIAN_POINT('Origin',(66.8813246308841,-2.,-68.39));
#55540=CARTESIAN_POINT('Origin',(61.61,-4.,-64.39));
#55541=CARTESIAN_POINT('Origin',(66.8813246308841,-2.,-64.39));
#55542=CARTESIAN_POINT('Origin',(56.338675369116,-2.,-64.39));
#55543=CARTESIAN_POINT('Origin',(56.338675369116,-2.,-68.39));
#55544=CARTESIAN_POINT('',(58.1495932410337,-2.84886775246144,-68.39));
#55545=CARTESIAN_POINT('Origin',(56.338675369116,-2.,-68.39));
#55546=CARTESIAN_POINT('',(58.1495932410337,-2.84886775246144,-64.39));
#55547=CARTESIAN_POINT('',(58.1495932410337,-2.84886775246144,-68.39));
#55548=CARTESIAN_POINT('Origin',(56.338675369116,-2.,-64.39));
#55549=CARTESIAN_POINT('Origin',(66.8813246308841,-2.,-66.39));
#55550=CARTESIAN_POINT('',(65.0704067589663,-2.84886775246144,-64.39));
#55551=CARTESIAN_POINT('Origin',(66.8813246308841,-2.,-64.39));
#55552=CARTESIAN_POINT('',(65.0704067589663,-2.84886775246144,-68.39));
#55553=CARTESIAN_POINT('',(65.0704067589663,-2.84886775246144,-68.39));
#55554=CARTESIAN_POINT('Origin',(66.8813246308841,-2.,-68.39));
#55555=CARTESIAN_POINT('Origin',(66.8813246308841,-2.,-64.39));
#55556=CARTESIAN_POINT('',(57.4252260922666,-2.50932065147687,-64.39));
#55557=CARTESIAN_POINT('Origin',(56.338675369116,-2.,-64.39));
#55558=CARTESIAN_POINT('',(58.7053050692247,-1.66334918565392,-64.39));
#55559=CARTESIAN_POINT('',(59.11,-0.8,-64.39));
#55560=CARTESIAN_POINT('',(60.0634934731631,-0.8,-64.39));
#55561=CARTESIAN_POINT('Origin',(60.0634934731631,-2.3,-64.39));
#55562=CARTESIAN_POINT('',(63.156506526837,-0.8,-64.39));
#55563=CARTESIAN_POINT('',(59.11,-0.8,-64.39));
#55564=CARTESIAN_POINT('',(64.5146949307753,-1.66334918565392,-64.39));
#55565=CARTESIAN_POINT('Origin',(63.156506526837,-2.3,-64.39));
#55566=CARTESIAN_POINT('',(64.11,-0.8,-64.39));
#55567=CARTESIAN_POINT('',(65.7947739077334,-2.50932065147687,-64.39));
#55568=CARTESIAN_POINT('Origin',(66.8813246308841,-2.,-64.39));
#55569=CARTESIAN_POINT('',(65.2390620795424,-1.32380208466934,-64.39));
#55570=CARTESIAN_POINT('',(64.8343671487671,-0.460452899015424,-64.39));
#55571=CARTESIAN_POINT('',(63.156506526837,1.0842021724855E-16,-64.39));
#55572=CARTESIAN_POINT('Origin',(63.156506526837,-2.3,-64.39));
#55573=CARTESIAN_POINT('',(60.0634934731631,-4.33680868994202E-16,-64.39));
#55574=CARTESIAN_POINT('',(59.11,1.0842021724855E-16,-64.39));
#55575=CARTESIAN_POINT('',(57.9809379204577,-1.32380208466934,-64.39));
#55576=CARTESIAN_POINT('Origin',(60.0634934731631,-2.3,-64.39));
#55577=CARTESIAN_POINT('',(58.3856328512329,-0.460452899015424,-64.39));
#55578=CARTESIAN_POINT('Origin',(59.11,-0.8,-68.39));
#55579=CARTESIAN_POINT('',(65.7947739077334,-2.50932065147687,-68.39));
#55580=CARTESIAN_POINT('Origin',(66.8813246308841,-2.,-68.39));
#55581=CARTESIAN_POINT('',(64.5146949307753,-1.66334918565392,-68.39));
#55582=CARTESIAN_POINT('',(64.11,-0.8,-68.39));
#55583=CARTESIAN_POINT('',(63.156506526837,-0.8,-68.39));
#55584=CARTESIAN_POINT('Origin',(63.156506526837,-2.3,-68.39));
#55585=CARTESIAN_POINT('',(60.0634934731631,-0.8,-68.39));
#55586=CARTESIAN_POINT('',(59.11,-0.8,-68.39));
#55587=CARTESIAN_POINT('',(58.7053050692247,-1.66334918565392,-68.39));
#55588=CARTESIAN_POINT('Origin',(60.0634934731631,-2.3,-68.39));
#55589=CARTESIAN_POINT('',(59.11,-0.8,-68.39));
#55590=CARTESIAN_POINT('',(57.4252260922666,-2.50932065147687,-68.39));
#55591=CARTESIAN_POINT('Origin',(56.338675369116,-2.,-68.39));
#55592=CARTESIAN_POINT('',(57.9809379204577,-1.32380208466934,-68.39));
#55593=CARTESIAN_POINT('',(58.3856328512329,-0.460452899015424,-68.39));
#55594=CARTESIAN_POINT('',(60.0634934731631,1.0842021724855E-16,-68.39));
#55595=CARTESIAN_POINT('Origin',(60.0634934731631,-2.3,-68.39));
#55596=CARTESIAN_POINT('',(63.156506526837,1.0842021724855E-16,-68.39));
#55597=CARTESIAN_POINT('',(59.11,1.0842021724855E-16,-68.39));
#55598=CARTESIAN_POINT('',(65.2390620795424,-1.32380208466934,-68.39));
#55599=CARTESIAN_POINT('Origin',(63.156506526837,-2.3,-68.39));
#55600=CARTESIAN_POINT('',(64.8343671487671,-0.460452899015424,-68.39));
#55601=CARTESIAN_POINT('Origin',(60.0634934731631,-2.3,-68.39));
#55602=CARTESIAN_POINT('',(60.0634934731631,-0.8,-68.39));
#55603=CARTESIAN_POINT('',(58.7053050692247,-1.66334918565392,-68.39));
#55604=CARTESIAN_POINT('Origin',(63.156506526837,-2.3,-68.39));
#55605=CARTESIAN_POINT('',(64.5146949307753,-1.66334918565392,-68.39));
#55606=CARTESIAN_POINT('',(63.156506526837,-0.8,-68.39));
#55607=CARTESIAN_POINT('Origin',(59.11,-0.8,-68.39));
#55608=CARTESIAN_POINT('Origin',(64.11,-0.8,-68.39));
#55609=CARTESIAN_POINT('Origin',(59.11,-0.8,-68.39));
#55610=CARTESIAN_POINT('Origin',(60.0634934731631,-2.3,-68.39));
#55611=CARTESIAN_POINT('',(57.9809379204577,-1.32380208466934,-68.39));
#55612=CARTESIAN_POINT('',(60.0634934731631,1.0842021724855E-16,-68.39));
#55613=CARTESIAN_POINT('Origin',(63.156506526837,-2.3,-68.39));
#55614=CARTESIAN_POINT('',(63.156506526837,1.0842021724855E-16,-68.39));
#55615=CARTESIAN_POINT('',(65.2390620795424,-1.32380208466934,-68.39));
#55616=CARTESIAN_POINT('Origin',(66.8813246308841,-2.,-66.39));
#55617=CARTESIAN_POINT('',(65.7947739077334,-2.50932065147687,-68.39));
#55618=CARTESIAN_POINT('Origin',(56.338675369116,-2.,-68.39));
#55619=CARTESIAN_POINT('',(57.4252260922666,-2.50932065147687,-68.39));
#55620=CARTESIAN_POINT('Origin',(58.3856328512329,-0.460452899015424,-68.39));
#55621=CARTESIAN_POINT('Origin',(64.8343671487671,-0.460452899015424,-68.39));
#55622=CARTESIAN_POINT('Origin',(59.11,1.0842021724855E-16,-68.39));
#55623=CARTESIAN_POINT('Origin',(61.61,-4.,65.61));
#55624=CARTESIAN_POINT('Origin',(56.338675369116,-2.,65.61));
#55625=CARTESIAN_POINT('Origin',(66.8813246308841,-2.,65.61));
#55626=CARTESIAN_POINT('Origin',(61.61,-4.,69.61));
#55627=CARTESIAN_POINT('Origin',(66.8813246308841,-2.,69.61));
#55628=CARTESIAN_POINT('Origin',(56.338675369116,-2.,69.61));
#55629=CARTESIAN_POINT('Origin',(56.338675369116,-2.,65.61));
#55630=CARTESIAN_POINT('',(58.1495932410337,-2.84886775246144,65.61));
#55631=CARTESIAN_POINT('Origin',(56.338675369116,-2.,65.61));
#55632=CARTESIAN_POINT('',(58.1495932410337,-2.84886775246144,69.61));
#55633=CARTESIAN_POINT('',(58.1495932410337,-2.84886775246144,65.61));
#55634=CARTESIAN_POINT('Origin',(56.338675369116,-2.,69.61));
#55635=CARTESIAN_POINT('Origin',(66.8813246308841,-2.,67.61));
#55636=CARTESIAN_POINT('',(65.0704067589663,-2.84886775246144,69.61));
#55637=CARTESIAN_POINT('Origin',(66.8813246308841,-2.,69.61));
#55638=CARTESIAN_POINT('',(65.0704067589663,-2.84886775246144,65.61));
#55639=CARTESIAN_POINT('',(65.0704067589663,-2.84886775246144,65.61));
#55640=CARTESIAN_POINT('Origin',(66.8813246308841,-2.,65.61));
#55641=CARTESIAN_POINT('Origin',(66.8813246308841,-2.,69.61));
#55642=CARTESIAN_POINT('',(57.4252260922666,-2.50932065147687,69.61));
#55643=CARTESIAN_POINT('Origin',(56.338675369116,-2.,69.61));
#55644=CARTESIAN_POINT('',(58.7053050692247,-1.66334918565392,69.61));
#55645=CARTESIAN_POINT('',(59.11,-0.8,69.61));
#55646=CARTESIAN_POINT('',(60.0634934731631,-0.8,69.61));
#55647=CARTESIAN_POINT('Origin',(60.0634934731631,-2.3,69.61));
#55648=CARTESIAN_POINT('',(63.156506526837,-0.8,69.61));
#55649=CARTESIAN_POINT('',(59.11,-0.8,69.61));
#55650=CARTESIAN_POINT('',(64.5146949307753,-1.66334918565392,69.61));
#55651=CARTESIAN_POINT('Origin',(63.156506526837,-2.3,69.61));
#55652=CARTESIAN_POINT('',(64.11,-0.8,69.61));
#55653=CARTESIAN_POINT('',(65.7947739077334,-2.50932065147687,69.61));
#55654=CARTESIAN_POINT('Origin',(66.8813246308841,-2.,69.61));
#55655=CARTESIAN_POINT('',(65.2390620795424,-1.32380208466934,69.61));
#55656=CARTESIAN_POINT('',(64.8343671487671,-0.460452899015424,69.61));
#55657=CARTESIAN_POINT('',(63.156506526837,1.0842021724855E-16,69.61));
#55658=CARTESIAN_POINT('Origin',(63.156506526837,-2.3,69.61));
#55659=CARTESIAN_POINT('',(60.0634934731631,-4.33680868994202E-16,69.61));
#55660=CARTESIAN_POINT('',(59.11,1.0842021724855E-16,69.61));
#55661=CARTESIAN_POINT('',(57.9809379204577,-1.32380208466934,69.61));
#55662=CARTESIAN_POINT('Origin',(60.0634934731631,-2.3,69.61));
#55663=CARTESIAN_POINT('',(58.3856328512329,-0.460452899015424,69.61));
#55664=CARTESIAN_POINT('Origin',(59.11,-0.8,65.61));
#55665=CARTESIAN_POINT('',(65.7947739077334,-2.50932065147687,65.61));
#55666=CARTESIAN_POINT('Origin',(66.8813246308841,-2.,65.61));
#55667=CARTESIAN_POINT('',(64.5146949307753,-1.66334918565392,65.61));
#55668=CARTESIAN_POINT('',(64.11,-0.8,65.61));
#55669=CARTESIAN_POINT('',(63.156506526837,-0.8,65.61));
#55670=CARTESIAN_POINT('Origin',(63.156506526837,-2.3,65.61));
#55671=CARTESIAN_POINT('',(60.0634934731631,-0.8,65.61));
#55672=CARTESIAN_POINT('',(59.11,-0.8,65.61));
#55673=CARTESIAN_POINT('',(58.7053050692247,-1.66334918565392,65.61));
#55674=CARTESIAN_POINT('Origin',(60.0634934731631,-2.3,65.61));
#55675=CARTESIAN_POINT('',(59.11,-0.8,65.61));
#55676=CARTESIAN_POINT('',(57.4252260922666,-2.50932065147687,65.61));
#55677=CARTESIAN_POINT('Origin',(56.338675369116,-2.,65.61));
#55678=CARTESIAN_POINT('',(57.9809379204577,-1.32380208466934,65.61));
#55679=CARTESIAN_POINT('',(58.3856328512329,-0.460452899015424,65.61));
#55680=CARTESIAN_POINT('',(60.0634934731631,1.0842021724855E-16,65.61));
#55681=CARTESIAN_POINT('Origin',(60.0634934731631,-2.3,65.61));
#55682=CARTESIAN_POINT('',(63.156506526837,1.0842021724855E-16,65.61));
#55683=CARTESIAN_POINT('',(59.11,1.0842021724855E-16,65.61));
#55684=CARTESIAN_POINT('',(65.2390620795424,-1.32380208466934,65.61));
#55685=CARTESIAN_POINT('Origin',(63.156506526837,-2.3,65.61));
#55686=CARTESIAN_POINT('',(64.8343671487671,-0.460452899015424,65.61));
#55687=CARTESIAN_POINT('Origin',(60.0634934731631,-2.3,65.61));
#55688=CARTESIAN_POINT('',(60.0634934731631,-0.8,65.61));
#55689=CARTESIAN_POINT('',(58.7053050692247,-1.66334918565392,65.61));
#55690=CARTESIAN_POINT('Origin',(63.156506526837,-2.3,65.61));
#55691=CARTESIAN_POINT('',(64.5146949307753,-1.66334918565392,65.61));
#55692=CARTESIAN_POINT('',(63.156506526837,-0.8,65.61));
#55693=CARTESIAN_POINT('Origin',(59.11,-0.8,65.61));
#55694=CARTESIAN_POINT('Origin',(64.11,-0.8,65.61));
#55695=CARTESIAN_POINT('Origin',(59.11,-0.8,65.61));
#55696=CARTESIAN_POINT('Origin',(60.0634934731631,-2.3,65.61));
#55697=CARTESIAN_POINT('',(57.9809379204577,-1.32380208466934,65.61));
#55698=CARTESIAN_POINT('',(60.0634934731631,1.0842021724855E-16,65.61));
#55699=CARTESIAN_POINT('Origin',(63.156506526837,-2.3,65.61));
#55700=CARTESIAN_POINT('',(63.156506526837,1.0842021724855E-16,65.61));
#55701=CARTESIAN_POINT('',(65.2390620795424,-1.32380208466934,65.61));
#55702=CARTESIAN_POINT('Origin',(66.8813246308841,-2.,67.61));
#55703=CARTESIAN_POINT('',(65.7947739077334,-2.50932065147687,65.61));
#55704=CARTESIAN_POINT('Origin',(56.338675369116,-2.,65.61));
#55705=CARTESIAN_POINT('',(57.4252260922666,-2.50932065147687,65.61));
#55706=CARTESIAN_POINT('Origin',(58.3856328512329,-0.460452899015424,65.61));
#55707=CARTESIAN_POINT('Origin',(64.8343671487671,-0.460452899015424,65.61));
#55708=CARTESIAN_POINT('Origin',(59.11,1.0842021724855E-16,65.61));
#55709=CARTESIAN_POINT('Origin',(-48.39,-4.,65.61));
#55710=CARTESIAN_POINT('Origin',(-53.661324630884,-2.,65.61));
#55711=CARTESIAN_POINT('Origin',(-43.1186753691159,-2.,65.61));
#55712=CARTESIAN_POINT('Origin',(-48.39,-4.,69.61));
#55713=CARTESIAN_POINT('Origin',(-43.1186753691159,-2.,69.61));
#55714=CARTESIAN_POINT('Origin',(-53.661324630884,-2.,69.61));
#55715=CARTESIAN_POINT('Origin',(-53.661324630884,-2.,65.61));
#55716=CARTESIAN_POINT('',(-51.8504067589663,-2.84886775246144,65.61));
#55717=CARTESIAN_POINT('Origin',(-53.661324630884,-2.,65.61));
#55718=CARTESIAN_POINT('',(-51.8504067589663,-2.84886775246144,69.61));
#55719=CARTESIAN_POINT('',(-51.8504067589663,-2.84886775246144,65.61));
#55720=CARTESIAN_POINT('Origin',(-53.661324630884,-2.,69.61));
#55721=CARTESIAN_POINT('Origin',(-43.1186753691159,-2.,67.61));
#55722=CARTESIAN_POINT('',(-44.9295932410337,-2.84886775246144,69.61));
#55723=CARTESIAN_POINT('Origin',(-43.1186753691159,-2.,69.61));
#55724=CARTESIAN_POINT('',(-44.9295932410337,-2.84886775246144,65.61));
#55725=CARTESIAN_POINT('',(-44.9295932410337,-2.84886775246144,65.61));
#55726=CARTESIAN_POINT('Origin',(-43.1186753691159,-2.,65.61));
#55727=CARTESIAN_POINT('Origin',(-43.1186753691159,-2.,69.61));
#55728=CARTESIAN_POINT('',(-52.5747739077334,-2.50932065147687,69.61));
#55729=CARTESIAN_POINT('Origin',(-53.661324630884,-2.,69.61));
#55730=CARTESIAN_POINT('',(-51.2946949307753,-1.66334918565392,69.61));
#55731=CARTESIAN_POINT('',(-50.89,-0.8,69.61));
#55732=CARTESIAN_POINT('',(-49.9365065268369,-0.8,69.61));
#55733=CARTESIAN_POINT('Origin',(-49.9365065268369,-2.3,69.61));
#55734=CARTESIAN_POINT('',(-46.843493473163,-0.8,69.61));
#55735=CARTESIAN_POINT('',(-50.89,-0.8,69.61));
#55736=CARTESIAN_POINT('',(-45.4853050692247,-1.66334918565392,69.61));
#55737=CARTESIAN_POINT('Origin',(-46.843493473163,-2.3,69.61));
#55738=CARTESIAN_POINT('',(-45.89,-0.8,69.61));
#55739=CARTESIAN_POINT('',(-44.2052260922666,-2.50932065147687,69.61));
#55740=CARTESIAN_POINT('Origin',(-43.1186753691159,-2.,69.61));
#55741=CARTESIAN_POINT('',(-44.7609379204576,-1.32380208466934,69.61));
#55742=CARTESIAN_POINT('',(-45.1656328512329,-0.460452899015424,69.61));
#55743=CARTESIAN_POINT('',(-46.843493473163,1.0842021724855E-16,69.61));
#55744=CARTESIAN_POINT('Origin',(-46.843493473163,-2.3,69.61));
#55745=CARTESIAN_POINT('',(-49.9365065268369,-4.33680868994202E-16,69.61));
#55746=CARTESIAN_POINT('',(-50.89,1.0842021724855E-16,69.61));
#55747=CARTESIAN_POINT('',(-52.0190620795423,-1.32380208466934,69.61));
#55748=CARTESIAN_POINT('Origin',(-49.9365065268369,-2.3,69.61));
#55749=CARTESIAN_POINT('',(-51.6143671487671,-0.460452899015424,69.61));
#55750=CARTESIAN_POINT('Origin',(-50.89,-0.8,65.61));
#55751=CARTESIAN_POINT('',(-44.2052260922666,-2.50932065147686,65.61));
#55752=CARTESIAN_POINT('Origin',(-43.1186753691159,-2.,65.61));
#55753=CARTESIAN_POINT('',(-45.4853050692247,-1.66334918565392,65.61));
#55754=CARTESIAN_POINT('',(-45.89,-0.8,65.61));
#55755=CARTESIAN_POINT('',(-46.843493473163,-0.8,65.61));
#55756=CARTESIAN_POINT('Origin',(-46.843493473163,-2.3,65.61));
#55757=CARTESIAN_POINT('',(-49.9365065268369,-0.8,65.61));
#55758=CARTESIAN_POINT('',(-50.89,-0.8,65.61));
#55759=CARTESIAN_POINT('',(-51.2946949307753,-1.66334918565392,65.61));
#55760=CARTESIAN_POINT('Origin',(-49.9365065268369,-2.3,65.61));
#55761=CARTESIAN_POINT('',(-50.89,-0.8,65.61));
#55762=CARTESIAN_POINT('',(-52.5747739077334,-2.50932065147687,65.61));
#55763=CARTESIAN_POINT('Origin',(-53.661324630884,-2.,65.61));
#55764=CARTESIAN_POINT('',(-52.0190620795423,-1.32380208466934,65.61));
#55765=CARTESIAN_POINT('',(-51.6143671487671,-0.460452899015424,65.61));
#55766=CARTESIAN_POINT('',(-49.9365065268369,1.0842021724855E-16,65.61));
#55767=CARTESIAN_POINT('Origin',(-49.9365065268369,-2.3,65.61));
#55768=CARTESIAN_POINT('',(-46.843493473163,1.0842021724855E-16,65.61));
#55769=CARTESIAN_POINT('',(-50.89,1.0842021724855E-16,65.61));
#55770=CARTESIAN_POINT('',(-44.7609379204576,-1.32380208466934,65.61));
#55771=CARTESIAN_POINT('Origin',(-46.843493473163,-2.3,65.61));
#55772=CARTESIAN_POINT('',(-45.1656328512329,-0.460452899015424,65.61));
#55773=CARTESIAN_POINT('Origin',(-49.9365065268369,-2.3,65.61));
#55774=CARTESIAN_POINT('',(-49.9365065268369,-0.8,65.61));
#55775=CARTESIAN_POINT('',(-51.2946949307753,-1.66334918565392,65.61));
#55776=CARTESIAN_POINT('Origin',(-46.843493473163,-2.3,65.61));
#55777=CARTESIAN_POINT('',(-45.4853050692247,-1.66334918565392,65.61));
#55778=CARTESIAN_POINT('',(-46.843493473163,-0.8,65.61));
#55779=CARTESIAN_POINT('Origin',(-50.89,-0.8,65.61));
#55780=CARTESIAN_POINT('Origin',(-45.89,-0.8,65.61));
#55781=CARTESIAN_POINT('Origin',(-50.89,-0.8,65.61));
#55782=CARTESIAN_POINT('Origin',(-49.9365065268369,-2.3,65.61));
#55783=CARTESIAN_POINT('',(-52.0190620795423,-1.32380208466934,65.61));
#55784=CARTESIAN_POINT('',(-49.9365065268369,1.0842021724855E-16,65.61));
#55785=CARTESIAN_POINT('Origin',(-46.843493473163,-2.3,65.61));
#55786=CARTESIAN_POINT('',(-46.843493473163,1.0842021724855E-16,65.61));
#55787=CARTESIAN_POINT('',(-44.7609379204576,-1.32380208466934,65.61));
#55788=CARTESIAN_POINT('Origin',(-43.1186753691159,-2.,67.61));
#55789=CARTESIAN_POINT('',(-44.2052260922666,-2.50932065147687,65.61));
#55790=CARTESIAN_POINT('Origin',(-53.661324630884,-2.,65.61));
#55791=CARTESIAN_POINT('',(-52.5747739077334,-2.50932065147687,65.61));
#55792=CARTESIAN_POINT('Origin',(-51.6143671487671,-0.460452899015424,65.61));
#55793=CARTESIAN_POINT('Origin',(-45.1656328512329,-0.460452899015424,65.61));
#55794=CARTESIAN_POINT('Origin',(-50.89,1.0842021724855E-16,65.61));
#55795=CARTESIAN_POINT('Origin',(-48.39,-4.,-68.39));
#55796=CARTESIAN_POINT('Origin',(-53.661324630884,-2.,-68.39));
#55797=CARTESIAN_POINT('Origin',(-43.1186753691159,-2.,-68.39));
#55798=CARTESIAN_POINT('Origin',(-48.39,-4.,-64.39));
#55799=CARTESIAN_POINT('Origin',(-43.1186753691159,-2.,-64.39));
#55800=CARTESIAN_POINT('Origin',(-53.661324630884,-2.,-64.39));
#55801=CARTESIAN_POINT('Origin',(-53.661324630884,-2.,-68.39));
#55802=CARTESIAN_POINT('',(-51.8504067589663,-2.84886775246144,-68.39));
#55803=CARTESIAN_POINT('Origin',(-53.661324630884,-2.,-68.39));
#55804=CARTESIAN_POINT('',(-51.8504067589663,-2.84886775246144,-64.39));
#55805=CARTESIAN_POINT('',(-51.8504067589663,-2.84886775246144,-68.39));
#55806=CARTESIAN_POINT('Origin',(-53.661324630884,-2.,-64.39));
#55807=CARTESIAN_POINT('Origin',(-43.1186753691159,-2.,-66.39));
#55808=CARTESIAN_POINT('',(-44.9295932410337,-2.84886775246144,-64.39));
#55809=CARTESIAN_POINT('Origin',(-43.1186753691159,-2.,-64.39));
#55810=CARTESIAN_POINT('',(-44.9295932410337,-2.84886775246144,-68.39));
#55811=CARTESIAN_POINT('',(-44.9295932410337,-2.84886775246144,-68.39));
#55812=CARTESIAN_POINT('Origin',(-43.1186753691159,-2.,-68.39));
#55813=CARTESIAN_POINT('Origin',(-43.1186753691159,-2.,-64.39));
#55814=CARTESIAN_POINT('',(-52.5747739077334,-2.50932065147687,-64.39));
#55815=CARTESIAN_POINT('Origin',(-53.661324630884,-2.,-64.39));
#55816=CARTESIAN_POINT('',(-51.2946949307753,-1.66334918565392,-64.39));
#55817=CARTESIAN_POINT('',(-50.89,-0.8,-64.39));
#55818=CARTESIAN_POINT('',(-49.936506526837,-0.8,-64.39));
#55819=CARTESIAN_POINT('Origin',(-49.936506526837,-2.3,-64.39));
#55820=CARTESIAN_POINT('',(-46.843493473163,-0.8,-64.39));
#55821=CARTESIAN_POINT('',(-50.89,-0.8,-64.39));
#55822=CARTESIAN_POINT('',(-45.4853050692247,-1.66334918565392,-64.39));
#55823=CARTESIAN_POINT('Origin',(-46.843493473163,-2.3,-64.39));
#55824=CARTESIAN_POINT('',(-45.89,-0.8,-64.39));
#55825=CARTESIAN_POINT('',(-44.2052260922666,-2.50932065147687,-64.39));
#55826=CARTESIAN_POINT('Origin',(-43.1186753691159,-2.,-64.39));
#55827=CARTESIAN_POINT('',(-44.7609379204576,-1.32380208466934,-64.39));
#55828=CARTESIAN_POINT('',(-45.1656328512329,-0.460452899015424,-64.39));
#55829=CARTESIAN_POINT('',(-46.843493473163,1.0842021724855E-16,-64.39));
#55830=CARTESIAN_POINT('Origin',(-46.843493473163,-2.3,-64.39));
#55831=CARTESIAN_POINT('',(-49.936506526837,-4.33680868994202E-16,-64.39));
#55832=CARTESIAN_POINT('',(-50.89,1.0842021724855E-16,-64.39));
#55833=CARTESIAN_POINT('',(-52.0190620795423,-1.32380208466934,-64.39));
#55834=CARTESIAN_POINT('Origin',(-49.936506526837,-2.3,-64.39));
#55835=CARTESIAN_POINT('',(-51.6143671487671,-0.460452899015424,-64.39));
#55836=CARTESIAN_POINT('Origin',(-50.89,-0.8,-68.39));
#55837=CARTESIAN_POINT('',(-44.2052260922666,-2.50932065147686,-68.39));
#55838=CARTESIAN_POINT('Origin',(-43.1186753691159,-2.,-68.39));
#55839=CARTESIAN_POINT('',(-45.4853050692247,-1.66334918565392,-68.39));
#55840=CARTESIAN_POINT('',(-45.89,-0.8,-68.39));
#55841=CARTESIAN_POINT('',(-46.843493473163,-0.8,-68.39));
#55842=CARTESIAN_POINT('Origin',(-46.843493473163,-2.3,-68.39));
#55843=CARTESIAN_POINT('',(-49.936506526837,-0.8,-68.39));
#55844=CARTESIAN_POINT('',(-50.89,-0.8,-68.39));
#55845=CARTESIAN_POINT('',(-51.2946949307753,-1.66334918565392,-68.39));
#55846=CARTESIAN_POINT('Origin',(-49.936506526837,-2.3,-68.39));
#55847=CARTESIAN_POINT('',(-50.89,-0.8,-68.39));
#55848=CARTESIAN_POINT('',(-52.5747739077334,-2.50932065147687,-68.39));
#55849=CARTESIAN_POINT('Origin',(-53.661324630884,-2.,-68.39));
#55850=CARTESIAN_POINT('',(-52.0190620795423,-1.32380208466934,-68.39));
#55851=CARTESIAN_POINT('',(-51.6143671487671,-0.460452899015424,-68.39));
#55852=CARTESIAN_POINT('',(-49.936506526837,1.0842021724855E-16,-68.39));
#55853=CARTESIAN_POINT('Origin',(-49.936506526837,-2.3,-68.39));
#55854=CARTESIAN_POINT('',(-46.843493473163,1.0842021724855E-16,-68.39));
#55855=CARTESIAN_POINT('',(-50.89,1.0842021724855E-16,-68.39));
#55856=CARTESIAN_POINT('',(-44.7609379204576,-1.32380208466934,-68.39));
#55857=CARTESIAN_POINT('Origin',(-46.843493473163,-2.3,-68.39));
#55858=CARTESIAN_POINT('',(-45.1656328512329,-0.460452899015424,-68.39));
#55859=CARTESIAN_POINT('Origin',(-49.936506526837,-2.3,-68.39));
#55860=CARTESIAN_POINT('',(-49.936506526837,-0.8,-68.39));
#55861=CARTESIAN_POINT('',(-51.2946949307753,-1.66334918565392,-68.39));
#55862=CARTESIAN_POINT('Origin',(-46.843493473163,-2.3,-68.39));
#55863=CARTESIAN_POINT('',(-45.4853050692247,-1.66334918565392,-68.39));
#55864=CARTESIAN_POINT('',(-46.843493473163,-0.8,-68.39));
#55865=CARTESIAN_POINT('Origin',(-50.89,-0.8,-68.39));
#55866=CARTESIAN_POINT('Origin',(-45.89,-0.8,-68.39));
#55867=CARTESIAN_POINT('Origin',(-50.89,-0.8,-68.39));
#55868=CARTESIAN_POINT('Origin',(-49.936506526837,-2.3,-68.39));
#55869=CARTESIAN_POINT('',(-52.0190620795423,-1.32380208466934,-68.39));
#55870=CARTESIAN_POINT('',(-49.936506526837,1.0842021724855E-16,-68.39));
#55871=CARTESIAN_POINT('Origin',(-46.843493473163,-2.3,-68.39));
#55872=CARTESIAN_POINT('',(-46.843493473163,1.0842021724855E-16,-68.39));
#55873=CARTESIAN_POINT('',(-44.7609379204576,-1.32380208466934,-68.39));
#55874=CARTESIAN_POINT('Origin',(-43.1186753691159,-2.,-66.39));
#55875=CARTESIAN_POINT('',(-44.2052260922666,-2.50932065147687,-68.39));
#55876=CARTESIAN_POINT('Origin',(-53.661324630884,-2.,-68.39));
#55877=CARTESIAN_POINT('',(-52.5747739077334,-2.50932065147687,-68.39));
#55878=CARTESIAN_POINT('Origin',(-51.6143671487671,-0.460452899015424,-68.39));
#55879=CARTESIAN_POINT('Origin',(-45.1656328512329,-0.460452899015424,-68.39));
#55880=CARTESIAN_POINT('Origin',(-50.89,1.0842021724855E-16,-68.39));
#55881=CARTESIAN_POINT('Origin',(-86.39,44.5787611019615,-30.));
#55882=CARTESIAN_POINT('Ctrl Pts',(-86.39,44.5787611019615,-12.5));
#55883=CARTESIAN_POINT('Ctrl Pts',(-86.39,43.433398281725,-12.5));
#55884=CARTESIAN_POINT('Ctrl Pts',(-86.3900000000003,41.4793849623337,-12.6924535140054));
#55885=CARTESIAN_POINT('Ctrl Pts',(-86.3900000000001,39.5894256066326,-13.2069280492973));
#55886=CARTESIAN_POINT('Ctrl Pts',(-86.3900000000001,38.8257009252949,-13.4727301229578));
#55887=CARTESIAN_POINT('Origin',(-86.39,42.6698984466481,-20.6937528963263));
#55888=CARTESIAN_POINT('',(-86.39,46.1862026520568,-22.1631559439119));
#55889=CARTESIAN_POINT('Ctrl Pts',(-86.39,44.5787611019615,-22.));
#55890=CARTESIAN_POINT('Ctrl Pts',(-86.39,45.1023555340697,-22.));
#55891=CARTESIAN_POINT('Ctrl Pts',(-86.39,45.6259499661778,-22.0515695504083));
#55892=CARTESIAN_POINT('Ctrl Pts',(-86.3899999999998,46.1394836780905,-22.1537177567742));
#55893=CARTESIAN_POINT('Ctrl Pts',(-86.3899999999998,46.1550660227812,-22.1568172778459));
#55894=CARTESIAN_POINT('Ctrl Pts',(-86.3899999999998,46.1706391043629,-22.1599633677105));
#55895=CARTESIAN_POINT('Ctrl Pts',(-86.3899999999998,46.1862026525634,-22.1631559443817));
#55896=CARTESIAN_POINT('',(-86.39,47.7866618629516,-21.4437528963263));
#55897=CARTESIAN_POINT('Origin',(-86.39,46.487623757275,-20.6937528963263));
#55898=CARTESIAN_POINT('',(-86.39,51.1378158375422,-15.6393839483491));
#55899=CARTESIAN_POINT('',(-86.39,43.2797229962849,-29.25));
#55900=CARTESIAN_POINT('Origin',(-86.39,49.8387777318655,-14.8893839483491));
#55901=CARTESIAN_POINT('',(-86.39,61.7683968696973,-26.7187856671455));
#55902=CARTESIAN_POINT('',(-86.39,56.0151454716109,-16.7539809986688));
#55903=CARTESIAN_POINT('Ctrl Pts',(-86.39,61.7683968689589,-26.7187856673309));
#55904=CARTESIAN_POINT('Ctrl Pts',(-86.39,61.7599375519114,-26.674463640704));
#55905=CARTESIAN_POINT('Ctrl Pts',(-86.3900000000001,61.5322159292861,-25.5059524219446));
#55906=CARTESIAN_POINT('Ctrl Pts',(-86.3900000000002,60.8508742849282,-23.2598700311452));
#55907=CARTESIAN_POINT('Ctrl Pts',(-86.39,59.2232760668162,-20.2148479377946));
#55908=CARTESIAN_POINT('Ctrl Pts',(-86.39,57.4908812316947,-18.1039187234887));
#55909=CARTESIAN_POINT('Ctrl Pts',(-86.3900000000001,56.3382988733641,-17.0329646666082));
#55910=CARTESIAN_POINT('Ctrl Pts',(-86.3900000000001,56.015145471611,-16.7539809986688));
#55911=CARTESIAN_POINT('',(-86.39,53.7358855886589,-17.139395137807));
#55912=CARTESIAN_POINT('Origin',(-86.39,55.0349236943356,-17.889395137807));
#55913=CARTESIAN_POINT('',(-86.39,45.8777992076382,-30.75));
#55914=CARTESIAN_POINT('',(-86.3899999999998,52.1693515295639,-27.4736373074919));
#55915=CARTESIAN_POINT('Ctrl Pts',(-86.3899999999997,50.5618748736091,-24.6894451446548));
#55916=CARTESIAN_POINT('Ctrl Pts',(-86.3899999999997,50.8041422375712,-24.9624237973974));
#55917=CARTESIAN_POINT('Ctrl Pts',(-86.3899999999996,51.3485297861136,-25.6673520933051));
#55918=CARTESIAN_POINT('Ctrl Pts',(-86.3899999999995,51.8596181789187,-26.6235312230362));
#55919=CARTESIAN_POINT('Ctrl Pts',(-86.3899999999996,52.1092282227056,-27.2929693864679));
#55920=CARTESIAN_POINT('Ctrl Pts',(-86.3899999999996,52.1693515272627,-27.4736373005769));
#55921=CARTESIAN_POINT('',(-86.39,53.5926110635042,-28.5));
#55922=CARTESIAN_POINT('Origin',(-86.39,53.5926110635042,-27.));
#55923=CARTESIAN_POINT('',(-86.39,60.2949931567668,-28.5));
#55924=CARTESIAN_POINT('',(-86.39,-3.78600659594871E-14,-28.5));
#55925=CARTESIAN_POINT('Origin',(-86.39,60.2949931567668,-27.));
#55926=CARTESIAN_POINT('',(-86.39,56.0151454719897,-43.2460190010043));
#55927=CARTESIAN_POINT('',(-86.39,61.7683968694786,-33.2812143329271));
#55928=CARTESIAN_POINT('Ctrl Pts',(-86.3900000000001,56.0151454719897,-43.2460190010042));
#55929=CARTESIAN_POINT('Ctrl Pts',(-86.3900000000001,56.3382988733641,-42.9670353333918));
#55930=CARTESIAN_POINT('Ctrl Pts',(-86.39,57.4908812316947,-41.8960812765113));
#55931=CARTESIAN_POINT('Ctrl Pts',(-86.3899999999999,59.2232760668162,-39.7851520622054));
#55932=CARTESIAN_POINT('Ctrl Pts',(-86.3899999999999,60.8508742849283,-36.7401299688548));
#55933=CARTESIAN_POINT('Ctrl Pts',(-86.3900000000002,61.5322159292861,-34.4940475780554));
#55934=CARTESIAN_POINT('Ctrl Pts',(-86.3900000000002,61.7599375519114,-33.325536359296));
#55935=CARTESIAN_POINT('Ctrl Pts',(-86.3900000000002,61.7683968689589,-33.2812143326691));
#55936=CARTESIAN_POINT('',(-86.39,60.2949931567668,-31.5));
#55937=CARTESIAN_POINT('Origin',(-86.39,60.2949931567668,-33.));
#55938=CARTESIAN_POINT('',(-86.39,53.5926110635042,-31.5));
#55939=CARTESIAN_POINT('',(-86.39,-3.78600659594871E-14,-31.5));
#55940=CARTESIAN_POINT('',(-86.3899999999999,52.1693515289861,-32.5263626942444));
#55941=CARTESIAN_POINT('Origin',(-86.39,53.5926110635042,-32.9999999999999));
#55942=CARTESIAN_POINT('Ctrl Pts',(-86.3899999999998,52.1693515261484,-32.5263627027716));
#55943=CARTESIAN_POINT('Ctrl Pts',(-86.3899999999998,52.1092282218831,-32.7070306157379));
#55944=CARTESIAN_POINT('Ctrl Pts',(-86.3899999999998,51.8596181783615,-33.3764687780062));
#55945=CARTESIAN_POINT('Ctrl Pts',(-86.39,51.3485297861136,-34.3326479066949));
#55946=CARTESIAN_POINT('Ctrl Pts',(-86.3899999999998,50.8041422375712,-35.0375762026026));
#55947=CARTESIAN_POINT('Ctrl Pts',(-86.3899999999998,50.5618748736091,-35.3105548553452));
#55948=CARTESIAN_POINT('',(-86.39,53.7358855886589,-42.860604862193));
#55949=CARTESIAN_POINT('',(-86.39,45.8777992076382,-29.25));
#55950=CARTESIAN_POINT('Origin',(-86.39,55.0349236943356,-42.110604862193));
#55951=CARTESIAN_POINT('',(-86.39,50.3318212777197,-46.5272698779464));
#55952=CARTESIAN_POINT('Ctrl Pts',(-86.39,38.825700926836,-46.5272698775785));
#55953=CARTESIAN_POINT('Ctrl Pts',(-86.3900000000001,39.5894256076847,-46.7930719509892));
#55954=CARTESIAN_POINT('Ctrl Pts',(-86.3900000000002,41.4793849628776,-47.3075464860481));
#55955=CARTESIAN_POINT('Ctrl Pts',(-86.39,44.5787611019615,-47.6128083915182));
#55956=CARTESIAN_POINT('Ctrl Pts',(-86.3900000000003,47.6781372410454,-47.3075464860481));
#55957=CARTESIAN_POINT('Ctrl Pts',(-86.3900000000001,49.5680965962383,-46.7930719509892));
#55958=CARTESIAN_POINT('Ctrl Pts',(-86.39,50.331821277087,-46.5272698775786));
#55959=CARTESIAN_POINT('',(-86.39,51.1378158375422,-44.3606160516509));
#55960=CARTESIAN_POINT('Origin',(-86.39,49.8387777318655,-45.1106160516509));
#55961=CARTESIAN_POINT('',(-86.39,47.7866618629516,-38.5562471036737));
#55962=CARTESIAN_POINT('',(-86.39,43.2797229962849,-30.75));
#55963=CARTESIAN_POINT('',(-86.39,46.1862026523886,-37.8368440547629));
#55964=CARTESIAN_POINT('Origin',(-86.39,46.4876237572749,-39.3062471036737));
#55965=CARTESIAN_POINT('',(-86.39,42.9713195518663,-37.8368440560881));
#55966=CARTESIAN_POINT('Ctrl Pts',(-86.3899999999997,46.1862026525626,-37.8368440556185));
#55967=CARTESIAN_POINT('Ctrl Pts',(-86.3899999999997,46.1706391043624,-37.8400366322896));
#55968=CARTESIAN_POINT('Ctrl Pts',(-86.3899999999996,45.6418375870482,-37.9468656555161));
#55969=CARTESIAN_POINT('Ctrl Pts',(-86.3899999999997,44.5787611019615,-38.0515695504083));
#55970=CARTESIAN_POINT('Ctrl Pts',(-86.3899999999996,43.5156846168748,-37.9468656555161));
#55971=CARTESIAN_POINT('Ctrl Pts',(-86.3899999999997,42.9868830995607,-37.8400366322896));
#55972=CARTESIAN_POINT('Ctrl Pts',(-86.3899999999997,42.971319551943,-37.836844055738));
#55973=CARTESIAN_POINT('',(-86.39,41.3708603409714,-38.5562471036737));
#55974=CARTESIAN_POINT('Origin',(-86.39,42.6698984466481,-39.3062471036737));
#55975=CARTESIAN_POINT('',(-86.39,45.8777992076382,-30.75));
#55976=CARTESIAN_POINT('',(-86.39,33.1423767323121,-43.2460190013313));
#55977=CARTESIAN_POINT('Ctrl Pts',(-86.3900000000001,27.3891253349641,-33.281214332669));
#55978=CARTESIAN_POINT('Ctrl Pts',(-86.3900000000001,27.3975846520116,-33.3255363592959));
#55979=CARTESIAN_POINT('Ctrl Pts',(-86.3900000000001,27.6253062746369,-34.4940475780554));
#55980=CARTESIAN_POINT('Ctrl Pts',(-86.39,28.3066479189948,-36.7401299688549));
#55981=CARTESIAN_POINT('Ctrl Pts',(-86.39,29.9342461371069,-39.7851520622054));
#55982=CARTESIAN_POINT('Ctrl Pts',(-86.3900000000001,31.6666409722284,-41.8960812765113));
#55983=CARTESIAN_POINT('Ctrl Pts',(-86.3900000000001,32.8192233305589,-42.9670353333918));
#55984=CARTESIAN_POINT('Ctrl Pts',(-86.3900000000001,33.1423767323121,-43.2460190013313));
#55985=CARTESIAN_POINT('',(-86.39,35.4216366152641,-42.860604862193));
#55986=CARTESIAN_POINT('Origin',(-86.39,34.1225985095874,-42.110604862193));
#55987=CARTESIAN_POINT('',(-86.39,38.7727956517265,-37.0562271467965));
#55988=CARTESIAN_POINT('',(-86.39,43.2797229962849,-29.25));
#55989=CARTESIAN_POINT('',(-86.39,38.5956473299119,-35.3105548561393));
#55990=CARTESIAN_POINT('Origin',(-86.39,37.4737575460498,-36.3062271467965));
#55991=CARTESIAN_POINT('',(-86.3899999999999,36.9881706743592,-32.5263626925082));
#55992=CARTESIAN_POINT('Ctrl Pts',(-86.3899999999998,38.5956473303139,-35.3105548553452));
#55993=CARTESIAN_POINT('Ctrl Pts',(-86.3899999999998,38.3533799663518,-35.0375762026026));
#55994=CARTESIAN_POINT('Ctrl Pts',(-86.3899999999997,37.8089924178094,-34.3326479066949));
#55995=CARTESIAN_POINT('Ctrl Pts',(-86.3899999999999,37.2979040250044,-33.3764687769638));
#55996=CARTESIAN_POINT('Ctrl Pts',(-86.3899999999999,37.0482939812175,-32.7070306135321));
#55997=CARTESIAN_POINT('Ctrl Pts',(-86.3899999999998,36.9881706766604,-32.5263626994232));
#55998=CARTESIAN_POINT('',(-86.39,35.5649111404189,-31.5));
#55999=CARTESIAN_POINT('Origin',(-86.39,35.5649111404189,-33.));
#56000=CARTESIAN_POINT('',(-86.39,-3.78600659594871E-14,-31.5));
#56001=CARTESIAN_POINT('',(-86.39,33.1423767319333,-16.7539809989958));
#56002=CARTESIAN_POINT('Ctrl Pts',(-86.3900000000001,33.1423767319333,-16.7539809989958));
#56003=CARTESIAN_POINT('Ctrl Pts',(-86.3900000000001,32.819223330559,-17.0329646666082));
#56004=CARTESIAN_POINT('Ctrl Pts',(-86.3900000000001,31.6666409722284,-18.1039187234887));
#56005=CARTESIAN_POINT('Ctrl Pts',(-86.3899999999999,29.9342461371069,-20.2148479377946));
#56006=CARTESIAN_POINT('Ctrl Pts',(-86.3900000000004,28.3066479189948,-23.2598700311452));
#56007=CARTESIAN_POINT('Ctrl Pts',(-86.3900000000002,27.6253062746369,-25.5059524219446));
#56008=CARTESIAN_POINT('Ctrl Pts',(-86.3900000000002,27.3975846520116,-26.674463640704));
#56009=CARTESIAN_POINT('Ctrl Pts',(-86.3900000000002,27.3891253349641,-26.7187856673309));
#56010=CARTESIAN_POINT('',(-86.39,35.5649111404189,-28.5));
#56011=CARTESIAN_POINT('',(-86.39,-3.78600659594871E-14,-28.5));
#56012=CARTESIAN_POINT('',(-86.3899999999999,36.988170674937,-27.4736373057556));
#56013=CARTESIAN_POINT('Origin',(-86.39,35.5649111404189,-27.));
#56014=CARTESIAN_POINT('',(-86.39,38.5956473300202,-24.6894451439698));
#56015=CARTESIAN_POINT('Ctrl Pts',(-86.3899999999998,36.9881706777747,-27.4736372972284));
#56016=CARTESIAN_POINT('Ctrl Pts',(-86.3899999999998,37.0482939820399,-27.2929693842621));
#56017=CARTESIAN_POINT('Ctrl Pts',(-86.3899999999999,37.2979040255616,-26.6235312219938));
#56018=CARTESIAN_POINT('Ctrl Pts',(-86.3899999999997,37.8089924178094,-25.6673520933051));
#56019=CARTESIAN_POINT('Ctrl Pts',(-86.3899999999998,38.3533799663518,-24.9624237973974));
#56020=CARTESIAN_POINT('Ctrl Pts',(-86.3899999999998,38.5956473303139,-24.6894451446548));
#56021=CARTESIAN_POINT('',(-86.39,38.7727956517265,-22.9437728532035));
#56022=CARTESIAN_POINT('Origin',(-86.39,37.4737575460499,-23.6937728532035));
#56023=CARTESIAN_POINT('',(-86.39,35.4216366152641,-17.139395137807));
#56024=CARTESIAN_POINT('',(-86.39,43.2797229962849,-30.75));
#56025=CARTESIAN_POINT('Origin',(-86.39,34.1225985095875,-17.889395137807));
#56026=CARTESIAN_POINT('Ctrl Pts',(-86.39,44.5787611019615,-0.5));
#56027=CARTESIAN_POINT('Ctrl Pts',(-86.39,42.6480066335628,-0.5));
#56028=CARTESIAN_POINT('Ctrl Pts',(-86.3899999999995,38.7864976967653,-0.880325434261422));
#56029=CARTESIAN_POINT('Ctrl Pts',(-86.3899999999997,34.8506764348762,-2.07424376132674));
#56030=CARTESIAN_POINT('Ctrl Pts',(-86.3899999999997,32.8626902557638,-2.92534739713908));
#56031=CARTESIAN_POINT('Ctrl Pts',(-86.3899999999997,32.6508629759047,-3.01900602948033));
#56032=CARTESIAN_POINT('Origin',(-86.39,36.2795905006212,-9.62541485779656));
#56033=CARTESIAN_POINT('',(-86.39,52.3121016231526,-11.0146003449218));
#56034=CARTESIAN_POINT('Ctrl Pts',(-86.39,44.5787611019615,-9.5));
#56035=CARTESIAN_POINT('Ctrl Pts',(-86.39,45.9204718342386,-9.5));
#56036=CARTESIAN_POINT('Ctrl Pts',(-86.3899999999998,48.5636521071579,-9.76033053440579));
#56037=CARTESIAN_POINT('Ctrl Pts',(-86.39,51.1067797000701,-10.5236598583039));
#56038=CARTESIAN_POINT('Ctrl Pts',(-86.3900000000001,52.3121016228057,-11.0146003457735));
#56039=CARTESIAN_POINT('Origin',(-86.39,52.8779317033019,-9.62541485779658));
#56040=CARTESIAN_POINT('Origin',(-86.39,55.9000854795073,-4.39089096912261));
#56041=CARTESIAN_POINT('',(-86.39,73.9088368631419,-26.8393082747607));
#56042=CARTESIAN_POINT('',(-86.39,61.981165935949,-6.17977240953646));
#56043=CARTESIAN_POINT('Ctrl Pts',(-86.3899999999997,73.9088368640174,-26.839308274661));
#56044=CARTESIAN_POINT('Ctrl Pts',(-86.3899999999997,73.8150807723753,-25.9691649995626));
#56045=CARTESIAN_POINT('Ctrl Pts',(-86.3899999999998,73.3905329456444,-23.1927173488564));
#56046=CARTESIAN_POINT('Ctrl Pts',(-86.3899999999996,72.0088947532483,-18.6380666239304));
#56047=CARTESIAN_POINT('Ctrl Pts',(-86.3899999999996,69.2652291855737,-13.5050293808538));
#56048=CARTESIAN_POINT('Ctrl Pts',(-86.3899999999999,65.8355371052309,-9.3259374892749));
#56049=CARTESIAN_POINT('Ctrl Pts',(-86.3899999999998,63.2074283898883,-7.07576138751773));
#56050=CARTESIAN_POINT('Ctrl Pts',(-86.3899999999997,61.981165935513,-6.17977241013897));
#56051=CARTESIAN_POINT('Origin',(-86.39,61.0962221090323,-7.39091832371568));
#56052=CARTESIAN_POINT('',(-86.39,64.8871997647975,-27.2044726114797));
#56053=CARTESIAN_POINT('Ctrl Pts',(-86.39,57.1538693431349,-13.8100697594034));
#56054=CARTESIAN_POINT('Ctrl Pts',(-86.39,57.8284952042209,-14.3341115102115));
#56055=CARTESIAN_POINT('Ctrl Pts',(-86.3899999999999,59.4786368856762,-15.7895125368886));
#56056=CARTESIAN_POINT('Ctrl Pts',(-86.3899999999999,61.7337643465056,-18.5373932985594));
#56057=CARTESIAN_POINT('Ctrl Pts',(-86.3899999999998,63.6403794020083,-22.1044191793415));
#56058=CARTESIAN_POINT('Ctrl Pts',(-86.3899999999998,64.5418111191123,-25.076041306158));
#56059=CARTESIAN_POINT('Ctrl Pts',(-86.3899999999999,64.8317241957022,-26.801305653953));
#56060=CARTESIAN_POINT('Ctrl Pts',(-86.3899999999999,64.8871997647975,-27.2044726114797));
#56061=CARTESIAN_POINT('Origin',(-86.39,66.3731980659926,-27.));
#56062=CARTESIAN_POINT('Origin',(-86.39,72.4174689786827,-27.));
#56063=CARTESIAN_POINT('',(-86.39,61.9811659358818,-53.8202275903908));
#56064=CARTESIAN_POINT('',(-86.39,73.9088368645467,-33.1606917253857));
#56065=CARTESIAN_POINT('Ctrl Pts',(-86.3899999999998,61.981165935513,-53.820227589861));
#56066=CARTESIAN_POINT('Ctrl Pts',(-86.3899999999997,63.2074283898883,-52.9242386124823));
#56067=CARTESIAN_POINT('Ctrl Pts',(-86.3899999999997,65.8355371052309,-50.6740625107251));
#56068=CARTESIAN_POINT('Ctrl Pts',(-86.3899999999997,69.2652291855737,-46.4949706191462));
#56069=CARTESIAN_POINT('Ctrl Pts',(-86.39,72.0088947532483,-41.3619333760696));
#56070=CARTESIAN_POINT('Ctrl Pts',(-86.3899999999997,73.3905329456444,-36.8072826511436));
#56071=CARTESIAN_POINT('Ctrl Pts',(-86.3899999999996,73.8150807723754,-34.0308350004374));
#56072=CARTESIAN_POINT('Ctrl Pts',(-86.3899999999996,73.9088368640174,-33.1606917253389));
#56073=CARTESIAN_POINT('Origin',(-86.39,72.4174689786827,-33.));
#56074=CARTESIAN_POINT('',(-86.39,64.8871997648004,-32.7955273884995));
#56075=CARTESIAN_POINT('Origin',(-86.39,66.3731980659926,-33.));
#56076=CARTESIAN_POINT('Ctrl Pts',(-86.39,64.8871997648004,-32.7955273884995));
#56077=CARTESIAN_POINT('Ctrl Pts',(-86.39,64.8317241957022,-33.198694346047));
#56078=CARTESIAN_POINT('Ctrl Pts',(-86.3899999999999,64.5418111191122,-34.923958693842));
#56079=CARTESIAN_POINT('Ctrl Pts',(-86.3899999999999,63.6403794020083,-37.8955808206585));
#56080=CARTESIAN_POINT('Ctrl Pts',(-86.39,61.7337643465056,-41.4626067014406));
#56081=CARTESIAN_POINT('Ctrl Pts',(-86.39,59.4786368856762,-44.2104874631114));
#56082=CARTESIAN_POINT('Ctrl Pts',(-86.3899999999999,57.8284952042209,-45.6658884897885));
#56083=CARTESIAN_POINT('Ctrl Pts',(-86.3899999999999,57.1538693431349,-46.1899302405967));
#56084=CARTESIAN_POINT('Origin',(-86.39,61.0962221090322,-52.6090816762843));
#56085=CARTESIAN_POINT('',(-86.39,56.5066592283165,-56.9809939712271));
#56086=CARTESIAN_POINT('Ctrl Pts',(-86.3899999999997,32.6508629759048,-56.9809939705197));
#56087=CARTESIAN_POINT('Ctrl Pts',(-86.3899999999997,32.8626902557639,-57.074652602861));
#56088=CARTESIAN_POINT('Ctrl Pts',(-86.3899999999997,34.8506764348762,-57.9257562386733));
#56089=CARTESIAN_POINT('Ctrl Pts',(-86.39,38.7864976967653,-59.1196745657386));
#56090=CARTESIAN_POINT('Ctrl Pts',(-86.3899999999997,44.5787611019615,-59.6901627171307));
#56091=CARTESIAN_POINT('Ctrl Pts',(-86.3899999999998,50.3710245071578,-59.1196745657386));
#56092=CARTESIAN_POINT('Ctrl Pts',(-86.3899999999999,54.3068457690469,-57.9257562386733));
#56093=CARTESIAN_POINT('Ctrl Pts',(-86.3899999999999,56.2948319481591,-57.0746526028609));
#56094=CARTESIAN_POINT('Ctrl Pts',(-86.3899999999999,56.5066592280182,-56.9809939705197));
#56095=CARTESIAN_POINT('Origin',(-86.39,55.9000854795073,-55.6091090308774));
#56096=CARTESIAN_POINT('',(-86.39,52.3121016229798,-48.9853996547525));
#56097=CARTESIAN_POINT('Origin',(-86.39,52.8779317033019,-50.3745851422034));
#56098=CARTESIAN_POINT('',(-86.39,36.8454205808236,-48.9853996550999));
#56099=CARTESIAN_POINT('Ctrl Pts',(-86.3899999999999,52.3121016227473,-48.9853996542503));
#56100=CARTESIAN_POINT('Ctrl Pts',(-86.39,51.1067797000296,-49.4763401417082));
#56101=CARTESIAN_POINT('Ctrl Pts',(-86.39,48.5636521071369,-50.2396694655963));
#56102=CARTESIAN_POINT('Ctrl Pts',(-86.3899999999999,44.5787611019615,-50.6321469729213));
#56103=CARTESIAN_POINT('Ctrl Pts',(-86.3900000000001,40.5938700967862,-50.2396694655963));
#56104=CARTESIAN_POINT('Ctrl Pts',(-86.3899999999999,38.0507425038934,-49.4763401417082));
#56105=CARTESIAN_POINT('Ctrl Pts',(-86.3899999999999,36.8454205811756,-48.9853996542502));
#56106=CARTESIAN_POINT('Origin',(-86.39,36.2795905006212,-50.3745851422034));
#56107=CARTESIAN_POINT('',(-86.39,27.1763562679741,-53.8202275904635));
#56108=CARTESIAN_POINT('Ctrl Pts',(-86.3899999999997,15.2486853399057,-33.1606917253389));
#56109=CARTESIAN_POINT('Ctrl Pts',(-86.3899999999997,15.3424414315477,-34.0308350004374));
#56110=CARTESIAN_POINT('Ctrl Pts',(-86.3899999999997,15.7669892582787,-36.8072826511436));
#56111=CARTESIAN_POINT('Ctrl Pts',(-86.3899999999997,17.1486274506748,-41.3619333760696));
#56112=CARTESIAN_POINT('Ctrl Pts',(-86.3899999999996,19.8922930183494,-46.4949706191462));
#56113=CARTESIAN_POINT('Ctrl Pts',(-86.3899999999997,23.3219850986922,-50.6740625107251));
#56114=CARTESIAN_POINT('Ctrl Pts',(-86.3899999999998,25.9500938140347,-52.9242386124823));
#56115=CARTESIAN_POINT('Ctrl Pts',(-86.3899999999998,27.17635626841,-53.820227589861));
#56116=CARTESIAN_POINT('Origin',(-86.39,28.0613000948908,-52.6090816762843));
#56117=CARTESIAN_POINT('',(-86.39,32.0036528606872,-46.1899302415183));
#56118=CARTESIAN_POINT('Origin',(-86.39,31.0834721426076,-47.3745261404244));
#56119=CARTESIAN_POINT('',(-86.39,24.2703224391255,-32.7955273885202));
#56120=CARTESIAN_POINT('Ctrl Pts',(-86.39,32.0036528607881,-46.1899302405967));
#56121=CARTESIAN_POINT('Ctrl Pts',(-86.3899999999999,31.3290269997021,-45.6658884897885));
#56122=CARTESIAN_POINT('Ctrl Pts',(-86.3899999999997,29.6788853182468,-44.2104874631114));
#56123=CARTESIAN_POINT('Ctrl Pts',(-86.3899999999999,27.4237578574175,-41.4626067014406));
#56124=CARTESIAN_POINT('Ctrl Pts',(-86.3899999999996,25.5171428019148,-37.8955808206585));
#56125=CARTESIAN_POINT('Ctrl Pts',(-86.39,24.6157110848108,-34.923958693842));
#56126=CARTESIAN_POINT('Ctrl Pts',(-86.39,24.3257980082209,-33.198694346047));
#56127=CARTESIAN_POINT('Ctrl Pts',(-86.39,24.2703224391255,-32.7955273885202));
#56128=CARTESIAN_POINT('Origin',(-86.39,22.7843241379305,-33.));
#56129=CARTESIAN_POINT('',(-86.39,27.1763562680412,-6.17977240960921));
#56130=CARTESIAN_POINT('Ctrl Pts',(-86.3899999999997,27.1763562684101,-6.17977241013893));
#56131=CARTESIAN_POINT('Ctrl Pts',(-86.3899999999997,25.9500938140348,-7.0757613875177));
#56132=CARTESIAN_POINT('Ctrl Pts',(-86.3899999999997,23.3219850986922,-9.32593748927488));
#56133=CARTESIAN_POINT('Ctrl Pts',(-86.3899999999997,19.8922930183494,-13.5050293808538));
#56134=CARTESIAN_POINT('Ctrl Pts',(-86.3899999999996,17.1486274506748,-18.6380666239304));
#56135=CARTESIAN_POINT('Ctrl Pts',(-86.3899999999997,15.7669892582787,-23.1927173488564));
#56136=CARTESIAN_POINT('Ctrl Pts',(-86.3899999999997,15.3424414315477,-25.9691649995626));
#56137=CARTESIAN_POINT('Ctrl Pts',(-86.3899999999997,15.2486853399057,-26.8393082746611));
#56138=CARTESIAN_POINT('',(-86.3899999999999,24.2703224391227,-27.2044726115005));
#56139=CARTESIAN_POINT('Origin',(-86.39,22.7843241379304,-27.));
#56140=CARTESIAN_POINT('',(-86.39,32.0036528607432,-13.8100697584875));
#56141=CARTESIAN_POINT('Ctrl Pts',(-86.3899999999999,24.2703224391227,-27.2044726115005));
#56142=CARTESIAN_POINT('Ctrl Pts',(-86.3899999999999,24.3257980082209,-26.801305653953));
#56143=CARTESIAN_POINT('Ctrl Pts',(-86.3899999999999,24.6157110848108,-25.076041306158));
#56144=CARTESIAN_POINT('Ctrl Pts',(-86.39,25.5171428019148,-22.1044191793415));
#56145=CARTESIAN_POINT('Ctrl Pts',(-86.3899999999999,27.4237578574175,-18.5373932985594));
#56146=CARTESIAN_POINT('Ctrl Pts',(-86.39,29.6788853182468,-15.7895125368886));
#56147=CARTESIAN_POINT('Ctrl Pts',(-86.3899999999999,31.3290269997022,-14.3341115102115));
#56148=CARTESIAN_POINT('Ctrl Pts',(-86.3899999999999,32.0036528607881,-13.8100697594033));
#56149=CARTESIAN_POINT('Origin',(-86.39,31.0834721426076,-12.6254738595756));
#56150=CARTESIAN_POINT('Origin',(-86.39,28.0613000948908,-7.39091832371568));
#56151=CARTESIAN_POINT('Origin',(-86.39,30.2431724514241,0.829967899138609));
#56152=CARTESIAN_POINT('',(-86.39,58.2818165767216,-0.530143045432115));
#56153=CARTESIAN_POINT('Ctrl Pts',(-86.39,44.5787611019615,2.5));
#56154=CARTESIAN_POINT('Ctrl Pts',(-86.3899999999999,46.7058634824009,2.5));
#56155=CARTESIAN_POINT('Ctrl Pts',(-86.3899999999999,50.9600682432795,2.08099740293233));
#56156=CARTESIAN_POINT('Ctrl Pts',(-86.39,55.4939941495213,0.705646015552456));
#56157=CARTESIAN_POINT('Ctrl Pts',(-86.39,57.863878739489,-0.335776881547477));
#56158=CARTESIAN_POINT('Ctrl Pts',(-86.39,58.2818165767217,-0.530143045432121));
#56159=CARTESIAN_POINT('Origin',(-86.39,58.914349752499,0.829967899138591));
#56160=CARTESIAN_POINT('Origin',(-86.39,61.1722800421212,4.74081788071294));
#56161=CARTESIAN_POINT('Origin',(-86.39,66.3683162853859,1.74061665201678));
#56162=CARTESIAN_POINT('',(-86.39,76.9518771320469,-27.1323759919381));
#56163=CARTESIAN_POINT('Ctrl Pts',(-86.3899999999998,63.2487659306122,-3.39775347084041));
#56164=CARTESIAN_POINT('Ctrl Pts',(-86.3899999999998,64.7867667693756,-4.47726951085139));
#56165=CARTESIAN_POINT('Ctrl Pts',(-86.39,67.8660024791148,-7.0635732469528));
#56166=CARTESIAN_POINT('Ctrl Pts',(-86.3900000000002,71.775717465263,-11.8275747416186));
#56167=CARTESIAN_POINT('Ctrl Pts',(-86.3899999999997,74.7983998703283,-17.4826157721267));
#56168=CARTESIAN_POINT('Ctrl Pts',(-86.39,76.3805781139171,-22.698358449033));
#56169=CARTESIAN_POINT('Ctrl Pts',(-86.3899999999999,76.8486238665249,-25.9669410775951));
#56170=CARTESIAN_POINT('Ctrl Pts',(-86.3899999999999,76.9518771315612,-27.1323759917098));
#56171=CARTESIAN_POINT('Origin',(-86.39,78.4460245797131,-27.));
#56172=CARTESIAN_POINT('Origin',(-86.39,82.9621121574678,-27.));
#56173=CARTESIAN_POINT('',(-86.3899999999999,67.2171661194344,-62.9773275507524));
#56174=CARTESIAN_POINT('',(-86.3899999999999,84.4575665229983,-33.1166895167565));
#56175=CARTESIAN_POINT('Ctrl Pts',(-86.3899999999999,67.2171661194344,-62.9773275507524));
#56176=CARTESIAN_POINT('Ctrl Pts',(-86.39,68.1585542512634,-62.3311804544817));
#56177=CARTESIAN_POINT('Ctrl Pts',(-86.39,70.120027043277,-60.8582491474625));
#56178=CARTESIAN_POINT('Ctrl Pts',(-86.3899999999999,72.9083073089528,-58.329286199092));
#56179=CARTESIAN_POINT('Ctrl Pts',(-86.3899999999999,75.5496661779346,-55.41704471446));
#56180=CARTESIAN_POINT('Ctrl Pts',(-86.3900000000001,77.8907325893732,-52.2581266162731));
#56181=CARTESIAN_POINT('Ctrl Pts',(-86.3899999999996,79.9131883593013,-48.8865394828812));
#56182=CARTESIAN_POINT('Ctrl Pts',(-86.3899999999997,81.5929974870803,-45.3315997101041));
#56183=CARTESIAN_POINT('Ctrl Pts',(-86.39,82.9188283169055,-41.6302351306666));
#56184=CARTESIAN_POINT('Ctrl Pts',(-86.3899999999999,83.8728260383109,-37.8158880252114));
#56185=CARTESIAN_POINT('Ctrl Pts',(-86.3899999999998,84.2979456369875,-34.9568586727847));
#56186=CARTESIAN_POINT('Ctrl Pts',(-86.3899999999998,84.4366426410887,-33.3848430749953));
#56187=CARTESIAN_POINT('Ctrl Pts',(-86.3899999999999,84.4575665229983,-33.1166895167565));
#56188=CARTESIAN_POINT('Origin',(-86.39,82.9621122252415,-33.));
#56189=CARTESIAN_POINT('',(-86.39,76.9518771320466,-32.8676240081228));
#56190=CARTESIAN_POINT('Origin',(-86.39,78.4460245797131,-33.));
#56191=CARTESIAN_POINT('Ctrl Pts',(-86.39,76.9518771315612,-32.8676240082902));
#56192=CARTESIAN_POINT('Ctrl Pts',(-86.39,76.8486238665249,-34.0330589224049));
#56193=CARTESIAN_POINT('Ctrl Pts',(-86.3900000000001,76.3805781139171,-37.301641550967));
#56194=CARTESIAN_POINT('Ctrl Pts',(-86.3899999999998,74.7983998703283,-42.5173842278733));
#56195=CARTESIAN_POINT('Ctrl Pts',(-86.3899999999998,71.7757174652631,-48.1724252583814));
#56196=CARTESIAN_POINT('Ctrl Pts',(-86.3900000000001,67.8660024791148,-52.9364267530473));
#56197=CARTESIAN_POINT('Ctrl Pts',(-86.39,64.7867667693755,-55.5227304891487));
#56198=CARTESIAN_POINT('Ctrl Pts',(-86.39,63.248765930612,-56.6022465291597));
#56199=CARTESIAN_POINT('Origin',(-86.39,66.3683162666315,-61.7406166195334));
#56200=CARTESIAN_POINT('Origin',(-86.39,61.1722799429393,-64.740817708925));
#56201=CARTESIAN_POINT('',(-86.39,58.2818165768387,-59.4698569545135));
#56202=CARTESIAN_POINT('Origin',(-86.39,58.9143497524989,-60.8299678991386));
#56203=CARTESIAN_POINT('',(-86.3899999999999,30.8757056272014,-59.4698569545679));
#56204=CARTESIAN_POINT('Ctrl Pts',(-86.39,58.2818165768387,-59.4698569545134));
#56205=CARTESIAN_POINT('Ctrl Pts',(-86.39,57.863878739489,-59.6642231184525));
#56206=CARTESIAN_POINT('Ctrl Pts',(-86.39,55.4939941495213,-60.7056460155525));
#56207=CARTESIAN_POINT('Ctrl Pts',(-86.3899999999999,50.9600682432795,-62.0809974029323));
#56208=CARTESIAN_POINT('Ctrl Pts',(-86.39,44.5787611019615,-62.7095012985338));
#56209=CARTESIAN_POINT('Ctrl Pts',(-86.3900000000001,38.1974539606436,-62.0809974029323));
#56210=CARTESIAN_POINT('Ctrl Pts',(-86.3899999999999,33.6635280544017,-60.7056460155525));
#56211=CARTESIAN_POINT('Ctrl Pts',(-86.3899999999999,31.293643464434,-59.6642231184525));
#56212=CARTESIAN_POINT('Ctrl Pts',(-86.3899999999999,30.8757056272014,-59.4698569545679));
#56213=CARTESIAN_POINT('Origin',(-86.39,30.2431724514241,-60.8299678991386));
#56214=CARTESIAN_POINT('Origin',(-86.39,22.7892059208967,-61.7406166479301));
#56215=CARTESIAN_POINT('',(-86.39,25.9087562731289,-56.6022465300058));
#56216=CARTESIAN_POINT('Origin',(-86.39,25.0470014756374,-57.8300000340158));
#56217=CARTESIAN_POINT('',(-86.39,12.2056450718761,-32.8676240080646));
#56218=CARTESIAN_POINT('Ctrl Pts',(-86.3899999999997,25.9087562733108,-56.6022465291596));
#56219=CARTESIAN_POINT('Ctrl Pts',(-86.3899999999997,24.3707554345474,-55.5227304891486));
#56220=CARTESIAN_POINT('Ctrl Pts',(-86.3899999999997,21.2915197248082,-52.9364267530472));
#56221=CARTESIAN_POINT('Ctrl Pts',(-86.3900000000001,17.38180473866,-48.1724252583814));
#56222=CARTESIAN_POINT('Ctrl Pts',(-86.39,14.3591223335948,-42.5173842278733));
#56223=CARTESIAN_POINT('Ctrl Pts',(-86.3899999999999,12.776944090006,-37.301641550967));
#56224=CARTESIAN_POINT('Ctrl Pts',(-86.3899999999998,12.3088983373981,-34.0330589224049));
#56225=CARTESIAN_POINT('Ctrl Pts',(-86.3899999999998,12.2056450723618,-32.8676240082902));
#56226=CARTESIAN_POINT('Origin',(-86.39,10.7114976242099,-33.));
#56227=CARTESIAN_POINT('',(-86.39,12.2056450718764,-27.13237599188));
#56228=CARTESIAN_POINT('Origin',(-86.39,10.7114976242099,-27.));
#56229=CARTESIAN_POINT('',(-86.39,25.9087562731469,-3.39775347015071));
#56230=CARTESIAN_POINT('Ctrl Pts',(-86.3899999999999,12.2056450723618,-27.1323759917097));
#56231=CARTESIAN_POINT('Ctrl Pts',(-86.3899999999999,12.3088983373981,-25.966941077595));
#56232=CARTESIAN_POINT('Ctrl Pts',(-86.3899999999999,12.776944090006,-22.698358449033));
#56233=CARTESIAN_POINT('Ctrl Pts',(-86.39,14.3591223335948,-17.4826157721267));
#56234=CARTESIAN_POINT('Ctrl Pts',(-86.3899999999999,17.38180473866,-11.8275747416186));
#56235=CARTESIAN_POINT('Ctrl Pts',(-86.39,21.2915197248083,-7.06357324695279));
#56236=CARTESIAN_POINT('Ctrl Pts',(-86.39,24.3707554345475,-4.47726951085134));
#56237=CARTESIAN_POINT('Ctrl Pts',(-86.39,25.9087562733109,-3.39775347084034));
#56238=CARTESIAN_POINT('Origin',(-86.39,25.0470014756374,-2.16999996598413));
#56239=CARTESIAN_POINT('Origin',(-86.39,22.789205939653,1.74061661544304));
#56240=CARTESIAN_POINT('Ctrl Pts',(-85.5899999999998,84.4575665229977,-33.1166895167634));
#56241=CARTESIAN_POINT('Ctrl Pts',(-86.55,84.4575665229977,-33.1166895167634));
#56242=CARTESIAN_POINT('Ctrl Pts',(-85.5899999999998,84.4366426410883,-33.3848430749998));
#56243=CARTESIAN_POINT('Ctrl Pts',(-86.55,84.4366426410883,-33.3848430749998));
#56244=CARTESIAN_POINT('Ctrl Pts',(-85.5899999999997,84.2979456369872,-34.9568586727869));
#56245=CARTESIAN_POINT('Ctrl Pts',(-86.55,84.2979456369872,-34.9568586727869));
#56246=CARTESIAN_POINT('Ctrl Pts',(-85.5899999999998,83.8728260383109,-37.8158880252114));
#56247=CARTESIAN_POINT('Ctrl Pts',(-86.55,83.8728260383109,-37.8158880252114));
#56248=CARTESIAN_POINT('Ctrl Pts',(-85.59,82.9188283169055,-41.6302351306666));
#56249=CARTESIAN_POINT('Ctrl Pts',(-86.5500000000002,82.9188283169055,-41.6302351306666));
#56250=CARTESIAN_POINT('Ctrl Pts',(-85.5899999999997,81.5929974870803,-45.3315997101041));
#56251=CARTESIAN_POINT('Ctrl Pts',(-86.5499999999999,81.5929974870803,-45.3315997101041));
#56252=CARTESIAN_POINT('Ctrl Pts',(-85.5899999999996,79.9131883593013,-48.8865394828812));
#56253=CARTESIAN_POINT('Ctrl Pts',(-86.5499999999998,79.9131883593013,-48.8865394828812));
#56254=CARTESIAN_POINT('Ctrl Pts',(-85.5900000000001,77.8907325893732,-52.2581266162731));
#56255=CARTESIAN_POINT('Ctrl Pts',(-86.5500000000003,77.8907325893732,-52.2581266162731));
#56256=CARTESIAN_POINT('Ctrl Pts',(-85.5899999999998,75.5496661779346,-55.41704471446));
#56257=CARTESIAN_POINT('Ctrl Pts',(-86.55,75.5496661779346,-55.41704471446));
#56258=CARTESIAN_POINT('Ctrl Pts',(-85.5899999999998,72.9083073089528,-58.329286199092));
#56259=CARTESIAN_POINT('Ctrl Pts',(-86.55,72.9083073089528,-58.329286199092));
#56260=CARTESIAN_POINT('Ctrl Pts',(-85.5899999999999,70.1200270432783,-60.8582491474613));
#56261=CARTESIAN_POINT('Ctrl Pts',(-86.5500000000002,70.1200270432783,-60.8582491474613));
#56262=CARTESIAN_POINT('Ctrl Pts',(-85.59,68.1585542512663,-62.3311804544795));
#56263=CARTESIAN_POINT('Ctrl Pts',(-86.5500000000002,68.1585542512663,-62.3311804544795));
#56264=CARTESIAN_POINT('Ctrl Pts',(-85.5899999999999,67.2171661194389,-62.9773275507493));
#56265=CARTESIAN_POINT('Ctrl Pts',(-86.5500000000001,67.2171661194389,-62.9773275507493));
#56266=CARTESIAN_POINT('',(-86.39,67.2171661194344,-62.9773275507524));
#56267=CARTESIAN_POINT('',(-85.5899999999996,84.4575665229983,-33.1166895167565));
#56268=CARTESIAN_POINT('Origin',(913.61,45.8777992076386,-29.25));
#56269=CARTESIAN_POINT('',(-86.3900000000002,53.7358855886589,-42.860604862193));
#56270=CARTESIAN_POINT('Origin',(913.61,43.2797229962853,-30.75));
#56271=CARTESIAN_POINT('',(-85.5899999999994,51.1378158375422,-44.3606160516509));
#56272=CARTESIAN_POINT('',(-86.39,47.7866618629516,-38.5562471036737));
#56273=CARTESIAN_POINT('Origin',(913.61,45.8777992076386,-30.75));
#56274=CARTESIAN_POINT('',(-85.5899999999993,41.3708603409714,-38.5562471036737));
#56275=CARTESIAN_POINT('Origin',(913.61,43.2797229962853,-29.25));
#56276=CARTESIAN_POINT('',(-85.5899999999993,35.4216366152641,-42.860604862193));
#56277=CARTESIAN_POINT('',(-86.3899999999997,38.7727956517265,-37.0562271467965));
#56278=CARTESIAN_POINT('Origin',(913.61,4.00385864813601E-13,-31.5));
#56279=CARTESIAN_POINT('',(-85.5899999999992,35.5649111404189,-31.5));
#56280=CARTESIAN_POINT('Origin',(913.61,4.00385864813601E-13,-28.5));
#56281=CARTESIAN_POINT('',(-86.3899999999997,35.5649111404189,-28.5));
#56282=CARTESIAN_POINT('Origin',(913.61,43.2797229962853,-30.75));
#56283=CARTESIAN_POINT('',(-86.3900000000002,35.4216366152641,-17.139395137807));
#56284=CARTESIAN_POINT('',(-85.5899999999991,38.7727956517265,-22.9437728532035));
#56285=CARTESIAN_POINT('Origin',(913.61,43.2797229962853,-29.25));
#56286=CARTESIAN_POINT('',(-86.3900000000004,51.1378158375422,-15.6393839483491));
#56287=CARTESIAN_POINT('',(-85.5899999999988,47.7866618629516,-21.4437528963263));
#56288=CARTESIAN_POINT('Origin',(913.61,45.8777992076386,-30.75));
#56289=CARTESIAN_POINT('',(-85.5899999999994,53.7358855886589,-17.139395137807));
#56290=CARTESIAN_POINT('Origin',(913.61,4.00385864813601E-13,-28.5));
#56291=CARTESIAN_POINT('',(-86.3900000000002,60.2949931567668,-28.5));
#56292=CARTESIAN_POINT('',(-85.5899999999991,53.5926110635042,-28.5));
#56293=CARTESIAN_POINT('Origin',(913.61,4.00385864813601E-13,-31.5));
#56294=CARTESIAN_POINT('',(-86.39,53.5926110635042,-31.5));
#56295=CARTESIAN_POINT('',(-85.5899999999993,60.2949931567668,-31.5));
#56296=CARTESIAN_POINT('Ctrl Pts',(-85.5899999999998,61.981165935513,-53.820227589861));
#56297=CARTESIAN_POINT('Ctrl Pts',(-86.55,61.981165935513,-53.820227589861));
#56298=CARTESIAN_POINT('Ctrl Pts',(-85.5899999999998,63.2074283898883,-52.9242386124823));
#56299=CARTESIAN_POINT('Ctrl Pts',(-86.55,63.2074283898883,-52.9242386124823));
#56300=CARTESIAN_POINT('Ctrl Pts',(-85.5899999999998,65.8355371052309,-50.6740625107251));
#56301=CARTESIAN_POINT('Ctrl Pts',(-86.55,65.8355371052309,-50.6740625107251));
#56302=CARTESIAN_POINT('Ctrl Pts',(-85.5899999999998,69.2652291855737,-46.4949706191462));
#56303=CARTESIAN_POINT('Ctrl Pts',(-86.55,69.2652291855737,-46.4949706191462));
#56304=CARTESIAN_POINT('Ctrl Pts',(-85.5900000000001,72.0088947532483,-41.3619333760696));
#56305=CARTESIAN_POINT('Ctrl Pts',(-86.5500000000002,72.0088947532483,-41.3619333760696));
#56306=CARTESIAN_POINT('Ctrl Pts',(-85.5899999999998,73.3905329456444,-36.8072826511436));
#56307=CARTESIAN_POINT('Ctrl Pts',(-86.5499999999999,73.3905329456444,-36.8072826511436));
#56308=CARTESIAN_POINT('Ctrl Pts',(-85.5899999999997,73.8150807723754,-34.0308350004374));
#56309=CARTESIAN_POINT('Ctrl Pts',(-86.5499999999998,73.8150807723754,-34.0308350004374));
#56310=CARTESIAN_POINT('Ctrl Pts',(-85.5899999999997,73.9088368640174,-33.1606917253389));
#56311=CARTESIAN_POINT('Ctrl Pts',(-86.5499999999998,73.9088368640174,-33.1606917253389));
#56312=CARTESIAN_POINT('',(-85.59,73.9088368640223,-33.1606917252932));
#56313=CARTESIAN_POINT('',(-86.3899999999997,61.9811659354668,-53.8202275898948));
#56314=CARTESIAN_POINT('Ctrl Pts',(-85.5899999999998,76.9518771315612,-32.8676240082902));
#56315=CARTESIAN_POINT('Ctrl Pts',(-86.5500000000002,76.9518771315612,-32.8676240082902));
#56316=CARTESIAN_POINT('Ctrl Pts',(-85.5899999999999,76.8486238665249,-34.0330589224049));
#56317=CARTESIAN_POINT('Ctrl Pts',(-86.5500000000002,76.8486238665249,-34.0330589224049));
#56318=CARTESIAN_POINT('Ctrl Pts',(-85.59,76.3805781139171,-37.301641550967));
#56319=CARTESIAN_POINT('Ctrl Pts',(-86.5500000000004,76.3805781139171,-37.301641550967));
#56320=CARTESIAN_POINT('Ctrl Pts',(-85.5899999999997,74.7983998703283,-42.5173842278733));
#56321=CARTESIAN_POINT('Ctrl Pts',(-86.5500000000001,74.7983998703283,-42.5173842278733));
#56322=CARTESIAN_POINT('Ctrl Pts',(-85.5899999999997,71.7757174652631,-48.1724252583814));
#56323=CARTESIAN_POINT('Ctrl Pts',(-86.5500000000001,71.7757174652631,-48.1724252583814));
#56324=CARTESIAN_POINT('Ctrl Pts',(-85.5899999999999,67.8660024791148,-52.9364267530473));
#56325=CARTESIAN_POINT('Ctrl Pts',(-86.5500000000003,67.8660024791148,-52.9364267530473));
#56326=CARTESIAN_POINT('Ctrl Pts',(-85.5899999999999,64.7867667693755,-55.5227304891487));
#56327=CARTESIAN_POINT('Ctrl Pts',(-86.5500000000002,64.7867667693755,-55.5227304891487));
#56328=CARTESIAN_POINT('Ctrl Pts',(-85.5899999999999,63.248765930612,-56.6022465291597));
#56329=CARTESIAN_POINT('Ctrl Pts',(-86.5500000000002,63.248765930612,-56.6022465291597));
#56330=CARTESIAN_POINT('',(-86.39,76.9518771315567,-32.8676240083405));
#56331=CARTESIAN_POINT('Ctrl Pts',(-85.59,73.9088368640174,-26.839308274661));
#56332=CARTESIAN_POINT('Ctrl Pts',(-86.5499999999999,73.9088368640174,-26.839308274661));
#56333=CARTESIAN_POINT('Ctrl Pts',(-85.59,73.8150807723753,-25.9691649995626));
#56334=CARTESIAN_POINT('Ctrl Pts',(-86.5499999999999,73.8150807723753,-25.9691649995626));
#56335=CARTESIAN_POINT('Ctrl Pts',(-85.5900000000001,73.3905329456444,-23.1927173488564));
#56336=CARTESIAN_POINT('Ctrl Pts',(-86.55,73.3905329456444,-23.1927173488564));
#56337=CARTESIAN_POINT('Ctrl Pts',(-85.59,72.0088947532483,-18.6380666239304));
#56338=CARTESIAN_POINT('Ctrl Pts',(-86.5499999999999,72.0088947532483,-18.6380666239304));
#56339=CARTESIAN_POINT('Ctrl Pts',(-85.59,69.2652291855737,-13.5050293808538));
#56340=CARTESIAN_POINT('Ctrl Pts',(-86.5499999999999,69.2652291855737,-13.5050293808538));
#56341=CARTESIAN_POINT('Ctrl Pts',(-85.5900000000002,65.8355371052309,-9.3259374892749));
#56342=CARTESIAN_POINT('Ctrl Pts',(-86.5500000000002,65.8355371052309,-9.3259374892749));
#56343=CARTESIAN_POINT('Ctrl Pts',(-85.5900000000001,63.2074283898883,-7.07576138751773));
#56344=CARTESIAN_POINT('Ctrl Pts',(-86.55,63.2074283898883,-7.07576138751773));
#56345=CARTESIAN_POINT('Ctrl Pts',(-85.5900000000001,61.981165935513,-6.17977241013897));
#56346=CARTESIAN_POINT('Ctrl Pts',(-86.55,61.981165935513,-6.17977241013897));
#56347=CARTESIAN_POINT('',(-85.5900000000001,61.9811659354668,-6.1797724101052));
#56348=CARTESIAN_POINT('',(-86.3899999999997,73.9088368640223,-26.8393082747068));
#56349=CARTESIAN_POINT('Ctrl Pts',(-85.5899999999999,63.2487659306122,-3.39775347084041));
#56350=CARTESIAN_POINT('Ctrl Pts',(-86.5500000000002,63.2487659306122,-3.39775347084041));
#56351=CARTESIAN_POINT('Ctrl Pts',(-85.5899999999999,64.7867667693756,-4.47726951085139));
#56352=CARTESIAN_POINT('Ctrl Pts',(-86.5500000000002,64.7867667693756,-4.47726951085139));
#56353=CARTESIAN_POINT('Ctrl Pts',(-85.5900000000001,67.8660024791148,-7.0635732469528));
#56354=CARTESIAN_POINT('Ctrl Pts',(-86.5500000000004,67.8660024791148,-7.0635732469528));
#56355=CARTESIAN_POINT('Ctrl Pts',(-85.5900000000003,71.775717465263,-11.8275747416186));
#56356=CARTESIAN_POINT('Ctrl Pts',(-86.5500000000006,71.775717465263,-11.8275747416186));
#56357=CARTESIAN_POINT('Ctrl Pts',(-85.5899999999998,74.7983998703283,-17.4826157721267));
#56358=CARTESIAN_POINT('Ctrl Pts',(-86.5500000000002,74.7983998703283,-17.4826157721267));
#56359=CARTESIAN_POINT('Ctrl Pts',(-85.5900000000001,76.3805781139171,-22.698358449033));
#56360=CARTESIAN_POINT('Ctrl Pts',(-86.5500000000004,76.3805781139171,-22.698358449033));
#56361=CARTESIAN_POINT('Ctrl Pts',(-85.59,76.8486238665249,-25.9669410775951));
#56362=CARTESIAN_POINT('Ctrl Pts',(-86.5500000000004,76.8486238665249,-25.9669410775951));
#56363=CARTESIAN_POINT('Ctrl Pts',(-85.59,76.9518771315612,-27.1323759917098));
#56364=CARTESIAN_POINT('Ctrl Pts',(-86.5500000000003,76.9518771315612,-27.1323759917098));
#56365=CARTESIAN_POINT('',(-85.5900000000001,76.9518771315568,-27.1323759916595));
#56366=CARTESIAN_POINT('Ctrl Pts',(-85.5899999999998,44.5787611019615,-0.5));
#56367=CARTESIAN_POINT('Ctrl Pts',(-86.55,44.5787611019615,-0.5));
#56368=CARTESIAN_POINT('Ctrl Pts',(-85.5899999999998,42.6480066335628,-0.5));
#56369=CARTESIAN_POINT('Ctrl Pts',(-86.55,42.6480066335628,-0.5));
#56370=CARTESIAN_POINT('Ctrl Pts',(-85.5899999999994,38.7864976967653,-0.880325434261422));
#56371=CARTESIAN_POINT('Ctrl Pts',(-86.5499999999996,38.7864976967653,-0.880325434261422));
#56372=CARTESIAN_POINT('Ctrl Pts',(-85.5899999999995,34.8506764348762,-2.07424376132674));
#56373=CARTESIAN_POINT('Ctrl Pts',(-86.5499999999997,34.8506764348762,-2.07424376132674));
#56374=CARTESIAN_POINT('Ctrl Pts',(-85.5899999999996,32.8626902557638,-2.92534739713908));
#56375=CARTESIAN_POINT('Ctrl Pts',(-86.5499999999998,32.8626902557638,-2.92534739713908));
#56376=CARTESIAN_POINT('Ctrl Pts',(-85.5899999999996,32.6508629759047,-3.01900602948033));
#56377=CARTESIAN_POINT('Ctrl Pts',(-86.5499999999998,32.6508629759047,-3.01900602948033));
#56378=CARTESIAN_POINT('Ctrl Pts',(-85.5899999999998,44.5787611019615,2.5));
#56379=CARTESIAN_POINT('Ctrl Pts',(-86.5500000000001,44.5787611019615,2.5));
#56380=CARTESIAN_POINT('Ctrl Pts',(-85.5899999999998,46.7058634824009,2.5));
#56381=CARTESIAN_POINT('Ctrl Pts',(-86.5500000000001,46.7058634824009,2.5));
#56382=CARTESIAN_POINT('Ctrl Pts',(-85.5899999999997,50.9600682432795,2.08099740293233));
#56383=CARTESIAN_POINT('Ctrl Pts',(-86.55,50.9600682432795,2.08099740293233));
#56384=CARTESIAN_POINT('Ctrl Pts',(-85.5899999999999,55.4939941495213,0.705646015552456));
#56385=CARTESIAN_POINT('Ctrl Pts',(-86.5500000000002,55.4939941495213,0.705646015552456));
#56386=CARTESIAN_POINT('Ctrl Pts',(-85.5899999999998,57.863878739489,-0.335776881547477));
#56387=CARTESIAN_POINT('Ctrl Pts',(-86.5500000000001,57.863878739489,-0.335776881547477));
#56388=CARTESIAN_POINT('Ctrl Pts',(-85.5899999999998,58.2818165781778,-0.530143046109336));
#56389=CARTESIAN_POINT('Ctrl Pts',(-86.5500000000001,58.2818165781778,-0.530143046109336));
#56390=CARTESIAN_POINT('',(-85.5900000000001,58.2818165781183,-0.530143046081633));
#56391=CARTESIAN_POINT('Ctrl Pts',(-85.5900000000001,27.1763562684101,-6.17977241013893));
#56392=CARTESIAN_POINT('Ctrl Pts',(-86.5499999999997,27.1763562684101,-6.17977241013893));
#56393=CARTESIAN_POINT('Ctrl Pts',(-85.5900000000001,25.9500938140348,-7.0757613875177));
#56394=CARTESIAN_POINT('Ctrl Pts',(-86.5499999999997,25.9500938140348,-7.0757613875177));
#56395=CARTESIAN_POINT('Ctrl Pts',(-85.5900000000001,23.3219850986922,-9.32593748927488));
#56396=CARTESIAN_POINT('Ctrl Pts',(-86.5499999999997,23.3219850986922,-9.32593748927488));
#56397=CARTESIAN_POINT('Ctrl Pts',(-85.5900000000001,19.8922930183494,-13.5050293808538));
#56398=CARTESIAN_POINT('Ctrl Pts',(-86.5499999999997,19.8922930183494,-13.5050293808538));
#56399=CARTESIAN_POINT('Ctrl Pts',(-85.59,17.1486274506748,-18.6380666239304));
#56400=CARTESIAN_POINT('Ctrl Pts',(-86.5499999999996,17.1486274506748,-18.6380666239304));
#56401=CARTESIAN_POINT('Ctrl Pts',(-85.59,15.7669892582787,-23.1927173488564));
#56402=CARTESIAN_POINT('Ctrl Pts',(-86.5499999999996,15.7669892582787,-23.1927173488564));
#56403=CARTESIAN_POINT('Ctrl Pts',(-85.59,15.3424414315477,-25.9691649995626));
#56404=CARTESIAN_POINT('Ctrl Pts',(-86.5499999999997,15.3424414315477,-25.9691649995626));
#56405=CARTESIAN_POINT('Ctrl Pts',(-85.5900000000001,15.2486853399057,-26.8393082746611));
#56406=CARTESIAN_POINT('Ctrl Pts',(-86.5499999999997,15.2486853399057,-26.8393082746611));
#56407=CARTESIAN_POINT('',(-86.3899999999997,27.1763562684563,-6.17977241010519));
#56408=CARTESIAN_POINT('Ctrl Pts',(-85.59,12.2056450723618,-27.1323759917097));
#56409=CARTESIAN_POINT('Ctrl Pts',(-86.55,12.2056450723618,-27.1323759917097));
#56410=CARTESIAN_POINT('Ctrl Pts',(-85.59,12.3088983373981,-25.966941077595));
#56411=CARTESIAN_POINT('Ctrl Pts',(-86.55,12.3088983373981,-25.966941077595));
#56412=CARTESIAN_POINT('Ctrl Pts',(-85.59,12.776944090006,-22.698358449033));
#56413=CARTESIAN_POINT('Ctrl Pts',(-86.55,12.776944090006,-22.698358449033));
#56414=CARTESIAN_POINT('Ctrl Pts',(-85.5900000000001,14.3591223335948,-17.4826157721267));
#56415=CARTESIAN_POINT('Ctrl Pts',(-86.5500000000001,14.3591223335948,-17.4826157721267));
#56416=CARTESIAN_POINT('Ctrl Pts',(-85.59,17.38180473866,-11.8275747416186));
#56417=CARTESIAN_POINT('Ctrl Pts',(-86.55,17.38180473866,-11.8275747416186));
#56418=CARTESIAN_POINT('Ctrl Pts',(-85.5900000000001,21.2915197248083,-7.06357324695279));
#56419=CARTESIAN_POINT('Ctrl Pts',(-86.5500000000001,21.2915197248083,-7.06357324695279));
#56420=CARTESIAN_POINT('Ctrl Pts',(-85.5900000000001,24.3707554345475,-4.47726951085134));
#56421=CARTESIAN_POINT('Ctrl Pts',(-86.5500000000001,24.3707554345475,-4.47726951085134));
#56422=CARTESIAN_POINT('Ctrl Pts',(-85.5900000000001,25.9087562733109,-3.39775347084034));
#56423=CARTESIAN_POINT('Ctrl Pts',(-86.5500000000001,25.9087562733109,-3.39775347084034));
#56424=CARTESIAN_POINT('',(-86.39,12.2056450723663,-27.1323759916595));
#56425=CARTESIAN_POINT('',(-85.5900000000001,25.9087562733283,-3.39775347082815));
#56426=CARTESIAN_POINT('Ctrl Pts',(-85.59,15.2486853399057,-33.1606917253389));
#56427=CARTESIAN_POINT('Ctrl Pts',(-86.5499999999998,15.2486853399057,-33.1606917253389));
#56428=CARTESIAN_POINT('Ctrl Pts',(-85.59,15.3424414315477,-34.0308350004374));
#56429=CARTESIAN_POINT('Ctrl Pts',(-86.5499999999998,15.3424414315477,-34.0308350004374));
#56430=CARTESIAN_POINT('Ctrl Pts',(-85.59,15.7669892582787,-36.8072826511436));
#56431=CARTESIAN_POINT('Ctrl Pts',(-86.5499999999997,15.7669892582787,-36.8072826511436));
#56432=CARTESIAN_POINT('Ctrl Pts',(-85.5900000000001,17.1486274506748,-41.3619333760696));
#56433=CARTESIAN_POINT('Ctrl Pts',(-86.5499999999998,17.1486274506748,-41.3619333760696));
#56434=CARTESIAN_POINT('Ctrl Pts',(-85.59,19.8922930183494,-46.4949706191462));
#56435=CARTESIAN_POINT('Ctrl Pts',(-86.5499999999997,19.8922930183494,-46.4949706191462));
#56436=CARTESIAN_POINT('Ctrl Pts',(-85.59,23.3219850986922,-50.6740625107251));
#56437=CARTESIAN_POINT('Ctrl Pts',(-86.5499999999998,23.3219850986922,-50.6740625107251));
#56438=CARTESIAN_POINT('Ctrl Pts',(-85.5900000000001,25.9500938140347,-52.9242386124823));
#56439=CARTESIAN_POINT('Ctrl Pts',(-86.5499999999999,25.9500938140347,-52.9242386124823));
#56440=CARTESIAN_POINT('Ctrl Pts',(-85.5900000000001,27.17635626841,-53.820227589861));
#56441=CARTESIAN_POINT('Ctrl Pts',(-86.5499999999999,27.17635626841,-53.820227589861));
#56442=CARTESIAN_POINT('',(-85.5900000000001,27.1763562684562,-53.8202275898948));
#56443=CARTESIAN_POINT('Ctrl Pts',(-85.59,25.9087562733108,-56.6022465291596));
#56444=CARTESIAN_POINT('Ctrl Pts',(-86.5500000000001,25.9087562733108,-56.6022465291596));
#56445=CARTESIAN_POINT('Ctrl Pts',(-85.59,24.3707554345474,-55.5227304891486));
#56446=CARTESIAN_POINT('Ctrl Pts',(-86.5500000000001,24.3707554345474,-55.5227304891486));
#56447=CARTESIAN_POINT('Ctrl Pts',(-85.59,21.2915197248082,-52.9364267530472));
#56448=CARTESIAN_POINT('Ctrl Pts',(-86.5500000000001,21.2915197248082,-52.9364267530472));
#56449=CARTESIAN_POINT('Ctrl Pts',(-85.5900000000003,17.38180473866,-48.1724252583814));
#56450=CARTESIAN_POINT('Ctrl Pts',(-86.5500000000004,17.38180473866,-48.1724252583814));
#56451=CARTESIAN_POINT('Ctrl Pts',(-85.5900000000002,14.3591223335948,-42.5173842278733));
#56452=CARTESIAN_POINT('Ctrl Pts',(-86.5500000000003,14.3591223335948,-42.5173842278733));
#56453=CARTESIAN_POINT('Ctrl Pts',(-85.5900000000001,12.776944090006,-37.301641550967));
#56454=CARTESIAN_POINT('Ctrl Pts',(-86.5500000000002,12.776944090006,-37.301641550967));
#56455=CARTESIAN_POINT('Ctrl Pts',(-85.5900000000001,12.3088983373981,-34.0330589224049));
#56456=CARTESIAN_POINT('Ctrl Pts',(-86.5500000000002,12.3088983373981,-34.0330589224049));
#56457=CARTESIAN_POINT('Ctrl Pts',(-85.5900000000001,12.2056450723618,-32.8676240082902));
#56458=CARTESIAN_POINT('Ctrl Pts',(-86.5500000000002,12.2056450723618,-32.8676240082902));
#56459=CARTESIAN_POINT('',(-86.3899999999997,25.9087562733283,-56.6022465291718));
#56460=CARTESIAN_POINT('',(-85.5899999999997,12.2056450723663,-32.8676240083405));
#56461=CARTESIAN_POINT('Ctrl Pts',(-85.5900000000001,58.2818165781778,-59.4698569538907));
#56462=CARTESIAN_POINT('Ctrl Pts',(-86.5500000000001,58.2818165781778,-59.4698569538907));
#56463=CARTESIAN_POINT('Ctrl Pts',(-85.5900000000001,57.863878739489,-59.6642231184525));
#56464=CARTESIAN_POINT('Ctrl Pts',(-86.5500000000001,57.863878739489,-59.6642231184525));
#56465=CARTESIAN_POINT('Ctrl Pts',(-85.5900000000001,55.4939941495213,-60.7056460155525));
#56466=CARTESIAN_POINT('Ctrl Pts',(-86.5500000000001,55.4939941495213,-60.7056460155525));
#56467=CARTESIAN_POINT('Ctrl Pts',(-85.59,50.9600682432795,-62.0809974029323));
#56468=CARTESIAN_POINT('Ctrl Pts',(-86.5499999999999,50.9600682432795,-62.0809974029323));
#56469=CARTESIAN_POINT('Ctrl Pts',(-85.5900000000001,44.5787611019615,-62.7095012985338));
#56470=CARTESIAN_POINT('Ctrl Pts',(-86.55,44.5787611019615,-62.7095012985338));
#56471=CARTESIAN_POINT('Ctrl Pts',(-85.5900000000002,38.1974539606436,-62.0809974029323));
#56472=CARTESIAN_POINT('Ctrl Pts',(-86.5500000000001,38.1974539606436,-62.0809974029323));
#56473=CARTESIAN_POINT('Ctrl Pts',(-85.59,33.6635280544017,-60.7056460155525));
#56474=CARTESIAN_POINT('Ctrl Pts',(-86.55,33.6635280544017,-60.7056460155525));
#56475=CARTESIAN_POINT('Ctrl Pts',(-85.59,31.293643464434,-59.6642231184525));
#56476=CARTESIAN_POINT('Ctrl Pts',(-86.5499999999999,31.293643464434,-59.6642231184525));
#56477=CARTESIAN_POINT('Ctrl Pts',(-85.5899999999999,30.8757056257452,-59.4698569538907));
#56478=CARTESIAN_POINT('Ctrl Pts',(-86.5499999999999,30.8757056257452,-59.4698569538907));
#56479=CARTESIAN_POINT('',(-86.39,58.2818165781182,-59.4698569539184));
#56480=CARTESIAN_POINT('',(-85.5899999999998,30.8757056258048,-59.4698569539184));
#56481=CARTESIAN_POINT('Ctrl Pts',(-85.5900000000001,32.6508629759048,-56.9809939705197));
#56482=CARTESIAN_POINT('Ctrl Pts',(-86.55,32.6508629759048,-56.9809939705197));
#56483=CARTESIAN_POINT('Ctrl Pts',(-85.5900000000001,32.8626902557639,-57.074652602861));
#56484=CARTESIAN_POINT('Ctrl Pts',(-86.55,32.8626902557639,-57.074652602861));
#56485=CARTESIAN_POINT('Ctrl Pts',(-85.5900000000001,34.8506764348762,-57.9257562386733));
#56486=CARTESIAN_POINT('Ctrl Pts',(-86.55,34.8506764348762,-57.9257562386733));
#56487=CARTESIAN_POINT('Ctrl Pts',(-85.5900000000004,38.7864976967653,-59.1196745657386));
#56488=CARTESIAN_POINT('Ctrl Pts',(-86.5500000000003,38.7864976967653,-59.1196745657386));
#56489=CARTESIAN_POINT('Ctrl Pts',(-85.5900000000001,44.5787611019615,-59.6901627171307));
#56490=CARTESIAN_POINT('Ctrl Pts',(-86.5499999999999,44.5787611019615,-59.6901627171307));
#56491=CARTESIAN_POINT('Ctrl Pts',(-85.5900000000002,50.3710245071578,-59.1196745657386));
#56492=CARTESIAN_POINT('Ctrl Pts',(-86.55,50.3710245071578,-59.1196745657386));
#56493=CARTESIAN_POINT('Ctrl Pts',(-85.5900000000002,54.3068457690469,-57.9257562386733));
#56494=CARTESIAN_POINT('Ctrl Pts',(-86.5500000000001,54.3068457690469,-57.9257562386733));
#56495=CARTESIAN_POINT('Ctrl Pts',(-85.5900000000002,56.2948319481591,-57.0746526028609));
#56496=CARTESIAN_POINT('Ctrl Pts',(-86.5500000000001,56.2948319481591,-57.0746526028609));
#56497=CARTESIAN_POINT('Ctrl Pts',(-85.5900000000002,56.5066592280182,-56.9809939705197));
#56498=CARTESIAN_POINT('Ctrl Pts',(-86.5500000000001,56.5066592280182,-56.9809939705197));
#56499=CARTESIAN_POINT('',(-85.5900000000003,56.5066592279993,-56.9809939705281));
#56500=CARTESIAN_POINT('Ctrl Pts',(-85.5900000000001,56.0151454704998,-43.2460190022905));
#56501=CARTESIAN_POINT('Ctrl Pts',(-86.5500000000003,56.0151454704998,-43.2460190022905));
#56502=CARTESIAN_POINT('Ctrl Pts',(-85.5900000000001,56.3382988733641,-42.9670353333918));
#56503=CARTESIAN_POINT('Ctrl Pts',(-86.5500000000003,56.3382988733641,-42.9670353333918));
#56504=CARTESIAN_POINT('Ctrl Pts',(-85.59,57.4908812316947,-41.8960812765113));
#56505=CARTESIAN_POINT('Ctrl Pts',(-86.5500000000003,57.4908812316947,-41.8960812765113));
#56506=CARTESIAN_POINT('Ctrl Pts',(-85.59,59.2232760668162,-39.7851520622054));
#56507=CARTESIAN_POINT('Ctrl Pts',(-86.5500000000002,59.2232760668162,-39.7851520622054));
#56508=CARTESIAN_POINT('Ctrl Pts',(-85.59,60.8508742849283,-36.7401299688548));
#56509=CARTESIAN_POINT('Ctrl Pts',(-86.5500000000002,60.8508742849283,-36.7401299688548));
#56510=CARTESIAN_POINT('Ctrl Pts',(-85.5900000000002,61.5322159292861,-34.4940475780554));
#56511=CARTESIAN_POINT('Ctrl Pts',(-86.5500000000004,61.5322159292861,-34.4940475780554));
#56512=CARTESIAN_POINT('Ctrl Pts',(-85.5900000000002,61.7599375519114,-33.325536359296));
#56513=CARTESIAN_POINT('Ctrl Pts',(-86.5500000000004,61.7599375519114,-33.325536359296));
#56514=CARTESIAN_POINT('Ctrl Pts',(-85.5900000000002,61.7683968689589,-33.2812143326691));
#56515=CARTESIAN_POINT('Ctrl Pts',(-86.5500000000004,61.7683968689589,-33.2812143326691));
#56516=CARTESIAN_POINT('',(-85.5900000000001,61.7683968689589,-33.2812143326695));
#56517=CARTESIAN_POINT('',(-86.3900000000002,56.0151454704896,-43.2460190022993));
#56518=CARTESIAN_POINT('Ctrl Pts',(-85.5900000000001,64.887199765057,-32.7955273866341));
#56519=CARTESIAN_POINT('Ctrl Pts',(-86.55,64.887199765057,-32.7955273866341));
#56520=CARTESIAN_POINT('Ctrl Pts',(-85.5900000000001,64.8317241957022,-33.198694346047));
#56521=CARTESIAN_POINT('Ctrl Pts',(-86.55,64.8317241957022,-33.198694346047));
#56522=CARTESIAN_POINT('Ctrl Pts',(-85.59,64.5418111191122,-34.923958693842));
#56523=CARTESIAN_POINT('Ctrl Pts',(-86.5499999999999,64.5418111191122,-34.923958693842));
#56524=CARTESIAN_POINT('Ctrl Pts',(-85.59,63.6403794020083,-37.8955808206585));
#56525=CARTESIAN_POINT('Ctrl Pts',(-86.5499999999999,63.6403794020083,-37.8955808206585));
#56526=CARTESIAN_POINT('Ctrl Pts',(-85.5900000000001,61.7337643465056,-41.4626067014406));
#56527=CARTESIAN_POINT('Ctrl Pts',(-86.55,61.7337643465056,-41.4626067014406));
#56528=CARTESIAN_POINT('Ctrl Pts',(-85.5900000000001,59.4786368856762,-44.2104874631114));
#56529=CARTESIAN_POINT('Ctrl Pts',(-86.55,59.4786368856762,-44.2104874631114));
#56530=CARTESIAN_POINT('Ctrl Pts',(-85.59,57.8284952042209,-45.6658884897885));
#56531=CARTESIAN_POINT('Ctrl Pts',(-86.5499999999999,57.8284952042209,-45.6658884897885));
#56532=CARTESIAN_POINT('Ctrl Pts',(-85.59,57.1538693431349,-46.1899302405967));
#56533=CARTESIAN_POINT('Ctrl Pts',(-86.5499999999999,57.1538693431349,-46.1899302405967));
#56534=CARTESIAN_POINT('',(-86.3900000000002,64.8871997650542,-32.795527386655));
#56535=CARTESIAN_POINT('Ctrl Pts',(-85.5900000000003,61.7683968689589,-26.7187856673309));
#56536=CARTESIAN_POINT('Ctrl Pts',(-86.5500000000003,61.7683968689589,-26.7187856673309));
#56537=CARTESIAN_POINT('Ctrl Pts',(-85.5900000000003,61.7599375519114,-26.674463640704));
#56538=CARTESIAN_POINT('Ctrl Pts',(-86.5500000000003,61.7599375519114,-26.674463640704));
#56539=CARTESIAN_POINT('Ctrl Pts',(-85.5900000000003,61.5322159292861,-25.5059524219446));
#56540=CARTESIAN_POINT('Ctrl Pts',(-86.5500000000004,61.5322159292861,-25.5059524219446));
#56541=CARTESIAN_POINT('Ctrl Pts',(-85.5900000000004,60.8508742849282,-23.2598700311452));
#56542=CARTESIAN_POINT('Ctrl Pts',(-86.5500000000004,60.8508742849282,-23.2598700311452));
#56543=CARTESIAN_POINT('Ctrl Pts',(-85.5900000000003,59.2232760668162,-20.2148479377946));
#56544=CARTESIAN_POINT('Ctrl Pts',(-86.5500000000003,59.2232760668162,-20.2148479377946));
#56545=CARTESIAN_POINT('Ctrl Pts',(-85.5900000000002,57.4908812316947,-18.1039187234887));
#56546=CARTESIAN_POINT('Ctrl Pts',(-86.5500000000002,57.4908812316947,-18.1039187234887));
#56547=CARTESIAN_POINT('Ctrl Pts',(-85.5900000000003,56.3382988733641,-17.0329646666082));
#56548=CARTESIAN_POINT('Ctrl Pts',(-86.5500000000004,56.3382988733641,-17.0329646666082));
#56549=CARTESIAN_POINT('Ctrl Pts',(-85.5900000000004,56.0151454704999,-16.7539809977095));
#56550=CARTESIAN_POINT('Ctrl Pts',(-86.5500000000004,56.0151454704999,-16.7539809977095));
#56551=CARTESIAN_POINT('',(-85.59,56.0151454704897,-16.7539809977007));
#56552=CARTESIAN_POINT('',(-86.3900000000002,61.7683968689589,-26.7187856673305));
#56553=CARTESIAN_POINT('Ctrl Pts',(-85.5900000000001,57.1538693431349,-13.8100697594034));
#56554=CARTESIAN_POINT('Ctrl Pts',(-86.55,57.1538693431349,-13.8100697594034));
#56555=CARTESIAN_POINT('Ctrl Pts',(-85.5900000000001,57.8284952042209,-14.3341115102115));
#56556=CARTESIAN_POINT('Ctrl Pts',(-86.55,57.8284952042209,-14.3341115102115));
#56557=CARTESIAN_POINT('Ctrl Pts',(-85.5900000000001,59.4786368856762,-15.7895125368886));
#56558=CARTESIAN_POINT('Ctrl Pts',(-86.55,59.4786368856762,-15.7895125368886));
#56559=CARTESIAN_POINT('Ctrl Pts',(-85.5900000000001,61.7337643465056,-18.5373932985594));
#56560=CARTESIAN_POINT('Ctrl Pts',(-86.55,61.7337643465056,-18.5373932985594));
#56561=CARTESIAN_POINT('Ctrl Pts',(-85.59,63.6403794020083,-22.1044191793415));
#56562=CARTESIAN_POINT('Ctrl Pts',(-86.5499999999999,63.6403794020083,-22.1044191793415));
#56563=CARTESIAN_POINT('Ctrl Pts',(-85.59,64.5418111191123,-25.076041306158));
#56564=CARTESIAN_POINT('Ctrl Pts',(-86.5499999999999,64.5418111191123,-25.076041306158));
#56565=CARTESIAN_POINT('Ctrl Pts',(-85.59,64.8317241957022,-26.801305653953));
#56566=CARTESIAN_POINT('Ctrl Pts',(-86.5499999999999,64.8317241957022,-26.801305653953));
#56567=CARTESIAN_POINT('Ctrl Pts',(-85.59,64.8871997650571,-27.2044726133659));
#56568=CARTESIAN_POINT('Ctrl Pts',(-86.5499999999999,64.8871997650571,-27.2044726133659));
#56569=CARTESIAN_POINT('',(-85.5900000000001,64.8871997650542,-27.204472613345));
#56570=CARTESIAN_POINT('Ctrl Pts',(-85.5899999999996,44.5787611019615,-12.5));
#56571=CARTESIAN_POINT('Ctrl Pts',(-86.5500000000004,44.5787611019615,-12.5));
#56572=CARTESIAN_POINT('Ctrl Pts',(-85.5899999999996,43.433398281725,-12.5));
#56573=CARTESIAN_POINT('Ctrl Pts',(-86.5500000000004,43.433398281725,-12.5));
#56574=CARTESIAN_POINT('Ctrl Pts',(-85.5899999999999,41.4793849491346,-12.6924535153054));
#56575=CARTESIAN_POINT('Ctrl Pts',(-86.5500000000007,41.4793849491346,-12.6924535153054));
#56576=CARTESIAN_POINT('Ctrl Pts',(-85.5899999999998,39.5894255810997,-13.2069280562477));
#56577=CARTESIAN_POINT('Ctrl Pts',(-86.5500000000005,39.5894255810997,-13.2069280562477));
#56578=CARTESIAN_POINT('Ctrl Pts',(-85.5899999999997,38.8257008878975,-13.4727301359734));
#56579=CARTESIAN_POINT('Ctrl Pts',(-86.5500000000005,38.8257008878975,-13.4727301359734));
#56580=CARTESIAN_POINT('Ctrl Pts',(-85.5900000000001,44.5787611019615,-9.5));
#56581=CARTESIAN_POINT('Ctrl Pts',(-86.5500000000001,44.5787611019615,-9.5));
#56582=CARTESIAN_POINT('Ctrl Pts',(-85.5900000000001,45.9204718342386,-9.5));
#56583=CARTESIAN_POINT('Ctrl Pts',(-86.5500000000001,45.9204718342386,-9.5));
#56584=CARTESIAN_POINT('Ctrl Pts',(-85.59,48.5636521071579,-9.76033053440579));
#56585=CARTESIAN_POINT('Ctrl Pts',(-86.55,48.5636521071579,-9.76033053440579));
#56586=CARTESIAN_POINT('Ctrl Pts',(-85.5900000000001,51.1067797000701,-10.5236598583039));
#56587=CARTESIAN_POINT('Ctrl Pts',(-86.5500000000002,51.1067797000701,-10.5236598583039));
#56588=CARTESIAN_POINT('Ctrl Pts',(-85.5900000000002,52.3121016228057,-11.0146003457735));
#56589=CARTESIAN_POINT('Ctrl Pts',(-86.5500000000002,52.3121016228057,-11.0146003457735));
#56590=CARTESIAN_POINT('',(-85.5900000000002,52.3121016227476,-11.0146003457498));
#56591=CARTESIAN_POINT('Ctrl Pts',(-85.5900000000001,33.1423767334232,-16.7539809977095));
#56592=CARTESIAN_POINT('Ctrl Pts',(-86.5500000000006,33.1423767334232,-16.7539809977095));
#56593=CARTESIAN_POINT('Ctrl Pts',(-85.5900000000001,32.819223330559,-17.0329646666082));
#56594=CARTESIAN_POINT('Ctrl Pts',(-86.5500000000006,32.819223330559,-17.0329646666082));
#56595=CARTESIAN_POINT('Ctrl Pts',(-85.5900000000001,31.6666409722284,-18.1039187234887));
#56596=CARTESIAN_POINT('Ctrl Pts',(-86.5500000000006,31.6666409722284,-18.1039187234887));
#56597=CARTESIAN_POINT('Ctrl Pts',(-85.59,29.9342461371069,-20.2148479377946));
#56598=CARTESIAN_POINT('Ctrl Pts',(-86.5500000000005,29.9342461371069,-20.2148479377946));
#56599=CARTESIAN_POINT('Ctrl Pts',(-85.5900000000004,28.3066479189948,-23.2598700311452));
#56600=CARTESIAN_POINT('Ctrl Pts',(-86.5500000000009,28.3066479189948,-23.2598700311452));
#56601=CARTESIAN_POINT('Ctrl Pts',(-85.5900000000002,27.6253062746369,-25.5059524219446));
#56602=CARTESIAN_POINT('Ctrl Pts',(-86.5500000000007,27.6253062746369,-25.5059524219446));
#56603=CARTESIAN_POINT('Ctrl Pts',(-85.5900000000002,27.3975846520116,-26.674463640704));
#56604=CARTESIAN_POINT('Ctrl Pts',(-86.5500000000007,27.3975846520116,-26.674463640704));
#56605=CARTESIAN_POINT('Ctrl Pts',(-85.5900000000002,27.3891253349641,-26.7187856673309));
#56606=CARTESIAN_POINT('Ctrl Pts',(-86.5500000000007,27.3891253349641,-26.7187856673309));
#56607=CARTESIAN_POINT('',(-86.3900000000002,33.1423767334334,-16.7539809977007));
#56608=CARTESIAN_POINT('Ctrl Pts',(-85.59,24.270322438866,-27.2044726133659));
#56609=CARTESIAN_POINT('Ctrl Pts',(-86.55,24.270322438866,-27.2044726133659));
#56610=CARTESIAN_POINT('Ctrl Pts',(-85.59,24.3257980082209,-26.801305653953));
#56611=CARTESIAN_POINT('Ctrl Pts',(-86.55,24.3257980082209,-26.801305653953));
#56612=CARTESIAN_POINT('Ctrl Pts',(-85.59,24.6157110848108,-25.076041306158));
#56613=CARTESIAN_POINT('Ctrl Pts',(-86.55,24.6157110848108,-25.076041306158));
#56614=CARTESIAN_POINT('Ctrl Pts',(-85.5900000000001,25.5171428019148,-22.1044191793415));
#56615=CARTESIAN_POINT('Ctrl Pts',(-86.5500000000001,25.5171428019148,-22.1044191793415));
#56616=CARTESIAN_POINT('Ctrl Pts',(-85.59,27.4237578574175,-18.5373932985594));
#56617=CARTESIAN_POINT('Ctrl Pts',(-86.55,27.4237578574175,-18.5373932985594));
#56618=CARTESIAN_POINT('Ctrl Pts',(-85.59,29.6788853182468,-15.7895125368886));
#56619=CARTESIAN_POINT('Ctrl Pts',(-86.55,29.6788853182468,-15.7895125368886));
#56620=CARTESIAN_POINT('Ctrl Pts',(-85.59,31.3290269997022,-14.3341115102115));
#56621=CARTESIAN_POINT('Ctrl Pts',(-86.55,31.3290269997022,-14.3341115102115));
#56622=CARTESIAN_POINT('Ctrl Pts',(-85.59,32.0036528607881,-13.8100697594033));
#56623=CARTESIAN_POINT('Ctrl Pts',(-86.55,32.0036528607881,-13.8100697594033));
#56624=CARTESIAN_POINT('',(-86.3899999999999,24.2703224388689,-27.2044726133451));
#56625=CARTESIAN_POINT('',(-85.59,32.0036528607784,-13.8100697594109));
#56626=CARTESIAN_POINT('Ctrl Pts',(-85.5900000000002,27.3891253349641,-33.281214332669));
#56627=CARTESIAN_POINT('Ctrl Pts',(-86.5500000000002,27.3891253349641,-33.281214332669));
#56628=CARTESIAN_POINT('Ctrl Pts',(-85.5900000000002,27.3975846520116,-33.3255363592959));
#56629=CARTESIAN_POINT('Ctrl Pts',(-86.5500000000002,27.3975846520116,-33.3255363592959));
#56630=CARTESIAN_POINT('Ctrl Pts',(-85.5900000000001,27.6253062746369,-34.4940475780554));
#56631=CARTESIAN_POINT('Ctrl Pts',(-86.5500000000002,27.6253062746369,-34.4940475780554));
#56632=CARTESIAN_POINT('Ctrl Pts',(-85.5900000000001,28.3066479189948,-36.7401299688549));
#56633=CARTESIAN_POINT('Ctrl Pts',(-86.5500000000001,28.3066479189948,-36.7401299688549));
#56634=CARTESIAN_POINT('Ctrl Pts',(-85.5900000000001,29.9342461371069,-39.7851520622054));
#56635=CARTESIAN_POINT('Ctrl Pts',(-86.5500000000001,29.9342461371069,-39.7851520622054));
#56636=CARTESIAN_POINT('Ctrl Pts',(-85.5900000000001,31.6666409722284,-41.8960812765113));
#56637=CARTESIAN_POINT('Ctrl Pts',(-86.5500000000002,31.6666409722284,-41.8960812765113));
#56638=CARTESIAN_POINT('Ctrl Pts',(-85.5900000000001,32.8192233305589,-42.9670353333918));
#56639=CARTESIAN_POINT('Ctrl Pts',(-86.5500000000002,32.8192233305589,-42.9670353333918));
#56640=CARTESIAN_POINT('Ctrl Pts',(-85.5900000000001,33.1423767334232,-43.2460190022905));
#56641=CARTESIAN_POINT('Ctrl Pts',(-86.5500000000002,33.1423767334232,-43.2460190022905));
#56642=CARTESIAN_POINT('',(-85.5900000000001,33.1423767334334,-43.2460190022993));
#56643=CARTESIAN_POINT('Ctrl Pts',(-85.5900000000001,32.0036528607881,-46.1899302405967));
#56644=CARTESIAN_POINT('Ctrl Pts',(-86.55,32.0036528607881,-46.1899302405967));
#56645=CARTESIAN_POINT('Ctrl Pts',(-85.59,31.3290269997021,-45.6658884897885));
#56646=CARTESIAN_POINT('Ctrl Pts',(-86.5499999999999,31.3290269997021,-45.6658884897885));
#56647=CARTESIAN_POINT('Ctrl Pts',(-85.5899999999999,29.6788853182468,-44.2104874631114));
#56648=CARTESIAN_POINT('Ctrl Pts',(-86.5499999999997,29.6788853182468,-44.2104874631114));
#56649=CARTESIAN_POINT('Ctrl Pts',(-85.5900000000001,27.4237578574175,-41.4626067014406));
#56650=CARTESIAN_POINT('Ctrl Pts',(-86.5499999999999,27.4237578574175,-41.4626067014406));
#56651=CARTESIAN_POINT('Ctrl Pts',(-85.5899999999997,25.5171428019148,-37.8955808206585));
#56652=CARTESIAN_POINT('Ctrl Pts',(-86.5499999999996,25.5171428019148,-37.8955808206585));
#56653=CARTESIAN_POINT('Ctrl Pts',(-85.5900000000001,24.6157110848108,-34.923958693842));
#56654=CARTESIAN_POINT('Ctrl Pts',(-86.55,24.6157110848108,-34.923958693842));
#56655=CARTESIAN_POINT('Ctrl Pts',(-85.5900000000001,24.3257980082209,-33.198694346047));
#56656=CARTESIAN_POINT('Ctrl Pts',(-86.55,24.3257980082209,-33.198694346047));
#56657=CARTESIAN_POINT('Ctrl Pts',(-85.5900000000001,24.270322438866,-32.7955273866341));
#56658=CARTESIAN_POINT('Ctrl Pts',(-86.5499999999999,24.270322438866,-32.7955273866341));
#56659=CARTESIAN_POINT('',(-86.39,32.0036528607783,-46.189930240589));
#56660=CARTESIAN_POINT('',(-85.5900000000001,24.2703224388689,-32.7955273866549));
#56661=CARTESIAN_POINT('Ctrl Pts',(-85.59,52.3121016227473,-48.9853996542503));
#56662=CARTESIAN_POINT('Ctrl Pts',(-86.5500000000001,52.3121016227473,-48.9853996542503));
#56663=CARTESIAN_POINT('Ctrl Pts',(-85.5900000000001,51.1067797000296,-49.4763401417082));
#56664=CARTESIAN_POINT('Ctrl Pts',(-86.5500000000001,51.1067797000296,-49.4763401417082));
#56665=CARTESIAN_POINT('Ctrl Pts',(-85.5900000000001,48.5636521071369,-50.2396694655963));
#56666=CARTESIAN_POINT('Ctrl Pts',(-86.5500000000002,48.5636521071369,-50.2396694655963));
#56667=CARTESIAN_POINT('Ctrl Pts',(-85.59,44.5787611019615,-50.6321469729213));
#56668=CARTESIAN_POINT('Ctrl Pts',(-86.55,44.5787611019615,-50.6321469729213));
#56669=CARTESIAN_POINT('Ctrl Pts',(-85.5900000000002,40.5938700967862,-50.2396694655963));
#56670=CARTESIAN_POINT('Ctrl Pts',(-86.5500000000002,40.5938700967862,-50.2396694655963));
#56671=CARTESIAN_POINT('Ctrl Pts',(-85.59,38.0507425038934,-49.4763401417082));
#56672=CARTESIAN_POINT('Ctrl Pts',(-86.5500000000001,38.0507425038934,-49.4763401417082));
#56673=CARTESIAN_POINT('Ctrl Pts',(-85.59,36.8454205811756,-48.9853996542502));
#56674=CARTESIAN_POINT('Ctrl Pts',(-86.5500000000001,36.8454205811756,-48.9853996542502));
#56675=CARTESIAN_POINT('',(-86.39,52.3121016227475,-48.9853996542502));
#56676=CARTESIAN_POINT('',(-85.5900000000001,36.8454205811755,-48.9853996542502));
#56677=CARTESIAN_POINT('Ctrl Pts',(-85.5900000000001,38.825700926836,-46.5272698775785));
#56678=CARTESIAN_POINT('Ctrl Pts',(-86.5500000000004,38.825700926836,-46.5272698775785));
#56679=CARTESIAN_POINT('Ctrl Pts',(-85.5900000000001,39.5894256076847,-46.7930719509892));
#56680=CARTESIAN_POINT('Ctrl Pts',(-86.5500000000005,39.5894256076847,-46.7930719509892));
#56681=CARTESIAN_POINT('Ctrl Pts',(-85.5900000000002,41.4793849628776,-47.3075464860481));
#56682=CARTESIAN_POINT('Ctrl Pts',(-86.5500000000006,41.4793849628776,-47.3075464860481));
#56683=CARTESIAN_POINT('Ctrl Pts',(-85.5900000000001,44.5787611019615,-47.6128083915182));
#56684=CARTESIAN_POINT('Ctrl Pts',(-86.5500000000004,44.5787611019615,-47.6128083915182));
#56685=CARTESIAN_POINT('Ctrl Pts',(-85.5900000000004,47.6781372410454,-47.3075464860481));
#56686=CARTESIAN_POINT('Ctrl Pts',(-86.5500000000007,47.6781372410454,-47.3075464860481));
#56687=CARTESIAN_POINT('Ctrl Pts',(-85.5900000000002,49.5680965962383,-46.7930719509892));
#56688=CARTESIAN_POINT('Ctrl Pts',(-86.5500000000005,49.5680965962383,-46.7930719509892));
#56689=CARTESIAN_POINT('Ctrl Pts',(-85.5900000000001,50.331821277087,-46.5272698775786));
#56690=CARTESIAN_POINT('Ctrl Pts',(-86.5500000000004,50.331821277087,-46.5272698775786));
#56691=CARTESIAN_POINT('',(-85.59,50.3318212771098,-46.5272698775706));
#56692=CARTESIAN_POINT('Ctrl Pts',(-85.5900000000003,52.1693515320407,-32.5263626850653));
#56693=CARTESIAN_POINT('Ctrl Pts',(-86.5499999999999,52.1693515320407,-32.5263626850653));
#56694=CARTESIAN_POINT('Ctrl Pts',(-85.5900000000003,52.1092282262322,-32.7070306040739));
#56695=CARTESIAN_POINT('Ctrl Pts',(-86.5499999999999,52.1092282262322,-32.7070306040739));
#56696=CARTESIAN_POINT('Ctrl Pts',(-85.5900000000003,51.8596181813079,-33.3764687724939));
#56697=CARTESIAN_POINT('Ctrl Pts',(-86.5499999999999,51.8596181813079,-33.3764687724939));
#56698=CARTESIAN_POINT('Ctrl Pts',(-85.5900000000005,51.3485297861136,-34.3326479066949));
#56699=CARTESIAN_POINT('Ctrl Pts',(-86.55,51.3485297861136,-34.3326479066949));
#56700=CARTESIAN_POINT('Ctrl Pts',(-85.5900000000003,50.8041422375712,-35.0375762026026));
#56701=CARTESIAN_POINT('Ctrl Pts',(-86.5499999999999,50.8041422375712,-35.0375762026026));
#56702=CARTESIAN_POINT('Ctrl Pts',(-85.5900000000003,50.5618748736091,-35.3105548553452));
#56703=CARTESIAN_POINT('Ctrl Pts',(-86.5499999999999,50.5618748736091,-35.3105548553452));
#56704=CARTESIAN_POINT('',(-86.3899999999999,52.1693515320421,-32.5263626850612));
#56705=CARTESIAN_POINT('Ctrl Pts',(-85.5900000000001,50.5618748736091,-24.6894451446548));
#56706=CARTESIAN_POINT('Ctrl Pts',(-86.5499999999996,50.5618748736091,-24.6894451446548));
#56707=CARTESIAN_POINT('Ctrl Pts',(-85.5900000000001,50.8041422375712,-24.9624237973974));
#56708=CARTESIAN_POINT('Ctrl Pts',(-86.5499999999996,50.8041422375712,-24.9624237973974));
#56709=CARTESIAN_POINT('Ctrl Pts',(-85.59,51.3485297861136,-25.6673520933051));
#56710=CARTESIAN_POINT('Ctrl Pts',(-86.5499999999995,51.3485297861136,-25.6673520933051));
#56711=CARTESIAN_POINT('Ctrl Pts',(-85.59,51.8596181813079,-26.6235312275061));
#56712=CARTESIAN_POINT('Ctrl Pts',(-86.5499999999994,51.8596181813079,-26.6235312275061));
#56713=CARTESIAN_POINT('Ctrl Pts',(-85.59,52.1092282262323,-27.2929693959262));
#56714=CARTESIAN_POINT('Ctrl Pts',(-86.5499999999995,52.1092282262323,-27.2929693959262));
#56715=CARTESIAN_POINT('Ctrl Pts',(-85.59,52.1693515320408,-27.4736373149347));
#56716=CARTESIAN_POINT('Ctrl Pts',(-86.5499999999995,52.1693515320408,-27.4736373149347));
#56717=CARTESIAN_POINT('',(-85.5900000000002,52.1693515320421,-27.4736373149388));
#56718=CARTESIAN_POINT('Ctrl Pts',(-85.5900000000004,44.5787611019615,-22.));
#56719=CARTESIAN_POINT('Ctrl Pts',(-86.55,44.5787611019615,-22.));
#56720=CARTESIAN_POINT('Ctrl Pts',(-85.5900000000005,45.1023555340697,-22.));
#56721=CARTESIAN_POINT('Ctrl Pts',(-86.55,45.1023555340697,-22.));
#56722=CARTESIAN_POINT('Ctrl Pts',(-85.5900000000004,45.6418375870485,-22.0531343444839));
#56723=CARTESIAN_POINT('Ctrl Pts',(-86.55,45.6418375870485,-22.0531343444839));
#56724=CARTESIAN_POINT('Ctrl Pts',(-85.5900000000003,46.1706391043629,-22.1599633677105));
#56725=CARTESIAN_POINT('Ctrl Pts',(-86.5499999999998,46.1706391043629,-22.1599633677105));
#56726=CARTESIAN_POINT('Ctrl Pts',(-85.5900000000003,46.1862026525634,-22.1631559443817));
#56727=CARTESIAN_POINT('Ctrl Pts',(-86.5499999999998,46.1862026525634,-22.1631559443817));
#56728=CARTESIAN_POINT('',(-85.5900000000003,46.1862026525626,-22.1631559443816));
#56729=CARTESIAN_POINT('Ctrl Pts',(-85.5900000000003,36.9881706718823,-27.4736373149347));
#56730=CARTESIAN_POINT('Ctrl Pts',(-86.5499999999998,36.9881706718823,-27.4736373149347));
#56731=CARTESIAN_POINT('Ctrl Pts',(-85.5900000000003,37.0482939776908,-27.2929693959261));
#56732=CARTESIAN_POINT('Ctrl Pts',(-86.5499999999999,37.0482939776908,-27.2929693959261));
#56733=CARTESIAN_POINT('Ctrl Pts',(-85.5900000000004,37.2979040226152,-26.6235312275061));
#56734=CARTESIAN_POINT('Ctrl Pts',(-86.5499999999999,37.2979040226152,-26.6235312275061));
#56735=CARTESIAN_POINT('Ctrl Pts',(-85.5900000000002,37.8089924178094,-25.6673520933051));
#56736=CARTESIAN_POINT('Ctrl Pts',(-86.5499999999997,37.8089924178094,-25.6673520933051));
#56737=CARTESIAN_POINT('Ctrl Pts',(-85.5900000000003,38.3533799663518,-24.9624237973974));
#56738=CARTESIAN_POINT('Ctrl Pts',(-86.5499999999998,38.3533799663518,-24.9624237973974));
#56739=CARTESIAN_POINT('Ctrl Pts',(-85.5900000000003,38.5956473303139,-24.6894451446548));
#56740=CARTESIAN_POINT('Ctrl Pts',(-86.5499999999998,38.5956473303139,-24.6894451446548));
#56741=CARTESIAN_POINT('',(-86.3899999999997,36.988170671881,-27.4736373149387));
#56742=CARTESIAN_POINT('',(-85.5900000000003,38.5956473303199,-24.6894451446481));
#56743=CARTESIAN_POINT('Ctrl Pts',(-85.5900000000007,38.5956473303139,-35.3105548553452));
#56744=CARTESIAN_POINT('Ctrl Pts',(-86.5499999999998,38.5956473303139,-35.3105548553452));
#56745=CARTESIAN_POINT('Ctrl Pts',(-85.5900000000006,38.3533799663518,-35.0375762026026));
#56746=CARTESIAN_POINT('Ctrl Pts',(-86.5499999999997,38.3533799663518,-35.0375762026026));
#56747=CARTESIAN_POINT('Ctrl Pts',(-85.5900000000005,37.8089924178094,-34.3326479066949));
#56748=CARTESIAN_POINT('Ctrl Pts',(-86.5499999999996,37.8089924178094,-34.3326479066949));
#56749=CARTESIAN_POINT('Ctrl Pts',(-85.5900000000008,37.2979040226152,-33.3764687724939));
#56750=CARTESIAN_POINT('Ctrl Pts',(-86.5499999999999,37.2979040226152,-33.3764687724939));
#56751=CARTESIAN_POINT('Ctrl Pts',(-85.5900000000007,37.0482939776908,-32.7070306040739));
#56752=CARTESIAN_POINT('Ctrl Pts',(-86.5499999999999,37.0482939776908,-32.7070306040739));
#56753=CARTESIAN_POINT('Ctrl Pts',(-85.5900000000007,36.9881706718823,-32.5263626850653));
#56754=CARTESIAN_POINT('Ctrl Pts',(-86.5499999999998,36.9881706718823,-32.5263626850653));
#56755=CARTESIAN_POINT('',(-86.3899999999999,38.5956473303199,-35.3105548553519));
#56756=CARTESIAN_POINT('',(-85.5900000000003,36.988170671881,-32.5263626850613));
#56757=CARTESIAN_POINT('Ctrl Pts',(-85.5900000000002,46.1862026525626,-37.8368440556185));
#56758=CARTESIAN_POINT('Ctrl Pts',(-86.5499999999997,46.1862026525626,-37.8368440556185));
#56759=CARTESIAN_POINT('Ctrl Pts',(-85.5900000000002,46.1706391043624,-37.8400366322896));
#56760=CARTESIAN_POINT('Ctrl Pts',(-86.5499999999997,46.1706391043624,-37.8400366322896));
#56761=CARTESIAN_POINT('Ctrl Pts',(-85.5900000000001,45.6418375870482,-37.9468656555161));
#56762=CARTESIAN_POINT('Ctrl Pts',(-86.5499999999996,45.6418375870482,-37.9468656555161));
#56763=CARTESIAN_POINT('Ctrl Pts',(-85.5900000000003,44.5787611019615,-38.0515695504083));
#56764=CARTESIAN_POINT('Ctrl Pts',(-86.5499999999997,44.5787611019615,-38.0515695504083));
#56765=CARTESIAN_POINT('Ctrl Pts',(-85.5900000000001,43.5156846168748,-37.9468656555161));
#56766=CARTESIAN_POINT('Ctrl Pts',(-86.5499999999996,43.5156846168748,-37.9468656555161));
#56767=CARTESIAN_POINT('Ctrl Pts',(-85.5900000000002,42.9868830995607,-37.8400366322896));
#56768=CARTESIAN_POINT('Ctrl Pts',(-86.5499999999997,42.9868830995607,-37.8400366322896));
#56769=CARTESIAN_POINT('Ctrl Pts',(-85.5900000000002,42.9713195513605,-37.8368440556185));
#56770=CARTESIAN_POINT('Ctrl Pts',(-86.5499999999997,42.9713195513605,-37.8368440556185));
#56771=CARTESIAN_POINT('',(-86.3899999999996,46.1862026525626,-37.8368440556185));
#56772=CARTESIAN_POINT('',(-85.5900000000001,42.9713195513605,-37.8368440556185));
#56773=CARTESIAN_POINT('Origin',(-85.9899999999996,53.5926110635042,-32.9999999999999));
#56774=CARTESIAN_POINT('Origin',(-85.9899999999997,66.3731980659926,-33.));
#56775=CARTESIAN_POINT('Origin',(-85.9899999999997,60.2949931567668,-33.));
#56776=CARTESIAN_POINT('Origin',(-85.99,78.4460245797131,-33.));
#56777=CARTESIAN_POINT('Origin',(-85.99,72.4174689786827,-33.));
#56778=CARTESIAN_POINT('Origin',(-85.9900000000002,66.3683162666315,-61.7406166195334));
#56779=CARTESIAN_POINT('Origin',(-85.9899999998252,61.1722799429393,-64.740817708925));
#56780=CARTESIAN_POINT('Origin',(-85.9899999999997,22.7892059208967,-61.7406166479301));
#56781=CARTESIAN_POINT('Origin',(-85.9900000000002,22.789205939653,1.74061661544304));
#56782=CARTESIAN_POINT('Origin',(-85.99,61.1722800421212,4.74081788071294));
#56783=CARTESIAN_POINT('Origin',(-85.990000000157,66.3683162853859,1.74061665201678));
#56784=CARTESIAN_POINT('Origin',(-85.9900000000001,82.9621121574678,-27.));
#56785=CARTESIAN_POINT('Origin',(-85.9900000000747,82.9621122252415,-33.));
#56786=CARTESIAN_POINT('Origin',(-85.9899999999998,30.2431724514241,0.829967899138609));
#56787=CARTESIAN_POINT('Origin',(-85.9899999999996,58.9143497524989,-60.8299678991386));
#56788=CARTESIAN_POINT('Origin',(-85.9899999999992,30.2431724514241,-60.8299678991386));
#56789=CARTESIAN_POINT('Origin',(-85.9899999999993,25.0470014756374,-57.8300000340158));
#56790=CARTESIAN_POINT('Origin',(-85.9899999999993,10.7114976242099,-33.));
#56791=CARTESIAN_POINT('Origin',(-85.9899999999996,10.7114976242099,-27.));
#56792=CARTESIAN_POINT('Origin',(-85.9899999999995,25.0470014756374,-2.16999996598413));
#56793=CARTESIAN_POINT('Origin',(-85.9899999999996,58.914349752499,0.829967899138591));
#56794=CARTESIAN_POINT('Origin',(-85.9899999999997,78.4460245797131,-27.));
#56795=CARTESIAN_POINT('Origin',(-85.9899999999993,61.0962221090322,-52.6090816762843));
#56796=CARTESIAN_POINT('Origin',(-85.9899999999997,55.9000854795073,-55.6091090308774));
#56797=CARTESIAN_POINT('Origin',(-85.9899999999995,28.0613000948908,-52.6090816762843));
#56798=CARTESIAN_POINT('Origin',(-85.9899999999995,28.0613000948908,-7.39091832371568));
#56799=CARTESIAN_POINT('Origin',(-85.9899999999996,55.9000854795073,-4.39089096912261));
#56800=CARTESIAN_POINT('Origin',(-85.9899999999996,61.0962221090323,-7.39091832371568));
#56801=CARTESIAN_POINT('Origin',(-85.9899999999997,72.4174689786827,-27.));
#56802=CARTESIAN_POINT('Origin',(-85.9899999999997,36.2795905006212,-9.62541485779656));
#56803=CARTESIAN_POINT('Origin',(-85.9899999999996,52.8779317033019,-50.3745851422034));
#56804=CARTESIAN_POINT('Origin',(-85.9899999999998,36.2795905006212,-50.3745851422034));
#56805=CARTESIAN_POINT('Origin',(-85.9899999999997,31.0834721426076,-47.3745261404244));
#56806=CARTESIAN_POINT('Origin',(-85.9899999999996,22.7843241379305,-33.));
#56807=CARTESIAN_POINT('Origin',(-85.9899999999995,22.7843241379304,-27.));
#56808=CARTESIAN_POINT('Origin',(-85.9899999999996,31.0834721426076,-12.6254738595756));
#56809=CARTESIAN_POINT('Origin',(-85.99,52.8779317033019,-9.62541485779658));
#56810=CARTESIAN_POINT('Origin',(-85.9899999999997,66.3731980659926,-27.));
#56811=CARTESIAN_POINT('Origin',(-85.9899999999998,55.0349236943356,-42.110604862193));
#56812=CARTESIAN_POINT('Origin',(-85.9899999999998,49.8387777318655,-45.1106160516509));
#56813=CARTESIAN_POINT('Origin',(-85.9899999999997,34.1225985095874,-42.110604862193));
#56814=CARTESIAN_POINT('Origin',(-85.9899999999997,34.1225985095875,-17.889395137807));
#56815=CARTESIAN_POINT('Origin',(-85.9899999999999,49.8387777318655,-14.8893839483491));
#56816=CARTESIAN_POINT('Origin',(-85.9899999999999,55.0349236943356,-17.889395137807));
#56817=CARTESIAN_POINT('Origin',(-85.9899999999997,60.2949931567668,-27.));
#56818=CARTESIAN_POINT('Origin',(-85.9899999999995,42.6698984466481,-20.6937528963263));
#56819=CARTESIAN_POINT('Origin',(-85.9899999999997,46.4876237572749,-39.3062471036737));
#56820=CARTESIAN_POINT('Origin',(-85.9899999999996,42.6698984466481,-39.3062471036737));
#56821=CARTESIAN_POINT('Origin',(-85.9899999999993,37.4737575460498,-36.3062271467965));
#56822=CARTESIAN_POINT('Origin',(-85.9899999999993,35.5649111404189,-33.));
#56823=CARTESIAN_POINT('Origin',(-85.9899999999993,35.5649111404189,-27.));
#56824=CARTESIAN_POINT('Origin',(-85.9899999999995,37.4737575460499,-23.6937728532035));
#56825=CARTESIAN_POINT('Origin',(-85.989999999999,46.487623757275,-20.6937528963263));
#56826=CARTESIAN_POINT('Origin',(-85.9899999999992,53.5926110635042,-27.));
#56827=CARTESIAN_POINT('Origin',(-74.39,76.,45.));
#56828=CARTESIAN_POINT('',(-74.39,76.,47.667));
#56829=CARTESIAN_POINT('',(-74.39,78.667,45.));
#56830=CARTESIAN_POINT('Origin',(-74.39,70.792807570849,47.667));
#56831=CARTESIAN_POINT('',(-74.39,70.792807570849,47.667));
#56832=CARTESIAN_POINT('Origin',(-74.39,70.792807570849,45.));
#56833=CARTESIAN_POINT('',(-74.39,68.9069537854245,46.8858537854245));
#56834=CARTESIAN_POINT('Origin',(-74.39,66.0242462145755,44.0031462145755));
#56835=CARTESIAN_POINT('',(-74.39,66.0242462145755,44.0031462145755));
#56836=CARTESIAN_POINT('Origin',(-74.39,67.9101,42.117292429151));
#56837=CARTESIAN_POINT('',(-74.39,65.2431,42.117292429151));
#56838=CARTESIAN_POINT('Origin',(-74.39,65.2431,34.547707570849));
#56839=CARTESIAN_POINT('',(-74.39,65.2431,34.547707570849));
#56840=CARTESIAN_POINT('Origin',(-74.39,67.9101,34.547707570849));
#56841=CARTESIAN_POINT('',(-74.39,66.0242462145755,32.6618537854245));
#56842=CARTESIAN_POINT('Origin',(-74.39,68.9069537854245,29.7791462145755));
#56843=CARTESIAN_POINT('',(-74.39,68.9069537854245,29.7791462145755));
#56844=CARTESIAN_POINT('Origin',(-74.39,70.792807570849,31.665));
#56845=CARTESIAN_POINT('',(-74.39,70.792807570849,28.998));
#56846=CARTESIAN_POINT('Origin',(-74.39,76.,28.998));
#56847=CARTESIAN_POINT('',(-74.39,76.,28.998));
#56848=CARTESIAN_POINT('Origin',(-74.39,76.,31.665));
#56849=CARTESIAN_POINT('',(-74.39,78.667,31.665));
#56850=CARTESIAN_POINT('Origin',(-74.39,78.667,45.));
#56851=CARTESIAN_POINT('Origin',(-74.39,64.417,65.));
#56852=CARTESIAN_POINT('',(-74.39,64.417,65.));
#56853=CARTESIAN_POINT('',(-74.39,64.417,75.));
#56854=CARTESIAN_POINT('Origin',(-74.39,64.6169999999999,65.));
#56855=CARTESIAN_POINT('',(-74.39,78.6669999999999,65.));
#56856=CARTESIAN_POINT('Origin',(-74.39,78.667,75.));
#56857=CARTESIAN_POINT('',(-74.39,78.667,75.));
#56858=CARTESIAN_POINT('Origin',(-74.39,78.467,75.));
#56859=CARTESIAN_POINT('Origin',(-84.39,91.,75.));
#56860=CARTESIAN_POINT('Origin',(69.81,91.,75.));
#56861=CARTESIAN_POINT('Origin',(69.01,86.,-80.));
#56862=CARTESIAN_POINT('Origin',(-82.79,86.,-80.));
#56863=CARTESIAN_POINT('Origin',(60.61,1.21259619067905E-14,-69.5));
#56864=CARTESIAN_POINT('',(60.61,46.0787611019615,-69.5));
#56865=CARTESIAN_POINT('Origin',(60.61,46.0787611019615,-68.));
#56866=CARTESIAN_POINT('',(60.61,46.0787611019615,-66.5));
#56867=CARTESIAN_POINT('Origin',(60.61,1.21259619067905E-14,-66.5));
#56868=CARTESIAN_POINT('Origin',(60.61,1.21259619067905E-14,-16.5));
#56869=CARTESIAN_POINT('',(60.61,18.0787611019615,-16.5));
#56870=CARTESIAN_POINT('Origin',(60.61,1.21259619067905E-14,-19.5));
#56871=CARTESIAN_POINT('',(60.61,18.0787611019615,-19.5));
#56872=CARTESIAN_POINT('Origin',(60.61,18.0787611019615,-18.));
#56873=CARTESIAN_POINT('Origin',(60.61,1.21259619067905E-14,-21.5));
#56874=CARTESIAN_POINT('',(60.61,18.0787611019615,-21.5));
#56875=CARTESIAN_POINT('Origin',(60.61,1.21259619067905E-14,-24.5));
#56876=CARTESIAN_POINT('',(60.61,18.0787611019615,-24.5));
#56877=CARTESIAN_POINT('Origin',(60.61,18.0787611019615,-23.));
#56878=CARTESIAN_POINT('Origin',(60.61,1.21259619067905E-14,-24.5));
#56879=CARTESIAN_POINT('',(60.61,46.0787611019615,-24.5));
#56880=CARTESIAN_POINT('Origin',(60.61,46.0787611019615,-23.));
#56881=CARTESIAN_POINT('',(60.61,46.0787611019615,-21.5));
#56882=CARTESIAN_POINT('Origin',(60.61,1.21259619067905E-14,-21.5));
#56883=CARTESIAN_POINT('Origin',(60.61,1.21259619067905E-14,-26.5));
#56884=CARTESIAN_POINT('',(60.61,18.0787611019615,-26.5));
#56885=CARTESIAN_POINT('Origin',(60.61,1.21259619067905E-14,-29.5));
#56886=CARTESIAN_POINT('',(60.61,18.0787611019615,-29.5));
#56887=CARTESIAN_POINT('Origin',(60.61,18.0787611019615,-28.));
#56888=CARTESIAN_POINT('Origin',(60.61,1.21259619067905E-14,-19.5));
#56889=CARTESIAN_POINT('',(60.61,46.0787611019615,-19.5));
#56890=CARTESIAN_POINT('Origin',(60.61,46.0787611019615,-18.));
#56891=CARTESIAN_POINT('',(60.61,46.0787611019615,-16.5));
#56892=CARTESIAN_POINT('Origin',(60.61,1.21259619067905E-14,-16.5));
#56893=CARTESIAN_POINT('Origin',(60.61,1.21259619067905E-14,-14.5));
#56894=CARTESIAN_POINT('',(60.61,46.0787611019615,-14.5));
#56895=CARTESIAN_POINT('Origin',(60.61,46.0787611019615,-13.));
#56896=CARTESIAN_POINT('',(60.61,46.0787611019615,-11.5));
#56897=CARTESIAN_POINT('Origin',(60.61,1.21259619067905E-14,-11.5));
#56898=CARTESIAN_POINT('Origin',(60.61,1.21259619067905E-14,-11.5));
#56899=CARTESIAN_POINT('',(60.61,18.0787611019615,-11.5));
#56900=CARTESIAN_POINT('Origin',(60.61,1.21259619067905E-14,-14.5));
#56901=CARTESIAN_POINT('',(60.61,18.0787611019615,-14.5));
#56902=CARTESIAN_POINT('Origin',(60.61,18.0787611019615,-13.));
#56903=CARTESIAN_POINT('Origin',(60.61,1.21259619067905E-14,-51.5));
#56904=CARTESIAN_POINT('',(60.61,18.0787611019615,-51.5));
#56905=CARTESIAN_POINT('Origin',(60.61,1.21259619067905E-14,-54.5));
#56906=CARTESIAN_POINT('',(60.61,18.0787611019615,-54.5));
#56907=CARTESIAN_POINT('Origin',(60.61,18.0787611019615,-53.));
#56908=CARTESIAN_POINT('Origin',(60.61,1.21259619067905E-14,-46.5));
#56909=CARTESIAN_POINT('',(60.61,18.0787611019615,-46.5));
#56910=CARTESIAN_POINT('Origin',(60.61,1.21259619067905E-14,-49.5));
#56911=CARTESIAN_POINT('',(60.61,18.0787611019615,-49.5));
#56912=CARTESIAN_POINT('Origin',(60.61,18.0787611019615,-48.));
#56913=CARTESIAN_POINT('Origin',(60.61,1.21259619067905E-14,-41.5));
#56914=CARTESIAN_POINT('',(60.61,18.0787611019615,-41.5));
#56915=CARTESIAN_POINT('Origin',(60.61,1.21259619067905E-14,-44.5));
#56916=CARTESIAN_POINT('',(60.61,18.0787611019615,-44.5));
#56917=CARTESIAN_POINT('Origin',(60.61,18.0787611019615,-43.));
#56918=CARTESIAN_POINT('Origin',(60.61,1.21259619067905E-14,-44.5));
#56919=CARTESIAN_POINT('',(60.61,46.0787611019615,-44.5));
#56920=CARTESIAN_POINT('Origin',(60.61,46.0787611019615,-43.));
#56921=CARTESIAN_POINT('',(60.61,46.0787611019615,-41.5));
#56922=CARTESIAN_POINT('Origin',(60.61,1.21259619067905E-14,-41.5));
#56923=CARTESIAN_POINT('Origin',(60.61,1.21259619067905E-14,-49.5));
#56924=CARTESIAN_POINT('',(60.61,46.0787611019615,-49.5));
#56925=CARTESIAN_POINT('Origin',(60.61,46.0787611019615,-48.));
#56926=CARTESIAN_POINT('',(60.61,46.0787611019615,-46.5));
#56927=CARTESIAN_POINT('Origin',(60.61,1.21259619067905E-14,-46.5));
#56928=CARTESIAN_POINT('Origin',(60.61,1.21259619067905E-14,-54.5));
#56929=CARTESIAN_POINT('',(60.61,46.0787611019615,-54.5));
#56930=CARTESIAN_POINT('Origin',(60.61,46.0787611019615,-53.));
#56931=CARTESIAN_POINT('',(60.61,46.0787611019615,-51.5));
#56932=CARTESIAN_POINT('Origin',(60.61,1.21259619067905E-14,-51.5));
#56933=CARTESIAN_POINT('Origin',(60.61,1.21259619067905E-14,-59.5));
#56934=CARTESIAN_POINT('',(60.61,46.0787611019615,-59.5));
#56935=CARTESIAN_POINT('Origin',(60.61,46.0787611019615,-58.));
#56936=CARTESIAN_POINT('',(60.61,46.0787611019615,-56.5));
#56937=CARTESIAN_POINT('Origin',(60.61,1.21259619067905E-14,-56.5));
#56938=CARTESIAN_POINT('Origin',(60.61,1.21259619067905E-14,-64.5));
#56939=CARTESIAN_POINT('',(60.61,46.0787611019615,-64.5));
#56940=CARTESIAN_POINT('Origin',(60.61,46.0787611019615,-63.));
#56941=CARTESIAN_POINT('',(60.61,46.0787611019615,-61.5));
#56942=CARTESIAN_POINT('Origin',(60.61,1.21259619067905E-14,-61.5));
#56943=CARTESIAN_POINT('Origin',(60.61,1.21259619067905E-14,-29.5));
#56944=CARTESIAN_POINT('',(60.61,46.0787611019615,-29.5));
#56945=CARTESIAN_POINT('Origin',(60.61,46.0787611019615,-28.));
#56946=CARTESIAN_POINT('',(60.61,46.0787611019615,-26.5));
#56947=CARTESIAN_POINT('Origin',(60.61,1.21259619067905E-14,-26.5));
#56948=CARTESIAN_POINT('Origin',(60.61,1.21259619067905E-14,-34.5));
#56949=CARTESIAN_POINT('',(60.61,46.0787611019615,-34.5));
#56950=CARTESIAN_POINT('Origin',(60.61,46.0787611019615,-33.));
#56951=CARTESIAN_POINT('',(60.61,46.0787611019615,-31.5));
#56952=CARTESIAN_POINT('Origin',(60.61,1.21259619067905E-14,-31.5));
#56953=CARTESIAN_POINT('Origin',(60.61,1.21259619067905E-14,-31.5));
#56954=CARTESIAN_POINT('',(60.61,18.0787611019615,-31.5));
#56955=CARTESIAN_POINT('Origin',(60.61,1.21259619067905E-14,-34.5));
#56956=CARTESIAN_POINT('',(60.61,18.0787611019615,-34.5));
#56957=CARTESIAN_POINT('Origin',(60.61,18.0787611019615,-33.));
#56958=CARTESIAN_POINT('Origin',(60.61,1.21259619067905E-14,-36.5));
#56959=CARTESIAN_POINT('',(60.61,18.0787611019615,-36.5));
#56960=CARTESIAN_POINT('Origin',(60.61,1.21259619067905E-14,-39.5));
#56961=CARTESIAN_POINT('',(60.61,18.0787611019615,-39.5));
#56962=CARTESIAN_POINT('Origin',(60.61,18.0787611019615,-38.));
#56963=CARTESIAN_POINT('Origin',(60.61,1.21259619067905E-14,-56.5));
#56964=CARTESIAN_POINT('',(60.61,18.0787611019615,-56.5));
#56965=CARTESIAN_POINT('Origin',(60.61,1.21259619067905E-14,-59.5));
#56966=CARTESIAN_POINT('',(60.61,18.0787611019615,-59.5));
#56967=CARTESIAN_POINT('Origin',(60.61,18.0787611019615,-58.));
#56968=CARTESIAN_POINT('Origin',(60.61,1.21259619067905E-14,-61.5));
#56969=CARTESIAN_POINT('',(60.61,18.0787611019615,-61.5));
#56970=CARTESIAN_POINT('Origin',(60.61,1.21259619067905E-14,-64.5));
#56971=CARTESIAN_POINT('',(60.61,18.0787611019615,-64.5));
#56972=CARTESIAN_POINT('Origin',(60.61,18.0787611019615,-63.));
#56973=CARTESIAN_POINT('Origin',(60.61,1.21259619067905E-14,-66.5));
#56974=CARTESIAN_POINT('',(60.61,18.0787611019615,-66.5));
#56975=CARTESIAN_POINT('Origin',(60.61,1.21259619067905E-14,-69.5));
#56976=CARTESIAN_POINT('',(60.61,18.0787611019615,-69.5));
#56977=CARTESIAN_POINT('Origin',(60.61,18.0787611019615,-68.));
#56978=CARTESIAN_POINT('Origin',(60.61,1.21259619067905E-14,-39.5));
#56979=CARTESIAN_POINT('',(60.61,46.0787611019615,-39.5));
#56980=CARTESIAN_POINT('Origin',(60.61,46.0787611019615,-38.));
#56981=CARTESIAN_POINT('',(60.61,46.0787611019615,-36.5));
#56982=CARTESIAN_POINT('Origin',(60.61,1.21259619067905E-14,-36.5));
#56983=CARTESIAN_POINT('Origin',(60.61,1.21259619067905E-14,66.5));
#56984=CARTESIAN_POINT('',(60.61,46.0787611019615,66.5));
#56985=CARTESIAN_POINT('Origin',(60.61,46.0787611019615,68.));
#56986=CARTESIAN_POINT('',(60.61,46.0787611019615,69.5));
#56987=CARTESIAN_POINT('Origin',(60.61,1.21259619067905E-14,69.5));
#56988=CARTESIAN_POINT('Origin',(60.61,1.21259619067905E-14,16.5));
#56989=CARTESIAN_POINT('',(60.61,18.0787611019615,16.5));
#56990=CARTESIAN_POINT('Origin',(60.61,18.0787611019615,18.));
#56991=CARTESIAN_POINT('',(60.61,18.0787611019615,19.5));
#56992=CARTESIAN_POINT('Origin',(60.61,1.21259619067905E-14,19.5));
#56993=CARTESIAN_POINT('Origin',(60.61,1.21259619067905E-14,21.5));
#56994=CARTESIAN_POINT('',(60.61,18.0787611019615,21.5));
#56995=CARTESIAN_POINT('Origin',(60.61,18.0787611019615,23.));
#56996=CARTESIAN_POINT('',(60.61,18.0787611019615,24.5));
#56997=CARTESIAN_POINT('Origin',(60.61,1.21259619067905E-14,24.5));
#56998=CARTESIAN_POINT('Origin',(60.61,1.21259619067905E-14,21.5));
#56999=CARTESIAN_POINT('',(60.61,46.0787611019615,21.5));
#57000=CARTESIAN_POINT('Origin',(60.61,46.0787611019615,23.));
#57001=CARTESIAN_POINT('',(60.61,46.0787611019615,24.5));
#57002=CARTESIAN_POINT('Origin',(60.61,1.21259619067905E-14,24.5));
#57003=CARTESIAN_POINT('Origin',(60.61,1.21259619067905E-14,26.5));
#57004=CARTESIAN_POINT('',(60.61,18.0787611019615,26.5));
#57005=CARTESIAN_POINT('Origin',(60.61,18.0787611019615,28.));
#57006=CARTESIAN_POINT('',(60.61,18.0787611019615,29.5));
#57007=CARTESIAN_POINT('Origin',(60.61,1.21259619067905E-14,29.5));
#57008=CARTESIAN_POINT('Origin',(60.61,1.21259619067905E-14,16.5));
#57009=CARTESIAN_POINT('',(60.61,46.0787611019615,16.5));
#57010=CARTESIAN_POINT('Origin',(60.61,46.0787611019615,18.));
#57011=CARTESIAN_POINT('',(60.61,46.0787611019615,19.5));
#57012=CARTESIAN_POINT('Origin',(60.61,1.21259619067905E-14,19.5));
#57013=CARTESIAN_POINT('Origin',(60.61,1.21259619067905E-14,11.5));
#57014=CARTESIAN_POINT('',(60.61,46.0787611019615,11.5));
#57015=CARTESIAN_POINT('Origin',(60.61,46.0787611019615,13.));
#57016=CARTESIAN_POINT('',(60.61,46.0787611019615,14.5));
#57017=CARTESIAN_POINT('Origin',(60.61,1.21259619067905E-14,14.5));
#57018=CARTESIAN_POINT('Origin',(60.61,1.21259619067905E-14,11.5));
#57019=CARTESIAN_POINT('',(60.61,18.0787611019615,11.5));
#57020=CARTESIAN_POINT('Origin',(60.61,18.0787611019615,13.));
#57021=CARTESIAN_POINT('',(60.61,18.0787611019615,14.5));
#57022=CARTESIAN_POINT('Origin',(60.61,1.21259619067905E-14,14.5));
#57023=CARTESIAN_POINT('Origin',(60.61,1.21259619067905E-14,51.5));
#57024=CARTESIAN_POINT('',(60.61,18.0787611019615,51.5));
#57025=CARTESIAN_POINT('Origin',(60.61,18.0787611019615,53.));
#57026=CARTESIAN_POINT('',(60.61,18.0787611019615,54.5));
#57027=CARTESIAN_POINT('Origin',(60.61,1.21259619067905E-14,54.5));
#57028=CARTESIAN_POINT('Origin',(60.61,1.21259619067905E-14,46.5));
#57029=CARTESIAN_POINT('',(60.61,18.0787611019615,46.5));
#57030=CARTESIAN_POINT('Origin',(60.61,18.0787611019615,48.));
#57031=CARTESIAN_POINT('',(60.61,18.0787611019615,49.5));
#57032=CARTESIAN_POINT('Origin',(60.61,1.21259619067905E-14,49.5));
#57033=CARTESIAN_POINT('Origin',(60.61,1.21259619067905E-14,41.5));
#57034=CARTESIAN_POINT('',(60.61,18.0787611019615,41.5));
#57035=CARTESIAN_POINT('Origin',(60.61,18.0787611019615,43.));
#57036=CARTESIAN_POINT('',(60.61,18.0787611019615,44.5));
#57037=CARTESIAN_POINT('Origin',(60.61,1.21259619067905E-14,44.5));
#57038=CARTESIAN_POINT('Origin',(60.61,1.21259619067905E-14,41.5));
#57039=CARTESIAN_POINT('',(60.61,46.0787611019615,41.5));
#57040=CARTESIAN_POINT('Origin',(60.61,46.0787611019615,43.));
#57041=CARTESIAN_POINT('',(60.61,46.0787611019615,44.5));
#57042=CARTESIAN_POINT('Origin',(60.61,1.21259619067905E-14,44.5));
#57043=CARTESIAN_POINT('Origin',(60.61,1.21259619067905E-14,46.5));
#57044=CARTESIAN_POINT('',(60.61,46.0787611019615,46.5));
#57045=CARTESIAN_POINT('Origin',(60.61,46.0787611019615,48.));
#57046=CARTESIAN_POINT('',(60.61,46.0787611019615,49.5));
#57047=CARTESIAN_POINT('Origin',(60.61,1.21259619067905E-14,49.5));
#57048=CARTESIAN_POINT('Origin',(60.61,1.21259619067905E-14,51.5));
#57049=CARTESIAN_POINT('',(60.61,46.0787611019615,51.5));
#57050=CARTESIAN_POINT('Origin',(60.61,46.0787611019615,53.));
#57051=CARTESIAN_POINT('',(60.61,46.0787611019615,54.5));
#57052=CARTESIAN_POINT('Origin',(60.61,1.21259619067905E-14,54.5));
#57053=CARTESIAN_POINT('Origin',(60.61,1.21259619067905E-14,56.5));
#57054=CARTESIAN_POINT('',(60.61,46.0787611019615,56.5));
#57055=CARTESIAN_POINT('Origin',(60.61,46.0787611019615,58.));
#57056=CARTESIAN_POINT('',(60.61,46.0787611019615,59.5));
#57057=CARTESIAN_POINT('Origin',(60.61,1.21259619067905E-14,59.5));
#57058=CARTESIAN_POINT('Origin',(60.61,1.21259619067905E-14,61.5));
#57059=CARTESIAN_POINT('',(60.61,46.0787611019615,61.5));
#57060=CARTESIAN_POINT('Origin',(60.61,46.0787611019615,63.));
#57061=CARTESIAN_POINT('',(60.61,46.0787611019615,64.5));
#57062=CARTESIAN_POINT('Origin',(60.61,1.21259619067905E-14,64.5));
#57063=CARTESIAN_POINT('Origin',(60.61,1.21259619067905E-14,26.5));
#57064=CARTESIAN_POINT('',(60.61,46.0787611019615,26.5));
#57065=CARTESIAN_POINT('Origin',(60.61,46.0787611019615,28.));
#57066=CARTESIAN_POINT('',(60.61,46.0787611019615,29.5));
#57067=CARTESIAN_POINT('Origin',(60.61,1.21259619067905E-14,29.5));
#57068=CARTESIAN_POINT('Origin',(60.61,1.21259619067905E-14,31.5));
#57069=CARTESIAN_POINT('',(60.61,46.0787611019615,31.5));
#57070=CARTESIAN_POINT('Origin',(60.61,46.0787611019615,33.));
#57071=CARTESIAN_POINT('',(60.61,46.0787611019615,34.5));
#57072=CARTESIAN_POINT('Origin',(60.61,1.21259619067905E-14,34.5));
#57073=CARTESIAN_POINT('Origin',(60.61,1.21259619067905E-14,31.5));
#57074=CARTESIAN_POINT('',(60.61,18.0787611019615,31.5));
#57075=CARTESIAN_POINT('Origin',(60.61,18.0787611019615,33.));
#57076=CARTESIAN_POINT('',(60.61,18.0787611019615,34.5));
#57077=CARTESIAN_POINT('Origin',(60.61,1.21259619067905E-14,34.5));
#57078=CARTESIAN_POINT('Origin',(60.61,1.21259619067905E-14,36.5));
#57079=CARTESIAN_POINT('',(60.61,18.0787611019615,36.5));
#57080=CARTESIAN_POINT('Origin',(60.61,18.0787611019615,38.));
#57081=CARTESIAN_POINT('',(60.61,18.0787611019615,39.5));
#57082=CARTESIAN_POINT('Origin',(60.61,1.21259619067905E-14,39.5));
#57083=CARTESIAN_POINT('Origin',(60.61,1.21259619067905E-14,56.5));
#57084=CARTESIAN_POINT('',(60.61,18.0787611019615,56.5));
#57085=CARTESIAN_POINT('Origin',(60.61,18.0787611019615,58.));
#57086=CARTESIAN_POINT('',(60.61,18.0787611019615,59.5));
#57087=CARTESIAN_POINT('Origin',(60.61,1.21259619067905E-14,59.5));
#57088=CARTESIAN_POINT('Origin',(60.61,1.21259619067905E-14,61.5));
#57089=CARTESIAN_POINT('',(60.61,18.0787611019615,61.5));
#57090=CARTESIAN_POINT('Origin',(60.61,18.0787611019615,63.));
#57091=CARTESIAN_POINT('',(60.61,18.0787611019615,64.5));
#57092=CARTESIAN_POINT('Origin',(60.61,1.21259619067905E-14,64.5));
#57093=CARTESIAN_POINT('Origin',(60.61,1.21259619067905E-14,66.5));
#57094=CARTESIAN_POINT('',(60.61,18.0787611019615,66.5));
#57095=CARTESIAN_POINT('Origin',(60.61,18.0787611019615,68.));
#57096=CARTESIAN_POINT('',(60.61,18.0787611019615,69.5));
#57097=CARTESIAN_POINT('Origin',(60.61,1.21259619067905E-14,69.5));
#57098=CARTESIAN_POINT('Origin',(60.61,1.21259619067905E-14,36.5));
#57099=CARTESIAN_POINT('',(60.61,46.0787611019615,36.5));
#57100=CARTESIAN_POINT('Origin',(60.61,46.0787611019615,38.));
#57101=CARTESIAN_POINT('',(60.61,46.0787611019615,39.5));
#57102=CARTESIAN_POINT('Origin',(60.61,1.21259619067905E-14,39.5));
#57103=CARTESIAN_POINT('Origin',(53.1295753616236,-3.2,80.));
#57104=CARTESIAN_POINT('',(53.1295753616236,-3.19999999999999,78.16));
#57105=CARTESIAN_POINT('Origin',(53.1295753616236,-3.19999999999999,78.16));
#57106=CARTESIAN_POINT('',(52.8895753616236,-3.19999999999999,78.16));
#57107=CARTESIAN_POINT('Origin',(52.8895753616236,-3.19999999999999,78.16));
#57108=CARTESIAN_POINT('',(52.8895753616236,-3.19999999999999,78.4));
#57109=CARTESIAN_POINT('Origin',(-67.1104246383764,-3.19999999999999,78.4));
#57110=CARTESIAN_POINT('',(-67.1104246383764,-3.19999999999999,78.4));
#57111=CARTESIAN_POINT('',(-67.1104246383764,-3.19999999999999,78.16));
#57112=CARTESIAN_POINT('Origin',(-67.1104246383764,-3.19999999999999,78.16));
#57113=CARTESIAN_POINT('',(-67.3504246383764,-3.19999999999999,78.16));
#57114=CARTESIAN_POINT('Origin',(-67.3504246383764,-3.19999999999999,78.16));
#57115=CARTESIAN_POINT('Origin',(-67.1104246383764,-2.4,78.4));
#57116=CARTESIAN_POINT('',(-67.1104246383764,-2.4,80.));
#57117=CARTESIAN_POINT('Origin',(-67.1104246383764,-2.4,78.4));
#57118=CARTESIAN_POINT('Origin',(-67.1104246383764,-2.4,78.4));
#57119=CARTESIAN_POINT('Origin',(52.8895753616236,-2.4,78.4));
#57120=CARTESIAN_POINT('Origin',(52.8895753616236,-2.4,78.4));
#57121=CARTESIAN_POINT('',(52.8895753616236,-2.4,79.2));
#57122=CARTESIAN_POINT('Origin',(52.8895753616236,-2.4,78.4));
#57123=CARTESIAN_POINT('Origin',(52.8895753616236,-2.4,78.4));
#57124=CARTESIAN_POINT('Origin',(52.8895753616236,-2.4,78.4));
#57125=CARTESIAN_POINT('Origin',(52.8895753616236,2.80000000000001,80.));
#57126=CARTESIAN_POINT('',(52.8895753616236,2.80000000000001,80.));
#57127=CARTESIAN_POINT('Origin',(-67.1104246383764,-3.2,80.));
#57128=CARTESIAN_POINT('',(-67.1104246383764,2.79999999999996,80.));
#57129=CARTESIAN_POINT('Origin',(48.8895753616236,2.80000000000003,80.));
#57130=CARTESIAN_POINT('',(48.8895753616235,6.80000000000003,80.));
#57131=CARTESIAN_POINT('Origin',(-63.1104246383764,6.79999999999999,80.));
#57132=CARTESIAN_POINT('',(-63.1104246383764,6.79999999999999,80.));
#57133=CARTESIAN_POINT('Origin',(-63.1104246383764,2.79999999999999,80.));
#57134=CARTESIAN_POINT('Origin',(-52.1104246383764,3.80000000000003,79.9999999999841));
#57135=CARTESIAN_POINT('Origin',(-46.8391000074924,3.80000000000003,77.9999999999841));
#57136=CARTESIAN_POINT('Origin',(-57.3817492692605,3.80000000000003,77.9999999999841));
#57137=CARTESIAN_POINT('Origin',(-52.1104246383764,-0.199999999999972,79.9999999999841));
#57138=CARTESIAN_POINT('Origin',(-57.3817492692605,-0.199999999999971,77.9999999999841));
#57139=CARTESIAN_POINT('Origin',(-46.8391000074924,-0.199999999999971,77.9999999999841));
#57140=CARTESIAN_POINT('Origin',(-46.8391000074924,3.80000000000003,77.9999999999841));
#57141=CARTESIAN_POINT('',(-48.6500178794101,3.80000000000003,78.8488677524455));
#57142=CARTESIAN_POINT('Origin',(-46.8391000074924,3.80000000000003,77.9999999999841));
#57143=CARTESIAN_POINT('',(-48.6500178794101,-0.199999999999972,78.8488677524455));
#57144=CARTESIAN_POINT('',(-48.6500178794101,3.80000000000003,78.8488677524455));
#57145=CARTESIAN_POINT('Origin',(-46.8391000074924,-0.199999999999971,77.9999999999841));
#57146=CARTESIAN_POINT('Origin',(-57.3817492692605,1.80000000000003,77.9999999999841));
#57147=CARTESIAN_POINT('',(-55.5708313973427,-0.199999999999972,78.8488677524455));
#57148=CARTESIAN_POINT('Origin',(-57.3817492692605,-0.199999999999971,77.9999999999841));
#57149=CARTESIAN_POINT('',(-55.5708313973427,3.80000000000003,78.8488677524455));
#57150=CARTESIAN_POINT('',(-55.5708313973427,3.80000000000003,78.8488677524455));
#57151=CARTESIAN_POINT('Origin',(-57.3817492692605,3.80000000000003,77.9999999999841));
#57152=CARTESIAN_POINT('Origin',(-57.3817492692605,-0.199999999999971,77.9999999999841));
#57153=CARTESIAN_POINT('',(-56.2951985461098,-0.199999999999974,78.509320651461));
#57154=CARTESIAN_POINT('Origin',(-57.3817492692605,-0.19999999999997,77.9999999999841));
#57155=CARTESIAN_POINT('',(-55.7394867179188,-0.199999999999974,77.3238020846534));
#57156=CARTESIAN_POINT('',(-55.3347917871435,-0.199999999999974,76.4604528989995));
#57157=CARTESIAN_POINT('',(-53.6569311652134,-0.199999999999972,75.9999999999841));
#57158=CARTESIAN_POINT('Origin',(-53.6569311652134,-0.19999999999997,78.2999999999841));
#57159=CARTESIAN_POINT('',(-50.5639181115395,-0.19999999999997,75.9999999999841));
#57160=CARTESIAN_POINT('',(-49.6104246383764,-0.199999999999972,75.9999999999841));
#57161=CARTESIAN_POINT('',(-48.4813625588341,-0.199999999999974,77.3238020846534));
#57162=CARTESIAN_POINT('Origin',(-50.5639181115395,-0.19999999999997,78.2999999999841));
#57163=CARTESIAN_POINT('',(-47.925650730643,-0.19999999999997,78.509320651461));
#57164=CARTESIAN_POINT('',(-48.8860574896093,-0.199999999999974,76.4604528989995));
#57165=CARTESIAN_POINT('Origin',(-46.8391000074924,-0.19999999999997,77.9999999999841));
#57166=CARTESIAN_POINT('',(-49.2057297076012,-0.199999999999972,77.663349185638));
#57167=CARTESIAN_POINT('',(-49.6104246383764,-0.199999999999972,76.7999999999841));
#57168=CARTESIAN_POINT('',(-50.5639181115395,-0.199999999999972,76.7999999999841));
#57169=CARTESIAN_POINT('Origin',(-50.5639181115395,-0.199999999999971,78.2999999999841));
#57170=CARTESIAN_POINT('',(-53.6569311652134,-0.199999999999972,76.7999999999841));
#57171=CARTESIAN_POINT('',(-49.6104246383764,-0.199999999999972,76.7999999999841));
#57172=CARTESIAN_POINT('',(-55.0151195691517,-0.199999999999972,77.663349185638));
#57173=CARTESIAN_POINT('Origin',(-53.6569311652134,-0.199999999999971,78.2999999999841));
#57174=CARTESIAN_POINT('',(-54.6104246383764,-0.199999999999972,76.7999999999841));
#57175=CARTESIAN_POINT('Origin',(-49.6104246383764,3.80000000000003,76.7999999999841));
#57176=CARTESIAN_POINT('',(-47.925650730643,3.80000000000003,78.509320651461));
#57177=CARTESIAN_POINT('Origin',(-46.8391000074924,3.80000000000003,77.9999999999841));
#57178=CARTESIAN_POINT('',(-48.4813625588341,3.80000000000003,77.3238020846534));
#57179=CARTESIAN_POINT('',(-48.8860574896093,3.80000000000003,76.4604528989995));
#57180=CARTESIAN_POINT('',(-50.5639181115395,3.80000000000003,75.9999999999841));
#57181=CARTESIAN_POINT('Origin',(-50.5639181115395,3.80000000000003,78.2999999999841));
#57182=CARTESIAN_POINT('',(-53.6569311652134,3.80000000000003,75.9999999999841));
#57183=CARTESIAN_POINT('',(-49.6104246383764,3.80000000000003,75.9999999999841));
#57184=CARTESIAN_POINT('',(-55.7394867179188,3.80000000000003,77.3238020846534));
#57185=CARTESIAN_POINT('Origin',(-53.6569311652134,3.80000000000003,78.2999999999841));
#57186=CARTESIAN_POINT('',(-56.2951985461098,3.80000000000003,78.509320651461));
#57187=CARTESIAN_POINT('',(-55.3347917871435,3.80000000000003,76.4604528989995));
#57188=CARTESIAN_POINT('Origin',(-57.3817492692605,3.80000000000003,77.9999999999841));
#57189=CARTESIAN_POINT('',(-55.0151195691517,3.80000000000003,77.663349185638));
#57190=CARTESIAN_POINT('',(-54.6104246383764,3.80000000000003,76.7999999999841));
#57191=CARTESIAN_POINT('',(-53.6569311652134,3.80000000000003,76.7999999999841));
#57192=CARTESIAN_POINT('Origin',(-53.6569311652134,3.80000000000003,78.2999999999841));
#57193=CARTESIAN_POINT('',(-50.5639181115395,3.80000000000003,76.7999999999841));
#57194=CARTESIAN_POINT('',(-49.6104246383764,3.80000000000003,76.7999999999841));
#57195=CARTESIAN_POINT('',(-49.2057297076012,3.80000000000003,77.663349185638));
#57196=CARTESIAN_POINT('Origin',(-50.5639181115395,3.80000000000003,78.2999999999841));
#57197=CARTESIAN_POINT('',(-49.6104246383764,3.80000000000003,76.7999999999841));
#57198=CARTESIAN_POINT('Origin',(-50.5639181115395,3.80000000000003,78.2999999999841));
#57199=CARTESIAN_POINT('',(-50.5639181115395,3.80000000000003,76.7999999999841));
#57200=CARTESIAN_POINT('',(-49.2057297076012,3.80000000000003,77.663349185638));
#57201=CARTESIAN_POINT('Origin',(-53.6569311652134,3.80000000000003,78.2999999999841));
#57202=CARTESIAN_POINT('',(-55.0151195691517,3.80000000000003,77.663349185638));
#57203=CARTESIAN_POINT('',(-53.6569311652134,3.80000000000003,76.7999999999841));
#57204=CARTESIAN_POINT('Origin',(-49.6104246383764,3.80000000000003,76.7999999999841));
#57205=CARTESIAN_POINT('Origin',(-54.6104246383764,3.80000000000003,76.7999999999841));
#57206=CARTESIAN_POINT('Origin',(-49.6104246383764,3.80000000000003,76.7999999999841));
#57207=CARTESIAN_POINT('Origin',(-50.5639181115395,3.80000000000003,78.2999999999841));
#57208=CARTESIAN_POINT('',(-48.4813625588341,3.80000000000003,77.3238020846534));
#57209=CARTESIAN_POINT('',(-50.5639181115395,3.80000000000003,75.9999999999841));
#57210=CARTESIAN_POINT('Origin',(-53.6569311652134,3.80000000000003,78.2999999999841));
#57211=CARTESIAN_POINT('',(-53.6569311652134,3.80000000000003,75.9999999999841));
#57212=CARTESIAN_POINT('',(-55.7394867179188,3.80000000000003,77.3238020846534));
#57213=CARTESIAN_POINT('Origin',(-57.3817492692605,1.80000000000003,77.9999999999841));
#57214=CARTESIAN_POINT('',(-56.2951985461098,3.80000000000003,78.509320651461));
#57215=CARTESIAN_POINT('Origin',(-46.8391000074924,3.80000000000003,77.9999999999841));
#57216=CARTESIAN_POINT('',(-47.925650730643,3.80000000000003,78.509320651461));
#57217=CARTESIAN_POINT('Origin',(-48.8860574896093,3.80000000000003,76.4604528989995));
#57218=CARTESIAN_POINT('Origin',(-55.3347917871435,3.80000000000003,76.4604528989995));
#57219=CARTESIAN_POINT('Origin',(-49.6104246383764,3.80000000000003,75.9999999999841));
#57220=CARTESIAN_POINT('Origin',(38.3304246383764,3.80000000000005,79.9999999999841));
#57221=CARTESIAN_POINT('Origin',(43.6017492692605,3.80000000000006,77.9999999999841));
#57222=CARTESIAN_POINT('Origin',(33.0591000074924,3.80000000000005,77.9999999999841));
#57223=CARTESIAN_POINT('Origin',(38.3304246383764,-0.199999999999946,79.9999999999841));
#57224=CARTESIAN_POINT('Origin',(33.0591000074924,-0.199999999999948,77.9999999999841));
#57225=CARTESIAN_POINT('Origin',(43.6017492692605,-0.199999999999942,77.9999999999841));
#57226=CARTESIAN_POINT('Origin',(33.0591000074924,3.80000000000005,77.9999999999841));
#57227=CARTESIAN_POINT('',(34.8700178794101,-0.199999999999948,78.8488677524455));
#57228=CARTESIAN_POINT('Origin',(33.0591000074924,-0.199999999999948,77.9999999999841));
#57229=CARTESIAN_POINT('',(34.8700178794101,3.80000000000005,78.8488677524455));
#57230=CARTESIAN_POINT('',(34.8700178794101,3.80000000000005,78.8488677524455));
#57231=CARTESIAN_POINT('Origin',(33.0591000074924,3.80000000000005,77.9999999999841));
#57232=CARTESIAN_POINT('Origin',(43.6017492692605,1.80000000000006,77.9999999999841));
#57233=CARTESIAN_POINT('',(41.7908313973427,3.80000000000006,78.8488677524455));
#57234=CARTESIAN_POINT('Origin',(43.6017492692605,3.80000000000006,77.9999999999841));
#57235=CARTESIAN_POINT('',(41.7908313973428,-0.199999999999944,78.8488677524455));
#57236=CARTESIAN_POINT('',(41.7908313973427,3.80000000000006,78.8488677524455));
#57237=CARTESIAN_POINT('Origin',(43.6017492692605,-0.199999999999942,77.9999999999841));
#57238=CARTESIAN_POINT('Origin',(33.0591000074924,-0.199999999999948,77.9999999999841));
#57239=CARTESIAN_POINT('',(34.1456507306431,-0.199999999999949,78.509320651461));
#57240=CARTESIAN_POINT('Origin',(33.0591000074924,-0.199999999999947,77.9999999999841));
#57241=CARTESIAN_POINT('',(34.7013625588341,-0.199999999999946,77.3238020846534));
#57242=CARTESIAN_POINT('',(35.1060574896094,-0.19999999999995,76.4604528989995));
#57243=CARTESIAN_POINT('',(36.7839181115395,-0.199999999999947,75.9999999999841));
#57244=CARTESIAN_POINT('Origin',(36.7839181115395,-0.199999999999945,78.2999999999841));
#57245=CARTESIAN_POINT('',(39.8769311652134,-0.199999999999943,75.9999999999841));
#57246=CARTESIAN_POINT('',(35.8304246383764,-0.199999999999948,75.9999999999841));
#57247=CARTESIAN_POINT('',(41.9594867179188,-0.199999999999945,77.3238020846534));
#57248=CARTESIAN_POINT('Origin',(39.8769311652134,-0.199999999999943,78.2999999999841));
#57249=CARTESIAN_POINT('',(42.5151985461099,-0.199999999999945,78.509320651461));
#57250=CARTESIAN_POINT('',(41.5547917871435,-0.199999999999945,76.4604528989995));
#57251=CARTESIAN_POINT('Origin',(43.6017492692605,-0.199999999999941,77.9999999999841));
#57252=CARTESIAN_POINT('',(41.2351195691517,-0.199999999999944,77.663349185638));
#57253=CARTESIAN_POINT('',(40.8304246383765,-0.199999999999944,76.7999999999841));
#57254=CARTESIAN_POINT('',(39.8769311652134,-0.199999999999945,76.7999999999841));
#57255=CARTESIAN_POINT('Origin',(39.8769311652134,-0.199999999999944,78.2999999999841));
#57256=CARTESIAN_POINT('',(36.7839181115395,-0.199999999999947,76.7999999999841));
#57257=CARTESIAN_POINT('',(35.8304246383764,-0.199999999999947,76.7999999999841));
#57258=CARTESIAN_POINT('',(35.4257297076012,-0.199999999999947,77.663349185638));
#57259=CARTESIAN_POINT('Origin',(36.7839181115395,-0.199999999999946,78.2999999999841));
#57260=CARTESIAN_POINT('',(35.8304246383764,-0.199999999999947,76.7999999999841));
#57261=CARTESIAN_POINT('Origin',(35.8304246383764,3.80000000000005,76.7999999999841));
#57262=CARTESIAN_POINT('',(42.5151985461099,3.80000000000006,78.509320651461));
#57263=CARTESIAN_POINT('Origin',(43.6017492692605,3.80000000000006,77.9999999999841));
#57264=CARTESIAN_POINT('',(41.9594867179188,3.80000000000006,77.3238020846534));
#57265=CARTESIAN_POINT('',(41.5547917871435,3.80000000000006,76.4604528989995));
#57266=CARTESIAN_POINT('',(39.8769311652134,3.80000000000005,75.9999999999841));
#57267=CARTESIAN_POINT('Origin',(39.8769311652134,3.80000000000005,78.2999999999841));
#57268=CARTESIAN_POINT('',(36.7839181115395,3.80000000000005,75.9999999999841));
#57269=CARTESIAN_POINT('',(35.8304246383764,3.80000000000005,75.9999999999841));
#57270=CARTESIAN_POINT('',(34.7013625588341,3.80000000000005,77.3238020846534));
#57271=CARTESIAN_POINT('Origin',(36.7839181115395,3.80000000000005,78.2999999999841));
#57272=CARTESIAN_POINT('',(34.1456507306431,3.80000000000005,78.509320651461));
#57273=CARTESIAN_POINT('',(35.1060574896094,3.80000000000005,76.4604528989995));
#57274=CARTESIAN_POINT('Origin',(33.0591000074924,3.80000000000005,77.9999999999841));
#57275=CARTESIAN_POINT('',(35.4257297076012,3.80000000000005,77.663349185638));
#57276=CARTESIAN_POINT('',(35.8304246383764,3.80000000000005,76.7999999999841));
#57277=CARTESIAN_POINT('',(36.7839181115395,3.80000000000005,76.7999999999841));
#57278=CARTESIAN_POINT('Origin',(36.7839181115395,3.80000000000005,78.2999999999841));
#57279=CARTESIAN_POINT('',(39.8769311652134,3.80000000000005,76.7999999999841));
#57280=CARTESIAN_POINT('',(35.8304246383764,3.80000000000005,76.7999999999841));
#57281=CARTESIAN_POINT('',(41.2351195691517,3.80000000000006,77.663349185638));
#57282=CARTESIAN_POINT('Origin',(39.8769311652134,3.80000000000005,78.2999999999841));
#57283=CARTESIAN_POINT('',(40.8304246383765,3.80000000000006,76.7999999999841));
#57284=CARTESIAN_POINT('Origin',(36.7839181115395,3.80000000000005,78.2999999999841));
#57285=CARTESIAN_POINT('',(35.4257297076012,3.80000000000005,77.663349185638));
#57286=CARTESIAN_POINT('',(36.7839181115395,3.80000000000005,76.7999999999841));
#57287=CARTESIAN_POINT('Origin',(39.8769311652134,3.80000000000005,78.2999999999841));
#57288=CARTESIAN_POINT('',(39.8769311652134,3.80000000000005,76.7999999999841));
#57289=CARTESIAN_POINT('',(41.2351195691517,3.80000000000006,77.663349185638));
#57290=CARTESIAN_POINT('Origin',(35.8304246383764,3.80000000000005,76.7999999999841));
#57291=CARTESIAN_POINT('Origin',(40.8304246383765,3.80000000000006,76.7999999999841));
#57292=CARTESIAN_POINT('Origin',(35.8304246383764,3.80000000000005,76.7999999999841));
#57293=CARTESIAN_POINT('Origin',(36.7839181115395,3.80000000000005,78.2999999999841));
#57294=CARTESIAN_POINT('',(36.7839181115395,3.80000000000005,75.9999999999841));
#57295=CARTESIAN_POINT('',(34.7013625588341,3.80000000000005,77.3238020846534));
#57296=CARTESIAN_POINT('Origin',(39.8769311652134,3.80000000000005,78.2999999999841));
#57297=CARTESIAN_POINT('',(41.9594867179188,3.80000000000006,77.3238020846534));
#57298=CARTESIAN_POINT('',(39.8769311652134,3.80000000000005,75.9999999999841));
#57299=CARTESIAN_POINT('Origin',(43.6017492692605,1.80000000000006,77.9999999999841));
#57300=CARTESIAN_POINT('',(42.5151985461099,1.80000000000006,78.509320651461));
#57301=CARTESIAN_POINT('Origin',(33.0591000074924,3.80000000000005,77.9999999999841));
#57302=CARTESIAN_POINT('',(34.1456507306431,3.80000000000005,78.509320651461));
#57303=CARTESIAN_POINT('Origin',(35.1060574896094,3.80000000000005,76.4604528989995));
#57304=CARTESIAN_POINT('Origin',(41.5547917871435,3.80000000000006,76.4604528989995));
#57305=CARTESIAN_POINT('Origin',(35.8304246383764,3.80000000000005,75.9999999999841));
#57306=CARTESIAN_POINT('Origin',(-67.3504246383764,-3.20000000000001,-80.));
#57307=CARTESIAN_POINT('',(-67.3504246383764,-3.20000000000001,-78.16));
#57308=CARTESIAN_POINT('Origin',(-67.3504246383764,-3.20000000000001,-78.16));
#57309=CARTESIAN_POINT('',(-67.1104246383764,-3.20000000000001,-78.16));
#57310=CARTESIAN_POINT('Origin',(-67.1104246383764,-3.20000000000001,-78.16));
#57311=CARTESIAN_POINT('',(-67.1104246383764,-3.20000000000001,-78.4));
#57312=CARTESIAN_POINT('Origin',(52.8895753616236,-3.20000000000001,-78.4));
#57313=CARTESIAN_POINT('',(52.8895753616236,-3.20000000000001,-78.4));
#57314=CARTESIAN_POINT('',(52.8895753616236,-3.20000000000001,-78.16));
#57315=CARTESIAN_POINT('Origin',(52.8895753616236,-3.20000000000001,-78.16));
#57316=CARTESIAN_POINT('',(53.1295753616236,-3.20000000000001,-78.16));
#57317=CARTESIAN_POINT('Origin',(53.1295753616236,-3.20000000000001,-78.16));
#57318=CARTESIAN_POINT('Origin',(52.8895753616236,-2.40000000000002,-78.4));
#57319=CARTESIAN_POINT('',(52.8895753616236,-2.40000000000002,-79.2));
#57320=CARTESIAN_POINT('',(52.8895753616236,-2.40000000000002,-80.));
#57321=CARTESIAN_POINT('',(52.8895753616236,-2.40000000000001,-80.0000000000001));
#57322=CARTESIAN_POINT('Origin',(52.8895753616236,-2.40000000000002,-78.4));
#57323=CARTESIAN_POINT('Origin',(52.8895753616236,-2.40000000000002,-78.4));
#57324=CARTESIAN_POINT('Origin',(-67.1104246383764,-2.40000000000002,-78.4));
#57325=CARTESIAN_POINT('',(-67.1104246383764,-2.40000000000002,-79.2));
#57326=CARTESIAN_POINT('Origin',(-67.1104246383764,-2.40000000000002,-78.4));
#57327=CARTESIAN_POINT('',(-67.1104246383764,-2.40000000000001,-80.));
#57328=CARTESIAN_POINT('',(-67.1104246383764,-2.40000000000001,-79.2));
#57329=CARTESIAN_POINT('Origin',(-67.1104246383764,-2.40000000000002,-78.4));
#57330=CARTESIAN_POINT('Origin',(-67.1104246383764,-2.40000000000002,-78.4));
#57331=CARTESIAN_POINT('',(52.8895753616236,-2.40000000000001,-80.));
#57332=CARTESIAN_POINT('Origin',(-67.1104246383764,-2.40000000000002,-78.4));
#57333=CARTESIAN_POINT('',(52.8895753616236,-2.40000000000001,-79.2));
#57334=CARTESIAN_POINT('Origin',(52.8895753616236,2.80000000000001,-80.));
#57335=CARTESIAN_POINT('',(52.8895753616236,2.80000000000002,-79.2));
#57336=CARTESIAN_POINT('',(52.8895753616236,2.80000000000012,-79.2));
#57337=CARTESIAN_POINT('',(52.8895753616236,2.80000000000002,-80.));
#57338=CARTESIAN_POINT('',(52.8895753616236,2.80000000000001,-80.));
#57339=CARTESIAN_POINT('',(52.8895753616236,2.80000000000001,-80.));
#57340=CARTESIAN_POINT('Origin',(-67.1104246383764,-3.2,-80.));
#57341=CARTESIAN_POINT('',(-67.1104246383764,2.79999999999997,-80.));
#57342=CARTESIAN_POINT('',(-67.1104246383764,-3.2,-80.));
#57343=CARTESIAN_POINT('',(-67.1104246383764,2.79999999999997,-79.2));
#57344=CARTESIAN_POINT('',(-67.1104246383764,2.79999999999999,-79.2));
#57345=CARTESIAN_POINT('',(-67.1104246383764,2.79999999999996,-80.));
#57346=CARTESIAN_POINT('Origin',(-63.1104246383764,2.79999999999999,-80.));
#57347=CARTESIAN_POINT('',(-63.1104246383764,6.79999999999999,-80.));
#57348=CARTESIAN_POINT('Origin',(-63.1104246383764,2.79999999999999,-80.));
#57349=CARTESIAN_POINT('',(48.8895753616235,6.80000000000003,-80.));
#57350=CARTESIAN_POINT('',(-63.1104246383764,6.79999999999999,-80.));
#57351=CARTESIAN_POINT('Origin',(48.8895753616236,2.80000000000003,-80.));
#57352=CARTESIAN_POINT('Origin',(-63.1104246383764,2.79999999999999,-79.2));
#57353=CARTESIAN_POINT('',(48.8895753616235,6.80000000000003,-79.2));
#57354=CARTESIAN_POINT('Origin',(48.8895753616236,2.80000000000003,-79.2));
#57355=CARTESIAN_POINT('',(-63.1104246383764,6.79999999999999,-79.2));
#57356=CARTESIAN_POINT('',(-63.1104246383764,6.79999999999999,-79.2));
#57357=CARTESIAN_POINT('Origin',(-63.1104246383764,2.79999999999999,-79.2));
#57358=CARTESIAN_POINT('Origin',(-63.1104246383764,2.79999999999999,-80.));
#57359=CARTESIAN_POINT('',(-63.1104246383764,6.79999999999999,-80.));
#57360=CARTESIAN_POINT('Origin',(-63.1104246383764,6.79999999999999,-80.));
#57361=CARTESIAN_POINT('',(48.8895753616235,6.80000000000003,-80.));
#57362=CARTESIAN_POINT('Origin',(48.8895753616236,2.80000000000003,-80.));
#57363=CARTESIAN_POINT('',(0.,0.,0.));
#57364=CARTESIAN_POINT('Origin',(-17.78,1.7549973081547,-14.4736733188239));
#57365=CARTESIAN_POINT('',(-5.01908361227606,1.7549973081547,-13.6735733188239));
#57366=CARTESIAN_POINT('Origin',(-5.01908361227606,1.7549973081547,-14.4736733188239));
#57367=CARTESIAN_POINT('',(-4.24429638772394,1.7549973081547,-13.6735733188239));
#57368=CARTESIAN_POINT('',(-17.78,1.7549973081547,-13.6735733188239));
#57369=CARTESIAN_POINT('Origin',(-4.24429638772394,1.7549973081547,-14.4736733188239));
#57370=CARTESIAN_POINT('Origin',(-17.78,1.7549973081547,-14.4736733188239));
#57371=CARTESIAN_POINT('',(4.24429638772393,1.7549973081547,-13.6735733188239));
#57372=CARTESIAN_POINT('Origin',(4.24429638772394,1.7549973081547,-14.4736733188239));
#57373=CARTESIAN_POINT('',(5.01908361227606,1.7549973081547,-13.6735733188239));
#57374=CARTESIAN_POINT('',(-17.78,1.7549973081547,-13.6735733188239));
#57375=CARTESIAN_POINT('Origin',(5.01908361227606,1.7549973081547,-14.4736733188239));
#57376=CARTESIAN_POINT('Origin',(-17.78,-1.6232026918453,-14.4736733188239));
#57377=CARTESIAN_POINT('',(-0.451338313394325,-1.6232026918453,-13.6735733188239));
#57378=CARTESIAN_POINT('Origin',(-0.451338313394324,-1.6232026918453,-14.4736733188239));
#57379=CARTESIAN_POINT('',(0.451338313394325,-1.6232026918453,-13.6735733188239));
#57380=CARTESIAN_POINT('',(-17.78,-1.6232026918453,-13.6735733188239));
#57381=CARTESIAN_POINT('Origin',(0.451338313394325,-1.6232026918453,-14.4736733188239));
#57382=CARTESIAN_POINT('Origin',(-14.224,0.0658973081546998,1.33274668117609));
#57383=CARTESIAN_POINT('',(-13.02385,0.0658973081546999,0.443746681176088));
#57384=CARTESIAN_POINT('',(-15.42415,0.0658973081546997,0.443746681176088));
#57385=CARTESIAN_POINT('Origin',(-14.224,0.0658973081546998,0.443746681176088));
#57386=CARTESIAN_POINT('Origin',(-14.224,0.0658973081546998,0.443746681176088));
#57387=CARTESIAN_POINT('',(-16.1969459099186,0.0658973081546996,1.33274668117609));
#57388=CARTESIAN_POINT('',(-16.1969459099186,0.0658973081546996,1.33274668117609));
#57389=CARTESIAN_POINT('Origin',(-14.224,0.0658973081546998,1.33274668117609));
#57390=CARTESIAN_POINT('Origin',(14.224,0.0658973081546998,1.33274668117609));
#57391=CARTESIAN_POINT('',(15.42415,0.0658973081546999,0.443746681176088));
#57392=CARTESIAN_POINT('',(13.02385,0.0658973081546997,0.443746681176088));
#57393=CARTESIAN_POINT('Origin',(14.224,0.0658973081546998,0.443746681176088));
#57394=CARTESIAN_POINT('Origin',(14.224,0.0658973081546998,0.443746681176088));
#57395=CARTESIAN_POINT('',(12.2510540900814,0.0658973081546996,1.33274668117609));
#57396=CARTESIAN_POINT('',(12.2510540900814,0.0658973081546996,1.33274668117609));
#57397=CARTESIAN_POINT('Origin',(14.224,0.0658973081546998,1.33274668117609));
#57398=CARTESIAN_POINT('Origin',(-14.224,0.0658973081546998,1.33274668117609));
#57399=CARTESIAN_POINT('',(-13.02385,0.0658973081546997,-0.871973318823906));
#57400=CARTESIAN_POINT('',(-13.02385,0.0658973081546997,1.33274668117609));
#57401=CARTESIAN_POINT('Origin',(-14.224,0.0658973081546998,-0.871973318823906));
#57402=CARTESIAN_POINT('Origin',(-14.224,0.0658973081546998,1.33274668117609));
#57403=CARTESIAN_POINT('',(-16.2281306676925,3.00334454458544,1.33274668117609));
#57404=CARTESIAN_POINT('',(-16.2281306676925,-2.87154992827604,1.33274668117609));
#57405=CARTESIAN_POINT('Origin',(-14.224,0.0658973081546998,1.33274668117609));
#57406=CARTESIAN_POINT('',(-16.2281306676925,3.00334454458544,-0.871973318823906));
#57407=CARTESIAN_POINT('',(-16.2281306676925,3.00334454458544,1.33274668117609));
#57408=CARTESIAN_POINT('',(-16.2281306676925,-2.87154992827604,-0.871973318823906));
#57409=CARTESIAN_POINT('Origin',(-14.224,0.0658973081546998,-0.871973318823906));
#57410=CARTESIAN_POINT('',(-16.2281306676925,-2.87154992827604,1.33274668117609));
#57411=CARTESIAN_POINT('Origin',(14.224,0.0658973081546998,1.33274668117609));
#57412=CARTESIAN_POINT('',(15.42415,0.0658973081546997,-0.871973318823906));
#57413=CARTESIAN_POINT('',(15.42415,0.0658973081546997,1.33274668117609));
#57414=CARTESIAN_POINT('Origin',(14.224,0.0658973081546998,-0.871973318823906));
#57415=CARTESIAN_POINT('Origin',(-6.6675,4.1108473081547,-10.0286733188239));
#57416=CARTESIAN_POINT('',(-9.3345,4.11084730815468,-10.0286733188239));
#57417=CARTESIAN_POINT('',(-6.66749999999998,6.7778473081547,-10.0286733188239));
#57418=CARTESIAN_POINT('Origin',(-6.6675,4.1108473081547,-10.0286733188239));
#57419=CARTESIAN_POINT('',(6.66749999999998,6.7778473081547,-10.0286733188239));
#57420=CARTESIAN_POINT('',(-6.66749999999998,6.7778473081547,-10.0286733188239));
#57421=CARTESIAN_POINT('',(9.3345,4.11084730815468,-10.0286733188239));
#57422=CARTESIAN_POINT('Origin',(6.6675,4.1108473081547,-10.0286733188239));
#57423=CARTESIAN_POINT('',(9.3345,-1.09634512099626,-10.0286733188239));
#57424=CARTESIAN_POINT('',(9.3345,-1.09634512099627,-10.0286733188239));
#57425=CARTESIAN_POINT('',(8.55335378542453,-2.98219890642078,-10.0286733188239));
#57426=CARTESIAN_POINT('Origin',(6.6675,-1.09634512099626,-10.0286733188239));
#57427=CARTESIAN_POINT('',(5.67064621457553,-5.86490647726981,-10.0286733188239));
#57428=CARTESIAN_POINT('',(8.55335378542453,-2.98219890642078,-10.0286733188239));
#57429=CARTESIAN_POINT('',(3.784792429151,-6.6460526918453,-10.0286733188239));
#57430=CARTESIAN_POINT('Origin',(3.78479242915099,-3.9790526918453,-10.0286733188239));
#57431=CARTESIAN_POINT('',(-3.78479242915098,-6.6460526918453,-10.0286733188239));
#57432=CARTESIAN_POINT('',(3.784792429151,-6.6460526918453,-10.0286733188239));
#57433=CARTESIAN_POINT('',(-5.67064621457553,-5.8649064772698,-10.0286733188239));
#57434=CARTESIAN_POINT('Origin',(-3.78479242915099,-3.9790526918453,-10.0286733188239));
#57435=CARTESIAN_POINT('',(-8.55335378542452,-2.98219890642078,-10.0286733188239));
#57436=CARTESIAN_POINT('',(-8.55335378542452,-2.98219890642078,-10.0286733188239));
#57437=CARTESIAN_POINT('',(-9.3345,-1.09634512099625,-10.0286733188239));
#57438=CARTESIAN_POINT('Origin',(-6.6675,-1.09634512099626,-10.0286733188239));
#57439=CARTESIAN_POINT('',(-9.3345,4.11084730815468,-10.0286733188239));
#57440=CARTESIAN_POINT('',(1.41351,-3.8012526918453,-10.0286733188239));
#57441=CARTESIAN_POINT('',(1.41351,0.554847308154699,-10.0286733188239));
#57442=CARTESIAN_POINT('',(1.41351,-3.8012526918453,-10.0286733188239));
#57443=CARTESIAN_POINT('',(-1.41351,0.554847308154699,-10.0286733188239));
#57444=CARTESIAN_POINT('',(-1.41351,0.554847308154699,-10.0286733188239));
#57445=CARTESIAN_POINT('',(-1.41351,-3.8012526918453,-10.0286733188239));
#57446=CARTESIAN_POINT('',(-1.41351,0.554847308154699,-10.0286733188239));
#57447=CARTESIAN_POINT('',(1.41351,-3.8012526918453,-10.0286733188239));
#57448=CARTESIAN_POINT('',(-3.21818,-0.4230526918453,-10.0286733188239));
#57449=CARTESIAN_POINT('',(-3.21818,3.9330473081547,-10.0286733188239));
#57450=CARTESIAN_POINT('',(-3.21818,-0.4230526918453,-10.0286733188239));
#57451=CARTESIAN_POINT('',(-6.0452,3.9330473081547,-10.0286733188239));
#57452=CARTESIAN_POINT('',(-6.0452,3.9330473081547,-10.0286733188239));
#57453=CARTESIAN_POINT('',(-6.0452,-0.4230526918453,-10.0286733188239));
#57454=CARTESIAN_POINT('',(-6.0452,3.9330473081547,-10.0286733188239));
#57455=CARTESIAN_POINT('',(-3.21818,-0.4230526918453,-10.0286733188239));
#57456=CARTESIAN_POINT('',(3.21818,-0.4230526918453,-10.0286733188239));
#57457=CARTESIAN_POINT('',(6.0452,-0.4230526918453,-10.0286733188239));
#57458=CARTESIAN_POINT('',(3.21818,-0.4230526918453,-10.0286733188239));
#57459=CARTESIAN_POINT('',(6.0452,3.9330473081547,-10.0286733188239));
#57460=CARTESIAN_POINT('',(6.0452,3.9330473081547,-10.0286733188239));
#57461=CARTESIAN_POINT('',(3.21818,3.9330473081547,-10.0286733188239));
#57462=CARTESIAN_POINT('',(6.0452,3.9330473081547,-10.0286733188239));
#57463=CARTESIAN_POINT('',(3.21818,-0.4230526918453,-10.0286733188239));
#57464=CARTESIAN_POINT('Origin',(-0.70231,-0.156352691845301,0.194826681176092));
#57465=CARTESIAN_POINT('',(-0.70231,-0.156352691845301,2.11901678258961));
#57466=CARTESIAN_POINT('',(-0.70231,-3.0900526918453,2.11901678258961));
#57467=CARTESIAN_POINT('',(-0.70231,-0.1563526918453,2.11901678258961));
#57468=CARTESIAN_POINT('',(-0.70231,-0.156352691845301,-8.4284733188239));
#57469=CARTESIAN_POINT('',(-0.70231,-0.156352691845301,0.194826681176092));
#57470=CARTESIAN_POINT('',(-0.70231,-3.0900526918453,-8.4284733188239));
#57471=CARTESIAN_POINT('',(-0.702309999999999,-3.7123526918453,-8.42847331882391));
#57472=CARTESIAN_POINT('',(-0.70231,-3.0900526918453,0.194826681176092));
#57473=CARTESIAN_POINT('Origin',(0.70231,-3.0900526918453,0.194826681176092));
#57474=CARTESIAN_POINT('',(0.451338313394325,-3.0900526918453,2.84404668117609));
#57475=CARTESIAN_POINT('',(0.70231,-3.0900526918453,2.11901678258961));
#57476=CARTESIAN_POINT('',(0.2667,-3.0900526918453,3.37744668117609));
#57477=CARTESIAN_POINT('',(-0.451338313394325,-3.0900526918453,2.84404668117609));
#57478=CARTESIAN_POINT('',(-0.70231,-3.0900526918453,2.84404668117609));
#57479=CARTESIAN_POINT('',(-0.2667,-3.0900526918453,3.37744668117609));
#57480=CARTESIAN_POINT('',(0.70231,-3.0900526918453,-8.4284733188239));
#57481=CARTESIAN_POINT('',(-4.15302828610066,-3.0900526918453,-8.42847331882391));
#57482=CARTESIAN_POINT('',(0.70231,-3.0900526918453,0.194826681176092));
#57483=CARTESIAN_POINT('Origin',(-0.70231,-0.156352691845301,0.194826681176092));
#57484=CARTESIAN_POINT('',(0.451338313394325,-0.156352691845301,2.84404668117609));
#57485=CARTESIAN_POINT('',(0.70231,-0.156352691845301,2.11901678258961));
#57486=CARTESIAN_POINT('',(0.2667,-0.156352691845301,3.37744668117609));
#57487=CARTESIAN_POINT('',(0.70231,-0.156352691845301,-8.42847331882391));
#57488=CARTESIAN_POINT('',(0.70231,-0.156352691845301,0.194826681176092));
#57489=CARTESIAN_POINT('',(-4.15302828610066,-0.156352691845301,-8.42847331882391));
#57490=CARTESIAN_POINT('',(-0.451338313394325,-0.156352691845301,2.84404668117609));
#57491=CARTESIAN_POINT('',(-0.2667,-0.156352691845301,3.37744668117609));
#57492=CARTESIAN_POINT('',(0.70231,-0.156352691845301,2.84404668117609));
#57493=CARTESIAN_POINT('Origin',(7.95655,-4.2101926918453,2.84404668117609));
#57494=CARTESIAN_POINT('',(0.451338313394325,-4.2101926918453,2.84404668117609));
#57495=CARTESIAN_POINT('',(-0.451338313394325,-4.2101926918453,2.84404668117609));
#57496=CARTESIAN_POINT('Origin',(5.334,3.2218473081547,0.194826681176092));
#57497=CARTESIAN_POINT('',(4.24429638772394,3.2218473081547,0.194826681176092));
#57498=CARTESIAN_POINT('',(3.92938,3.2218473081547,-1.22566934687279));
#57499=CARTESIAN_POINT('',(4.29534475917809,3.2218473081547,0.425091004392428));
#57500=CARTESIAN_POINT('',(5.01908361227606,3.2218473081547,0.194826681176092));
#57501=CARTESIAN_POINT('',(5.334,3.2218473081547,0.194826681176092));
#57502=CARTESIAN_POINT('',(5.334,3.2218473081547,-1.2256693468728));
#57503=CARTESIAN_POINT('',(5.0338362189082,3.2218473081547,0.128281972989317));
#57504=CARTESIAN_POINT('',(5.334,3.2218473081547,-8.42847331882391));
#57505=CARTESIAN_POINT('',(5.334,3.2218473081547,0.194826681176092));
#57506=CARTESIAN_POINT('',(3.92938,3.2218473081547,-8.42847331882391));
#57507=CARTESIAN_POINT('',(-4.15302828610066,3.2218473081547,-8.42847331882391));
#57508=CARTESIAN_POINT('',(3.92938,3.2218473081547,0.194826681176092));
#57509=CARTESIAN_POINT('Origin',(3.92938,0.2881473081547,0.194826681176092));
#57510=CARTESIAN_POINT('',(3.92938,0.2881473081547,-1.2256693468728));
#57511=CARTESIAN_POINT('',(3.92938,0.2881473081547,-8.42847331882391));
#57512=CARTESIAN_POINT('',(3.92938,0.2881473081547,0.194826681176092));
#57513=CARTESIAN_POINT('',(3.92938,0.288147308154702,-1.2256693468728));
#57514=CARTESIAN_POINT('',(3.92938,-3.7123526918453,-8.42847331882391));
#57515=CARTESIAN_POINT('Origin',(3.92938,0.2881473081547,0.194826681176092));
#57516=CARTESIAN_POINT('',(4.24429638772394,0.2881473081547,0.194826681176092));
#57517=CARTESIAN_POINT('',(4.36283493912025,0.2881473081547,0.729519532971222));
#57518=CARTESIAN_POINT('',(5.334,0.2881473081547,-8.4284733188239));
#57519=CARTESIAN_POINT('',(-4.15302828610066,0.2881473081547,-8.42847331882391));
#57520=CARTESIAN_POINT('',(5.334,0.2881473081547,-1.22566934687279));
#57521=CARTESIAN_POINT('',(5.334,0.2881473081547,0.194826681176092));
#57522=CARTESIAN_POINT('',(5.01908361227606,0.2881473081547,0.194826681176092));
#57523=CARTESIAN_POINT('',(4.90054506087975,0.2881473081547,0.729519532971222));
#57524=CARTESIAN_POINT('',(3.92938,0.2881473081547,0.194826681176092));
#57525=CARTESIAN_POINT('Origin',(5.334,0.2881473081547,0.194826681176092));
#57526=CARTESIAN_POINT('',(4.24429638772394,0.2881473081547,0.194826681176092));
#57527=CARTESIAN_POINT('',(5.01908361227606,0.2881473081547,0.194826681176092));
#57528=CARTESIAN_POINT('Origin',(-5.334,3.2218473081547,0.194826681176092));
#57529=CARTESIAN_POINT('',(-5.334,3.2218473081547,-1.2256693468728));
#57530=CARTESIAN_POINT('',(-5.334,0.2881473081547,-1.22566934687279));
#57531=CARTESIAN_POINT('',(-5.334,3.2218473081547,-1.2256693468728));
#57532=CARTESIAN_POINT('',(-5.334,3.2218473081547,-8.4284733188239));
#57533=CARTESIAN_POINT('',(-5.334,3.2218473081547,0.194826681176092));
#57534=CARTESIAN_POINT('',(-5.334,0.2881473081547,-8.4284733188239));
#57535=CARTESIAN_POINT('',(-5.334,-3.7123526918453,-8.42847331882391));
#57536=CARTESIAN_POINT('',(-5.334,0.2881473081547,0.194826681176092));
#57537=CARTESIAN_POINT('Origin',(-3.92938,0.2881473081547,0.194826681176092));
#57538=CARTESIAN_POINT('',(-4.24429638772394,0.2881473081547,0.194826681176092));
#57539=CARTESIAN_POINT('',(-5.01908361227606,0.2881473081547,0.194826681176092));
#57540=CARTESIAN_POINT('',(-3.92938,0.2881473081547,0.194826681176092));
#57541=CARTESIAN_POINT('',(-4.90054506087975,0.2881473081547,0.729519532971223));
#57542=CARTESIAN_POINT('',(-3.92938,0.2881473081547,-8.4284733188239));
#57543=CARTESIAN_POINT('',(-4.15302828610066,0.2881473081547,-8.42847331882391));
#57544=CARTESIAN_POINT('',(-3.92938,0.2881473081547,-1.2256693468728));
#57545=CARTESIAN_POINT('',(-3.92938,0.2881473081547,0.194826681176092));
#57546=CARTESIAN_POINT('',(-4.36283493912025,0.2881473081547,0.729519532971223));
#57547=CARTESIAN_POINT('Origin',(-5.334,3.2218473081547,0.194826681176092));
#57548=CARTESIAN_POINT('',(-5.01908361227606,3.2218473081547,0.194826681176092));
#57549=CARTESIAN_POINT('',(-5.0338362189082,3.2218473081547,0.128281972989317));
#57550=CARTESIAN_POINT('',(-4.24429638772394,3.2218473081547,0.194826681176092));
#57551=CARTESIAN_POINT('',(-5.334,3.2218473081547,0.194826681176092));
#57552=CARTESIAN_POINT('',(-3.92938,3.2218473081547,-1.2256693468728));
#57553=CARTESIAN_POINT('',(-4.29534475917809,3.2218473081547,0.425091004392428));
#57554=CARTESIAN_POINT('',(-3.92938,3.2218473081547,-8.42847331882391));
#57555=CARTESIAN_POINT('',(-3.92938,3.2218473081547,0.194826681176092));
#57556=CARTESIAN_POINT('',(-4.15302828610066,3.2218473081547,-8.42847331882391));
#57557=CARTESIAN_POINT('Origin',(-5.334,0.2881473081547,0.194826681176092));
#57558=CARTESIAN_POINT('',(-5.01908361227606,0.2881473081547,0.194826681176092));
#57559=CARTESIAN_POINT('',(-4.24429638772394,0.2881473081547,0.194826681176092));
#57560=CARTESIAN_POINT('Origin',(-4.15302828610066,-3.7123526918453,-8.42847331882391));
#57561=CARTESIAN_POINT('',(-4.15302828610065,-5.4903526918453,-8.42847331882391));
#57562=CARTESIAN_POINT('',(-5.41026414305035,-4.96958854879497,-8.42847331882391));
#57563=CARTESIAN_POINT('Origin',(-4.15302828610066,-3.7123526918453,-8.42847331882391));
#57564=CARTESIAN_POINT('',(4.15302828610066,-5.4903526918453,-8.42847331882391));
#57565=CARTESIAN_POINT('',(4.15302828610066,-5.4903526918453,-8.42847331882391));
#57566=CARTESIAN_POINT('',(5.41026414305036,-4.96958854879497,-8.42847331882391));
#57567=CARTESIAN_POINT('Origin',(4.15302828610066,-3.7123526918453,-8.42847331882391));
#57568=CARTESIAN_POINT('',(7.92473585694968,-2.45511683489562,-8.42847331882391));
#57569=CARTESIAN_POINT('',(7.92473585694968,-2.45511683489562,-8.42847331882391));
#57570=CARTESIAN_POINT('',(8.4455,-1.19788097794593,-8.42847331882391));
#57571=CARTESIAN_POINT('Origin',(6.6675,-1.19788097794594,-8.42847331882391));
#57572=CARTESIAN_POINT('',(8.4455,3.84414730815469,-8.42847331882391));
#57573=CARTESIAN_POINT('',(8.4455,-1.19788097794593,-8.42847331882391));
#57574=CARTESIAN_POINT('',(6.66749999999999,5.6221473081547,-8.42847331882391));
#57575=CARTESIAN_POINT('Origin',(6.6675,3.8441473081547,-8.42847331882391));
#57576=CARTESIAN_POINT('',(-6.66749999999999,5.6221473081547,-8.42847331882391));
#57577=CARTESIAN_POINT('',(-6.66749999999999,5.6221473081547,-8.42847331882391));
#57578=CARTESIAN_POINT('',(-8.4455,3.84414730815469,-8.42847331882391));
#57579=CARTESIAN_POINT('Origin',(-6.6675,3.8441473081547,-8.42847331882391));
#57580=CARTESIAN_POINT('',(-8.4455,-1.19788097794593,-8.42847331882391));
#57581=CARTESIAN_POINT('',(-8.4455,3.84414730815469,-8.42847331882391));
#57582=CARTESIAN_POINT('',(-7.92473585694968,-2.45511683489562,-8.42847331882391));
#57583=CARTESIAN_POINT('Origin',(-6.6675,-1.19788097794594,-8.42847331882391));
#57584=CARTESIAN_POINT('',(-7.92473585694968,-2.45511683489562,-8.42847331882391));
#57585=CARTESIAN_POINT('',(-3.92938,-3.7123526918453,-8.42847331882391));
#57586=CARTESIAN_POINT('',(5.334,-3.71235269184531,-8.42847331882391));
#57587=CARTESIAN_POINT('',(0.70231,-3.7123526918453,-8.42847331882391));
#57588=CARTESIAN_POINT('Origin',(7.95655,-4.2101926918453,3.37744668117609));
#57589=CARTESIAN_POINT('',(-11.15695,4.34198730815467,3.37744668117609));
#57590=CARTESIAN_POINT('',(-11.15695,-4.21019269184528,3.37744668117609));
#57591=CARTESIAN_POINT('',(-11.15695,-4.2101926918453,3.37744668117609));
#57592=CARTESIAN_POINT('',(-7.95654999999997,-7.4105926918453,3.37744668117609));
#57593=CARTESIAN_POINT('Origin',(-7.95655,-4.2101926918453,3.37744668117609));
#57594=CARTESIAN_POINT('',(7.95654999999997,-7.4105926918453,3.37744668117609));
#57595=CARTESIAN_POINT('',(7.95654999999997,-7.4105926918453,3.37744668117609));
#57596=CARTESIAN_POINT('',(11.15695,-4.21019269184528,3.37744668117609));
#57597=CARTESIAN_POINT('Origin',(7.95655,-4.2101926918453,3.37744668117609));
#57598=CARTESIAN_POINT('',(11.15695,4.34198730815467,3.37744668117609));
#57599=CARTESIAN_POINT('',(11.15695,-4.2101926918453,3.37744668117609));
#57600=CARTESIAN_POINT('',(7.95654999999997,7.5423873081547,3.37744668117609));
#57601=CARTESIAN_POINT('Origin',(7.95655,4.3419873081547,3.37744668117609));
#57602=CARTESIAN_POINT('',(-7.95654999999997,7.5423873081547,3.37744668117609));
#57603=CARTESIAN_POINT('',(-7.95654999999997,7.5423873081547,3.37744668117609));
#57604=CARTESIAN_POINT('Origin',(-7.95655,4.3419873081547,3.37744668117609));
#57605=CARTESIAN_POINT('',(-4.15302828610065,-5.4903526918453,3.37744668117609));
#57606=CARTESIAN_POINT('',(-5.41026414305035,-4.96958854879497,3.37744668117609));
#57607=CARTESIAN_POINT('Origin',(-4.15302828610066,-3.7123526918453,3.37744668117609));
#57608=CARTESIAN_POINT('',(-7.92473585694968,-2.45511683489562,3.37744668117609));
#57609=CARTESIAN_POINT('',(-7.92473585694968,-2.45511683489562,3.37744668117609));
#57610=CARTESIAN_POINT('',(-8.4455,-1.19788097794593,3.37744668117609));
#57611=CARTESIAN_POINT('Origin',(-6.6675,-1.19788097794594,3.37744668117609));
#57612=CARTESIAN_POINT('',(-8.4455,3.84414730815469,3.37744668117609));
#57613=CARTESIAN_POINT('',(-8.4455,3.84414730815469,3.37744668117609));
#57614=CARTESIAN_POINT('',(-6.66749999999999,5.6221473081547,3.37744668117609));
#57615=CARTESIAN_POINT('Origin',(-6.6675,3.8441473081547,3.37744668117609));
#57616=CARTESIAN_POINT('',(6.66749999999999,5.6221473081547,3.37744668117609));
#57617=CARTESIAN_POINT('',(-6.66749999999999,5.6221473081547,3.37744668117609));
#57618=CARTESIAN_POINT('',(8.4455,3.84414730815469,3.37744668117609));
#57619=CARTESIAN_POINT('Origin',(6.6675,3.8441473081547,3.37744668117609));
#57620=CARTESIAN_POINT('',(8.4455,-1.19788097794593,3.37744668117609));
#57621=CARTESIAN_POINT('',(8.4455,-1.19788097794593,3.37744668117609));
#57622=CARTESIAN_POINT('',(7.92473585694968,-2.45511683489562,3.37744668117609));
#57623=CARTESIAN_POINT('Origin',(6.6675,-1.19788097794594,3.37744668117609));
#57624=CARTESIAN_POINT('',(5.41026414305036,-4.96958854879497,3.37744668117609));
#57625=CARTESIAN_POINT('',(7.92473585694968,-2.45511683489562,3.37744668117609));
#57626=CARTESIAN_POINT('',(4.15302828610066,-5.4903526918453,3.37744668117609));
#57627=CARTESIAN_POINT('Origin',(4.15302828610066,-3.7123526918453,3.37744668117609));
#57628=CARTESIAN_POINT('',(4.15302828610066,-5.4903526918453,3.37744668117609));
#57629=CARTESIAN_POINT('Origin',(7.95655,-4.2101926918453,-0.871973318823906));
#57630=CARTESIAN_POINT('',(-9.96068066769246,7.27943454458544,-0.871973318823906));
#57631=CARTESIAN_POINT('',(-9.96068066769246,7.27943454458544,-0.871973318823906));
#57632=CARTESIAN_POINT('',(-7.95654999999997,7.8979873081547,-0.871973318823906));
#57633=CARTESIAN_POINT('Origin',(-7.95655,4.3419873081547,-0.871973318823906));
#57634=CARTESIAN_POINT('',(7.95654999999997,7.8979873081547,-0.871973318823906));
#57635=CARTESIAN_POINT('',(-7.95654999999997,7.8979873081547,-0.871973318823906));
#57636=CARTESIAN_POINT('',(9.96068066769246,7.27943454458544,-0.871973318823906));
#57637=CARTESIAN_POINT('Origin',(7.95655,4.3419873081547,-0.871973318823906));
#57638=CARTESIAN_POINT('',(16.2281306676925,3.00334454458544,-0.871973318823906));
#57639=CARTESIAN_POINT('',(9.96068066769246,7.27943454458544,-0.871973318823906));
#57640=CARTESIAN_POINT('',(16.2281306676925,-2.87154992827604,-0.871973318823906));
#57641=CARTESIAN_POINT('Origin',(14.224,0.0658973081546998,-0.871973318823906));
#57642=CARTESIAN_POINT('',(9.96068066769245,-7.14763992827604,-0.871973318823906));
#57643=CARTESIAN_POINT('',(16.2281306676925,-2.87154992827604,-0.871973318823906));
#57644=CARTESIAN_POINT('',(7.95654999999997,-7.7661926918453,-0.871973318823906));
#57645=CARTESIAN_POINT('Origin',(7.95655,-4.2101926918453,-0.871973318823906));
#57646=CARTESIAN_POINT('',(-7.95654999999997,-7.7661926918453,-0.871973318823906));
#57647=CARTESIAN_POINT('',(7.95654999999997,-7.7661926918453,-0.871973318823906));
#57648=CARTESIAN_POINT('',(-9.96068066769245,-7.14763992827604,-0.871973318823906));
#57649=CARTESIAN_POINT('Origin',(-7.95655,-4.2101926918453,-0.871973318823906));
#57650=CARTESIAN_POINT('',(-16.2281306676925,-2.87154992827604,-0.871973318823906));
#57651=CARTESIAN_POINT('',(-6.66749999999998,6.7778473081547,-0.871973318823906));
#57652=CARTESIAN_POINT('',(6.66749999999998,6.7778473081547,-0.871973318823906));
#57653=CARTESIAN_POINT('',(-6.66749999999998,6.7778473081547,-0.871973318823906));
#57654=CARTESIAN_POINT('',(-9.3345,4.11084730815468,-0.871973318823906));
#57655=CARTESIAN_POINT('Origin',(-6.6675,4.1108473081547,-0.871973318823906));
#57656=CARTESIAN_POINT('',(-9.3345,-1.09634512099625,-0.871973318823906));
#57657=CARTESIAN_POINT('',(-9.3345,4.11084730815468,-0.871973318823906));
#57658=CARTESIAN_POINT('',(-8.55335378542452,-2.98219890642078,-0.871973318823906));
#57659=CARTESIAN_POINT('Origin',(-6.6675,-1.09634512099626,-0.871973318823906));
#57660=CARTESIAN_POINT('',(-5.67064621457553,-5.8649064772698,-0.871973318823906));
#57661=CARTESIAN_POINT('',(-8.55335378542452,-2.98219890642078,-0.871973318823906));
#57662=CARTESIAN_POINT('',(-3.78479242915098,-6.6460526918453,-0.871973318823906));
#57663=CARTESIAN_POINT('Origin',(-3.78479242915099,-3.9790526918453,-0.871973318823906));
#57664=CARTESIAN_POINT('',(3.784792429151,-6.6460526918453,-0.871973318823906));
#57665=CARTESIAN_POINT('',(3.784792429151,-6.6460526918453,-0.871973318823906));
#57666=CARTESIAN_POINT('',(5.67064621457553,-5.86490647726981,-0.871973318823906));
#57667=CARTESIAN_POINT('Origin',(3.78479242915099,-3.9790526918453,-0.871973318823906));
#57668=CARTESIAN_POINT('',(8.55335378542453,-2.98219890642078,-0.871973318823906));
#57669=CARTESIAN_POINT('',(8.55335378542453,-2.98219890642078,-0.871973318823906));
#57670=CARTESIAN_POINT('',(9.3345,-1.09634512099626,-0.871973318823906));
#57671=CARTESIAN_POINT('Origin',(6.6675,-1.09634512099626,-0.871973318823906));
#57672=CARTESIAN_POINT('',(9.3345,4.11084730815468,-0.871973318823906));
#57673=CARTESIAN_POINT('',(9.3345,-1.09634512099627,-0.871973318823906));
#57674=CARTESIAN_POINT('Origin',(6.6675,4.1108473081547,-0.871973318823906));
#57675=CARTESIAN_POINT('Origin',(-7.95655,4.3419873081547,3.37744668117609));
#57676=CARTESIAN_POINT('',(-11.51255,4.34198730815467,3.02184668117609));
#57677=CARTESIAN_POINT('',(-11.51255,4.34198730815467,1.33274668117609));
#57678=CARTESIAN_POINT('',(-11.51255,4.34198730815467,3.37744668117609));
#57679=CARTESIAN_POINT('',(-7.95654999999997,7.8979873081547,3.02184668117609));
#57680=CARTESIAN_POINT('Origin',(-7.95655,4.3419873081547,3.02184668117609));
#57681=CARTESIAN_POINT('',(-7.95654999999997,7.8979873081547,3.37744668117609));
#57682=CARTESIAN_POINT('',(-9.96068066769246,7.27943454458544,1.33274668117609));
#57683=CARTESIAN_POINT('',(-9.96068066769246,7.27943454458544,1.33274668117609));
#57684=CARTESIAN_POINT('Origin',(-7.95655,4.3419873081547,1.33274668117609));
#57685=CARTESIAN_POINT('Origin',(-11.51255,4.34198730815467,3.37744668117609));
#57686=CARTESIAN_POINT('',(-11.51255,-4.21019269184527,3.02184668117609));
#57687=CARTESIAN_POINT('',(-11.51255,-4.21019269184527,1.33274668117609));
#57688=CARTESIAN_POINT('',(-11.51255,-4.21019269184527,3.37744668117609));
#57689=CARTESIAN_POINT('',(-11.51255,4.34198730815467,3.02184668117609));
#57690=CARTESIAN_POINT('',(-11.51255,4.34198730815467,1.33274668117609));
#57691=CARTESIAN_POINT('Origin',(7.95655,-4.2101926918453,3.37744668117609));
#57692=CARTESIAN_POINT('',(11.51255,-4.21019269184527,3.02184668117609));
#57693=CARTESIAN_POINT('',(11.51255,-4.21019269184527,1.33274668117609));
#57694=CARTESIAN_POINT('',(11.51255,-4.21019269184527,3.37744668117609));
#57695=CARTESIAN_POINT('',(7.95654999999997,-7.7661926918453,3.02184668117609));
#57696=CARTESIAN_POINT('Origin',(7.95655,-4.2101926918453,3.02184668117609));
#57697=CARTESIAN_POINT('',(7.95654999999997,-7.7661926918453,3.37744668117609));
#57698=CARTESIAN_POINT('',(9.96068066769245,-7.14763992827604,1.33274668117609));
#57699=CARTESIAN_POINT('',(9.96068066769245,-7.14763992827604,1.33274668117609));
#57700=CARTESIAN_POINT('Origin',(7.95655,-4.2101926918453,1.33274668117609));
#57701=CARTESIAN_POINT('Origin',(11.51255,-4.21019269184527,3.37744668117609));
#57702=CARTESIAN_POINT('',(11.51255,4.34198730815467,3.02184668117609));
#57703=CARTESIAN_POINT('',(11.51255,4.34198730815467,1.33274668117609));
#57704=CARTESIAN_POINT('',(11.51255,4.34198730815467,3.37744668117609));
#57705=CARTESIAN_POINT('',(11.51255,-4.21019269184527,3.02184668117609));
#57706=CARTESIAN_POINT('',(11.51255,-4.21019269184527,1.33274668117609));
#57707=CARTESIAN_POINT('Origin',(7.95655,4.3419873081547,3.37744668117609));
#57708=CARTESIAN_POINT('',(7.95654999999997,7.8979873081547,3.02184668117609));
#57709=CARTESIAN_POINT('',(7.95654999999997,7.8979873081547,3.37744668117609));
#57710=CARTESIAN_POINT('Origin',(7.95655,4.3419873081547,3.02184668117609));
#57711=CARTESIAN_POINT('',(9.96068066769246,7.27943454458544,1.33274668117609));
#57712=CARTESIAN_POINT('Origin',(7.95655,4.3419873081547,1.33274668117609));
#57713=CARTESIAN_POINT('',(9.96068066769246,7.27943454458544,1.33274668117609));
#57714=CARTESIAN_POINT('Origin',(-7.95654999999997,7.8979873081547,3.37744668117609));
#57715=CARTESIAN_POINT('',(7.95654999999997,7.8979873081547,3.02184668117609));
#57716=CARTESIAN_POINT('Origin',(-7.95655,-4.2101926918453,3.37744668117609));
#57717=CARTESIAN_POINT('',(-7.95654999999997,-7.7661926918453,3.02184668117609));
#57718=CARTESIAN_POINT('',(-7.95654999999997,-7.7661926918453,3.37744668117609));
#57719=CARTESIAN_POINT('Origin',(-7.95655,-4.2101926918453,3.02184668117609));
#57720=CARTESIAN_POINT('',(-9.96068066769245,-7.14763992827604,1.33274668117609));
#57721=CARTESIAN_POINT('Origin',(-7.95655,-4.2101926918453,1.33274668117609));
#57722=CARTESIAN_POINT('',(-9.96068066769245,-7.14763992827604,1.33274668117609));
#57723=CARTESIAN_POINT('Origin',(7.95654999999997,-7.7661926918453,3.37744668117609));
#57724=CARTESIAN_POINT('',(-7.95654999999997,-7.7661926918453,3.02184668117609));
#57725=CARTESIAN_POINT('Origin',(16.2281306676925,-2.87154992827604,1.33274668117609));
#57726=CARTESIAN_POINT('',(16.2281306676925,-2.87154992827604,1.33274668117609));
#57727=CARTESIAN_POINT('',(16.2281306676925,-2.87154992827604,1.33274668117609));
#57728=CARTESIAN_POINT('',(16.2281306676925,-2.87154992827604,1.33274668117609));
#57729=CARTESIAN_POINT('Origin',(14.224,0.0658973081546998,1.33274668117609));
#57730=CARTESIAN_POINT('',(16.2281306676925,3.00334454458544,1.33274668117609));
#57731=CARTESIAN_POINT('',(16.2281306676925,3.00334454458544,1.33274668117609));
#57732=CARTESIAN_POINT('Origin',(14.224,0.0658973081546998,1.33274668117609));
#57733=CARTESIAN_POINT('Origin',(9.96068066769246,7.27943454458544,1.33274668117609));
#57734=CARTESIAN_POINT('',(9.96068066769246,7.27943454458544,1.33274668117609));
#57735=CARTESIAN_POINT('Origin',(7.95655,4.3419873081547,1.33274668117609));
#57736=CARTESIAN_POINT('Origin',(-9.96068066769246,7.27943454458544,1.33274668117609));
#57737=CARTESIAN_POINT('',(-9.96068066769246,7.27943454458544,1.33274668117609));
#57738=CARTESIAN_POINT('Origin',(-16.2281306676925,-2.87154992827604,1.33274668117609));
#57739=CARTESIAN_POINT('',(-16.2281306676925,-2.87154992827604,1.33274668117609));
#57740=CARTESIAN_POINT('Origin',(-7.95655,4.3419873081547,1.33274668117609));
#57741=CARTESIAN_POINT('Origin',(7.95655,4.3419873081547,3.02184668117609));
#57742=CARTESIAN_POINT('Origin',(7.95654999999997,7.5423873081547,3.02184668117609));
#57743=CARTESIAN_POINT('Origin',(11.15695,4.34198730815468,3.02184668117609));
#57744=CARTESIAN_POINT('Origin',(11.15695,-4.2101926918453,3.02184668117609));
#57745=CARTESIAN_POINT('Origin',(11.15695,-4.21019269184527,3.02184668117609));
#57746=CARTESIAN_POINT('Origin',(-7.95654999999997,7.5423873081547,3.02184668117609));
#57747=CARTESIAN_POINT('Origin',(-7.95654999999997,7.5423873081547,3.02184668117609));
#57748=CARTESIAN_POINT('Origin',(7.95655,-4.2101926918453,3.02184668117609));
#57749=CARTESIAN_POINT('Origin',(7.95654999999997,-7.4105926918453,3.02184668117609));
#57750=CARTESIAN_POINT('Origin',(-7.95655,4.3419873081547,3.02184668117609));
#57751=CARTESIAN_POINT('Origin',(-11.15695,4.34198730815467,3.02184668117609));
#57752=CARTESIAN_POINT('Origin',(7.95654999999997,-7.4105926918453,3.02184668117609));
#57753=CARTESIAN_POINT('Origin',(-7.95654999999997,-7.4105926918453,3.02184668117609));
#57754=CARTESIAN_POINT('Origin',(-11.15695,-4.2101926918453,3.02184668117609));
#57755=CARTESIAN_POINT('Origin',(-11.15695,-4.21019269184528,3.02184668117609));
#57756=CARTESIAN_POINT('Origin',(-7.95655,-4.2101926918453,3.02184668117609));
#57757=CARTESIAN_POINT('Origin',(-6.6675,4.1108473081547,-10.0286733188239));
#57758=CARTESIAN_POINT('',(-6.66749999999998,6.7778473081547,-10.0286733188239));
#57759=CARTESIAN_POINT('',(-9.3345,4.11084730815468,-10.0286733188239));
#57760=CARTESIAN_POINT('Origin',(-6.66749999999998,6.7778473081547,-10.0286733188239));
#57761=CARTESIAN_POINT('',(6.66749999999998,6.7778473081547,-10.0286733188239));
#57762=CARTESIAN_POINT('Origin',(6.6675,4.1108473081547,-10.0286733188239));
#57763=CARTESIAN_POINT('',(9.3345,4.11084730815468,-10.0286733188239));
#57764=CARTESIAN_POINT('Origin',(9.3345,-1.09634512099627,-10.0286733188239));
#57765=CARTESIAN_POINT('',(9.3345,-1.09634512099626,-10.0286733188239));
#57766=CARTESIAN_POINT('Origin',(6.6675,-1.09634512099626,-10.0286733188239));
#57767=CARTESIAN_POINT('',(8.55335378542453,-2.98219890642078,-10.0286733188239));
#57768=CARTESIAN_POINT('Origin',(8.55335378542453,-2.98219890642078,-10.0286733188239));
#57769=CARTESIAN_POINT('',(5.67064621457553,-5.86490647726981,-10.0286733188239));
#57770=CARTESIAN_POINT('Origin',(3.78479242915099,-3.9790526918453,-10.0286733188239));
#57771=CARTESIAN_POINT('',(3.784792429151,-6.6460526918453,-10.0286733188239));
#57772=CARTESIAN_POINT('Origin',(3.784792429151,-6.6460526918453,-10.0286733188239));
#57773=CARTESIAN_POINT('',(-3.78479242915098,-6.6460526918453,-10.0286733188239));
#57774=CARTESIAN_POINT('Origin',(-3.78479242915099,-3.9790526918453,-10.0286733188239));
#57775=CARTESIAN_POINT('',(-5.67064621457553,-5.8649064772698,-10.0286733188239));
#57776=CARTESIAN_POINT('Origin',(-8.55335378542452,-2.98219890642078,-10.0286733188239));
#57777=CARTESIAN_POINT('',(-8.55335378542452,-2.98219890642078,-10.0286733188239));
#57778=CARTESIAN_POINT('Origin',(-6.6675,-1.09634512099626,-10.0286733188239));
#57779=CARTESIAN_POINT('',(-9.3345,-1.09634512099625,-10.0286733188239));
#57780=CARTESIAN_POINT('Origin',(-9.3345,4.11084730815468,-10.0286733188239));
#57781=CARTESIAN_POINT('Origin',(-4.15302828610066,-3.7123526918453,-8.42847331882391));
#57782=CARTESIAN_POINT('',(-4.15302828610065,-5.4903526918453,-8.42847331882391));
#57783=CARTESIAN_POINT('',(-5.41026414305035,-4.96958854879497,-8.42847331882391));
#57784=CARTESIAN_POINT('Origin',(-7.92473585694968,-2.45511683489562,-8.42847331882391));
#57785=CARTESIAN_POINT('',(-7.92473585694968,-2.45511683489562,-8.42847331882391));
#57786=CARTESIAN_POINT('Origin',(-6.6675,-1.19788097794594,-8.42847331882391));
#57787=CARTESIAN_POINT('',(-8.4455,-1.19788097794593,-8.42847331882391));
#57788=CARTESIAN_POINT('Origin',(-8.4455,3.84414730815469,-8.42847331882391));
#57789=CARTESIAN_POINT('',(-8.4455,3.84414730815469,-8.42847331882391));
#57790=CARTESIAN_POINT('Origin',(-6.6675,3.8441473081547,-8.42847331882391));
#57791=CARTESIAN_POINT('',(-6.66749999999999,5.6221473081547,-8.42847331882391));
#57792=CARTESIAN_POINT('Origin',(-6.66749999999999,5.6221473081547,-8.42847331882391));
#57793=CARTESIAN_POINT('',(6.66749999999999,5.6221473081547,-8.42847331882391));
#57794=CARTESIAN_POINT('Origin',(6.6675,3.8441473081547,-8.42847331882391));
#57795=CARTESIAN_POINT('',(8.4455,3.84414730815469,-8.42847331882391));
#57796=CARTESIAN_POINT('Origin',(8.4455,-1.19788097794593,-8.42847331882391));
#57797=CARTESIAN_POINT('',(8.4455,-1.19788097794593,-8.42847331882391));
#57798=CARTESIAN_POINT('Origin',(6.6675,-1.19788097794594,-8.42847331882391));
#57799=CARTESIAN_POINT('',(7.92473585694968,-2.45511683489562,-8.42847331882391));
#57800=CARTESIAN_POINT('Origin',(7.92473585694968,-2.45511683489562,-8.42847331882391));
#57801=CARTESIAN_POINT('',(5.41026414305036,-4.96958854879497,-8.42847331882391));
#57802=CARTESIAN_POINT('Origin',(4.15302828610066,-3.7123526918453,-8.42847331882391));
#57803=CARTESIAN_POINT('',(4.15302828610066,-5.4903526918453,-8.42847331882391));
#57804=CARTESIAN_POINT('Origin',(4.15302828610066,-5.4903526918453,-8.42847331882391));
#57805=CARTESIAN_POINT('Origin',(0.70231,-3.0900526918453,0.194826681176092));
#57806=CARTESIAN_POINT('',(0.70231,-3.0900526918453,2.11901678258961));
#57807=CARTESIAN_POINT('Origin',(-3.92938,0.2881473081547,0.194826681176092));
#57808=CARTESIAN_POINT('',(-3.92938,0.288147308154702,-1.2256693468728));
#57809=CARTESIAN_POINT('Origin',(5.334,3.2218473081547,0.194826681176092));
#57810=CARTESIAN_POINT('',(5.334,3.2218473081547,-1.2256693468728));
#57811=CARTESIAN_POINT('Origin',(-4.36283493912025,9.41566770809984,0.729519532971223));
#57812=CARTESIAN_POINT('Origin',(-4.90054506087975,9.41566770809984,0.729519532971223));
#57813=CARTESIAN_POINT('Origin',(4.90054506087975,9.41566770809984,0.729519532971222));
#57814=CARTESIAN_POINT('Origin',(4.36283493912025,9.41566770809984,0.729519532971222));
#57815=CARTESIAN_POINT('Origin',(-0.2667,3.97571428641218,3.37744668117609));
#57816=CARTESIAN_POINT('Origin',(0.2667,3.97571428641218,3.37744668117609));
#57817=CARTESIAN_POINT('Origin',(1.41351,0.554847308154699,-11.0954733188239));
#57818=CARTESIAN_POINT('',(-1.41351,0.554847308154699,-11.0954733188239));
#57819=CARTESIAN_POINT('',(1.41351,0.554847308154699,-11.0954733188239));
#57820=CARTESIAN_POINT('',(-1.41351,0.554847308154699,-11.0954733188239));
#57821=CARTESIAN_POINT('',(1.41351,-3.8012526918453,-11.0954733188239));
#57822=CARTESIAN_POINT('',(1.41351,-3.8012526918453,-11.0954733188239));
#57823=CARTESIAN_POINT('',(-1.41351,-3.8012526918453,-11.0954733188239));
#57824=CARTESIAN_POINT('',(1.41351,-3.8012526918453,-11.0954733188239));
#57825=CARTESIAN_POINT('',(-1.41351,0.554847308154699,-11.0954733188239));
#57826=CARTESIAN_POINT('',(0.451338313394325,-0.156352691845301,-11.0954733188239));
#57827=CARTESIAN_POINT('',(-0.451338313394325,-0.156352691845301,-11.0954733188239));
#57828=CARTESIAN_POINT('',(-0.451338313394325,-0.156352691845301,-11.0954733188239));
#57829=CARTESIAN_POINT('',(-0.451338313394325,-3.0900526918453,-11.0954733188239));
#57830=CARTESIAN_POINT('',(-0.451338313394325,-3.0900526918453,-11.0954733188239));
#57831=CARTESIAN_POINT('',(0.451338313394325,-3.0900526918453,-11.0954733188239));
#57832=CARTESIAN_POINT('',(0.451338313394325,-3.0900526918453,-11.0954733188239));
#57833=CARTESIAN_POINT('',(0.451338313394325,-3.0900526918453,-11.0954733188239));
#57834=CARTESIAN_POINT('Origin',(-1.41351,0.554847308154699,-11.0954733188239));
#57835=CARTESIAN_POINT('',(1.41351,0.554847308154699,-11.0954733188239));
#57836=CARTESIAN_POINT('',(-1.41351,0.554847308154699,-11.0954733188239));
#57837=CARTESIAN_POINT('Origin',(1.41351,-3.8012526918453,-11.0954733188239));
#57838=CARTESIAN_POINT('',(1.41351,-3.8012526918453,-11.0954733188239));
#57839=CARTESIAN_POINT('Origin',(1.41351,-3.8012526918453,-11.0954733188239));
#57840=CARTESIAN_POINT('',(-1.41351,-3.8012526918453,-11.0954733188239));
#57841=CARTESIAN_POINT('Origin',(-1.41351,0.554847308154699,-11.0954733188239));
#57842=CARTESIAN_POINT('Origin',(-17.78,-1.6232026918453,-16.8055370922563));
#57843=CARTESIAN_POINT('',(-0.451338313394325,-1.06933891841287,-16.2516733188239));
#57844=CARTESIAN_POINT('',(-0.451338313394325,-0.156352691845301,-15.3386870922563));
#57845=CARTESIAN_POINT('',(-0.451338313394325,-2.07969580512908,-17.2620302055401));
#57846=CARTESIAN_POINT('',(0.451338313394325,-0.156352691845301,-15.3386870922563));
#57847=CARTESIAN_POINT('',(-0.451338313394325,-0.156352691845301,-15.3386870922563));
#57848=CARTESIAN_POINT('',(0.451338313394325,-1.06933891841287,-16.2516733188239));
#57849=CARTESIAN_POINT('',(0.451338313394325,-2.07969580512908,-17.2620302055401));
#57850=CARTESIAN_POINT('',(-0.451338313394325,-1.06933891841287,-16.2516733188239));
#57851=CARTESIAN_POINT('Origin',(-0.451338313394325,-3.0900526918453,-16.2516733188239));
#57852=CARTESIAN_POINT('',(0.451338313394325,-2.17706646527773,-16.2516733188239));
#57853=CARTESIAN_POINT('',(0.451338313394325,-3.0900526918453,-16.2516733188239));
#57854=CARTESIAN_POINT('',(-0.451338313394325,-2.17706646527773,-16.2516733188239));
#57855=CARTESIAN_POINT('',(-0.451338313394325,-2.17706646527773,-16.2516733188239));
#57856=CARTESIAN_POINT('',(-0.451338313394325,-3.0900526918453,-16.2516733188239));
#57857=CARTESIAN_POINT('Origin',(-17.78,-1.6232026918453,-16.8055370922563));
#57858=CARTESIAN_POINT('',(-0.451338313394325,-3.0900526918453,-15.3386870922563));
#57859=CARTESIAN_POINT('',(-0.451338313394325,-2.63355957856152,-15.7951802055401));
#57860=CARTESIAN_POINT('',(0.451338313394325,-3.0900526918453,-15.3386870922563));
#57861=CARTESIAN_POINT('',(0.451338313394325,-2.63355957856152,-15.7951802055401));
#57862=CARTESIAN_POINT('',(0.451338313394325,-3.0900526918453,-15.3386870922563));
#57863=CARTESIAN_POINT('Origin',(0.451338313394325,-3.0900526918453,-16.2516733188239));
#57864=CARTESIAN_POINT('',(-0.451338313394325,-3.0900526918453,-16.2516733188239));
#57865=CARTESIAN_POINT('',(0.451338313394325,-3.0900526918453,-16.2516733188239));
#57866=CARTESIAN_POINT('Origin',(0.451338313394325,-3.0900526918453,-16.2516733188239));
#57867=CARTESIAN_POINT('',(0.451338313394325,-0.156352691845301,-16.2516733188239));
#57868=CARTESIAN_POINT('Origin',(-0.451338313394325,-0.156352691845301,
-16.2516733188239));
#57869=CARTESIAN_POINT('',(-0.451338313394325,-0.156352691845301,-16.2516733188239));
#57870=CARTESIAN_POINT('Origin',(-0.451338313394325,-3.0900526918453,-16.2516733188239));
#57871=CARTESIAN_POINT('Origin',(3.21818,-0.4230526918453,-11.0954733188239));
#57872=CARTESIAN_POINT('',(3.21818,-0.4230526918453,-11.0954733188239));
#57873=CARTESIAN_POINT('',(3.21818,-0.4230526918453,-11.0954733188239));
#57874=CARTESIAN_POINT('',(6.0452,-0.4230526918453,-11.0954733188239));
#57875=CARTESIAN_POINT('',(3.21818,-0.4230526918453,-11.0954733188239));
#57876=CARTESIAN_POINT('',(6.0452,-0.4230526918453,-11.0954733188239));
#57877=CARTESIAN_POINT('Origin',(3.21818,-0.4230526918453,-11.0954733188239));
#57878=CARTESIAN_POINT('',(3.21818,3.9330473081547,-11.0954733188239));
#57879=CARTESIAN_POINT('',(3.21818,3.9330473081547,-11.0954733188239));
#57880=CARTESIAN_POINT('',(3.21818,-0.4230526918453,-11.0954733188239));
#57881=CARTESIAN_POINT('Origin',(6.0452,3.9330473081547,-11.0954733188239));
#57882=CARTESIAN_POINT('',(6.0452,3.9330473081547,-11.0954733188239));
#57883=CARTESIAN_POINT('',(6.0452,3.9330473081547,-11.0954733188239));
#57884=CARTESIAN_POINT('',(6.0452,3.9330473081547,-11.0954733188239));
#57885=CARTESIAN_POINT('Origin',(6.0452,3.9330473081547,-11.0954733188239));
#57886=CARTESIAN_POINT('',(6.0452,3.9330473081547,-11.0954733188239));
#57887=CARTESIAN_POINT('Origin',(6.0452,-0.423052691845299,-11.0954733188239));
#57888=CARTESIAN_POINT('',(5.01908361227606,3.2218473081547,-11.0954733188239));
#57889=CARTESIAN_POINT('',(5.01908361227606,0.2881473081547,-11.0954733188239));
#57890=CARTESIAN_POINT('',(5.01908361227606,3.2218473081547,-11.0954733188239));
#57891=CARTESIAN_POINT('',(4.24429638772394,3.2218473081547,-11.0954733188239));
#57892=CARTESIAN_POINT('',(5.01908361227606,3.2218473081547,-11.0954733188239));
#57893=CARTESIAN_POINT('',(4.24429638772394,0.2881473081547,-11.0954733188239));
#57894=CARTESIAN_POINT('',(4.24429638772394,3.2218473081547,-11.0954733188239));
#57895=CARTESIAN_POINT('',(4.24429638772394,0.2881473081547,-11.0954733188239));
#57896=CARTESIAN_POINT('Origin',(5.01908361227606,0.2881473081547,-16.2516733188239));
#57897=CARTESIAN_POINT('',(5.01908361227606,2.30886108158713,-16.2516733188239));
#57898=CARTESIAN_POINT('',(5.01908361227606,1.20113353472227,-16.2516733188239));
#57899=CARTESIAN_POINT('',(5.01908361227606,3.2218473081547,-16.2516733188239));
#57900=CARTESIAN_POINT('',(4.24429638772394,1.20113353472227,-16.2516733188239));
#57901=CARTESIAN_POINT('',(5.01908361227606,1.20113353472227,-16.2516733188239));
#57902=CARTESIAN_POINT('',(4.24429638772394,2.30886108158713,-16.2516733188239));
#57903=CARTESIAN_POINT('',(4.24429638772394,3.2218473081547,-16.2516733188239));
#57904=CARTESIAN_POINT('',(5.01908361227606,2.30886108158713,-16.2516733188239));
#57905=CARTESIAN_POINT('Origin',(-17.78,1.7549973081547,-16.8055370922563));
#57906=CARTESIAN_POINT('',(5.01908361227606,3.2218473081547,-15.3386870922563));
#57907=CARTESIAN_POINT('',(5.01908361227606,1.7549973081547,-16.8055370922563));
#57908=CARTESIAN_POINT('',(4.24429638772394,3.2218473081547,-15.3386870922563));
#57909=CARTESIAN_POINT('',(4.24429638772394,2.76535419487092,-15.7951802055401));
#57910=CARTESIAN_POINT('',(5.01908361227606,3.2218473081547,-15.3386870922563));
#57911=CARTESIAN_POINT('Origin',(-17.78,1.7549973081547,-16.8055370922563));
#57912=CARTESIAN_POINT('',(5.01908361227606,0.2881473081547,-15.3386870922563));
#57913=CARTESIAN_POINT('',(4.24429638772394,0.2881473081547,-15.3386870922563));
#57914=CARTESIAN_POINT('',(4.24429638772394,0.2881473081547,-15.3386870922563));
#57915=CARTESIAN_POINT('',(4.24429638772394,2.21149042143848,-17.2620302055401));
#57916=CARTESIAN_POINT('',(5.01908361227606,1.7549973081547,-16.8055370922563));
#57917=CARTESIAN_POINT('Origin',(4.24429638772394,0.2881473081547,-16.2516733188239));
#57918=CARTESIAN_POINT('',(4.24429638772394,0.2881473081547,-16.2516733188239));
#57919=CARTESIAN_POINT('',(5.01908361227606,0.2881473081547,-16.2516733188239));
#57920=CARTESIAN_POINT('Origin',(5.01908361227606,3.2218473081547,-16.2516733188239));
#57921=CARTESIAN_POINT('',(5.01908361227606,3.2218473081547,-16.2516733188239));
#57922=CARTESIAN_POINT('',(4.24429638772394,3.2218473081547,-16.2516733188239));
#57923=CARTESIAN_POINT('Origin',(4.24429638772394,3.2218473081547,-16.2516733188239));
#57924=CARTESIAN_POINT('Origin',(5.01908361227606,3.2218473081547,-16.2516733188239));
#57925=CARTESIAN_POINT('Origin',(-3.21818,-0.4230526918453,-11.0954733188239));
#57926=CARTESIAN_POINT('',(-3.21818,-0.4230526918453,-11.0954733188239));
#57927=CARTESIAN_POINT('',(-3.21818,3.9330473081547,-11.0954733188239));
#57928=CARTESIAN_POINT('',(-3.21818,-0.4230526918453,-11.0954733188239));
#57929=CARTESIAN_POINT('',(-6.0452,-0.4230526918453,-11.0954733188239));
#57930=CARTESIAN_POINT('',(-3.21818,-0.4230526918453,-11.0954733188239));
#57931=CARTESIAN_POINT('',(-6.0452,3.9330473081547,-11.0954733188239));
#57932=CARTESIAN_POINT('',(-6.0452,3.9330473081547,-11.0954733188239));
#57933=CARTESIAN_POINT('',(-6.0452,3.9330473081547,-11.0954733188239));
#57934=CARTESIAN_POINT('',(-4.24429638772394,3.2218473081547,-11.0954733188239));
#57935=CARTESIAN_POINT('',(-4.24429638772394,0.2881473081547,-11.0954733188239));
#57936=CARTESIAN_POINT('',(-4.24429638772394,0.2881473081547,-11.0954733188239));
#57937=CARTESIAN_POINT('',(-5.01908361227606,3.2218473081547,-11.0954733188239));
#57938=CARTESIAN_POINT('',(-5.01908361227606,3.2218473081547,-11.0954733188239));
#57939=CARTESIAN_POINT('',(-5.01908361227606,0.2881473081547,-11.0954733188239));
#57940=CARTESIAN_POINT('',(-5.01908361227606,0.2881473081547,-11.0954733188239));
#57941=CARTESIAN_POINT('',(-4.24429638772394,0.2881473081547,-11.0954733188239));
#57942=CARTESIAN_POINT('Origin',(-3.21818,-0.4230526918453,-11.0954733188239));
#57943=CARTESIAN_POINT('',(-3.21818,-0.4230526918453,-11.0954733188239));
#57944=CARTESIAN_POINT('',(-3.21818,3.9330473081547,-11.0954733188239));
#57945=CARTESIAN_POINT('Origin',(-3.21818,-0.4230526918453,-11.0954733188239));
#57946=CARTESIAN_POINT('',(-6.0452,-0.4230526918453,-11.0954733188239));
#57947=CARTESIAN_POINT('Origin',(-6.0452,3.9330473081547,-11.0954733188239));
#57948=CARTESIAN_POINT('',(-6.0452,3.9330473081547,-11.0954733188239));
#57949=CARTESIAN_POINT('Origin',(-6.0452,3.9330473081547,-11.0954733188239));
#57950=CARTESIAN_POINT('Origin',(-4.24429638772394,3.2218473081547,-16.2516733188239));
#57951=CARTESIAN_POINT('',(-5.01908361227606,1.20113353472227,-16.2516733188239));
#57952=CARTESIAN_POINT('',(-4.24429638772394,1.20113353472227,-16.2516733188239));
#57953=CARTESIAN_POINT('',(-4.24429638772394,1.20113353472227,-16.2516733188239));
#57954=CARTESIAN_POINT('',(-5.01908361227606,2.30886108158713,-16.2516733188239));
#57955=CARTESIAN_POINT('',(-5.01908361227606,0.2881473081547,-16.2516733188239));
#57956=CARTESIAN_POINT('',(-4.24429638772394,2.30886108158713,-16.2516733188239));
#57957=CARTESIAN_POINT('',(-4.24429638772394,2.30886108158713,-16.2516733188239));
#57958=CARTESIAN_POINT('',(-4.24429638772394,0.2881473081547,-16.2516733188239));
#57959=CARTESIAN_POINT('Origin',(-17.78,1.7549973081547,-16.8055370922563));
#57960=CARTESIAN_POINT('',(-5.01908361227606,3.2218473081547,-15.3386870922563));
#57961=CARTESIAN_POINT('',(-4.24429638772394,3.2218473081547,-15.3386870922563));
#57962=CARTESIAN_POINT('',(-5.01908361227606,3.2218473081547,-15.3386870922563));
#57963=CARTESIAN_POINT('',(-4.24429638772394,1.29850419487091,-17.2620302055401));
#57964=CARTESIAN_POINT('',(-5.01908361227606,1.29850419487091,-17.2620302055401));
#57965=CARTESIAN_POINT('Origin',(-17.78,1.7549973081547,-16.8055370922563));
#57966=CARTESIAN_POINT('',(-4.24429638772394,0.2881473081547,-15.3386870922563));
#57967=CARTESIAN_POINT('',(-4.24429638772394,0.744640421438487,-15.7951802055401));
#57968=CARTESIAN_POINT('',(-5.01908361227606,0.2881473081547,-15.3386870922563));
#57969=CARTESIAN_POINT('',(-4.24429638772394,0.2881473081547,-15.3386870922563));
#57970=CARTESIAN_POINT('',(-5.01908361227606,0.744640421438487,-15.7951802055401));
#57971=CARTESIAN_POINT('Origin',(-4.24429638772394,0.2881473081547,-16.2516733188239));
#57972=CARTESIAN_POINT('',(-5.01908361227606,0.2881473081547,-16.2516733188239));
#57973=CARTESIAN_POINT('',(-4.24429638772394,0.2881473081547,-16.2516733188239));
#57974=CARTESIAN_POINT('Origin',(-5.01908361227606,3.2218473081547,-16.2516733188239));
#57975=CARTESIAN_POINT('',(-4.24429638772394,3.2218473081547,-16.2516733188239));
#57976=CARTESIAN_POINT('',(-5.01908361227606,3.2218473081547,-16.2516733188239));
#57977=CARTESIAN_POINT('Origin',(-5.01908361227606,0.2881473081547,-16.2516733188239));
#57978=CARTESIAN_POINT('Origin',(-4.24429638772394,0.2881473081547,-16.2516733188239));
#57979=CARTESIAN_POINT('',(0.,0.,0.));
#57980=CARTESIAN_POINT('Origin',(-1.03877763349493,4.27252044680983E-8,
-2.34921160237358));
#57981=CARTESIAN_POINT('',(-7.78877763349493,4.6250000427252,-2.34921160237359));
#57982=CARTESIAN_POINT('',(-7.78877763349493,-4.6249999572748,-2.34921160237358));
#57983=CARTESIAN_POINT('',(-7.78877763349493,4.6250000427252,-2.34921160237358));
#57984=CARTESIAN_POINT('',(5.71122236650507,4.6250000427252,-2.34921160237359));
#57985=CARTESIAN_POINT('',(-7.78877763349493,4.6250000427252,-2.34921160237358));
#57986=CARTESIAN_POINT('',(5.71122236650507,-4.6249999572748,-2.34921160237359));
#57987=CARTESIAN_POINT('',(5.71122236650507,4.6250000427252,-2.34921160237358));
#57988=CARTESIAN_POINT('',(-7.78877763349493,-4.6249999572748,-2.34921160237358));
#57989=CARTESIAN_POINT('Origin',(-1.03877763349493,4.27252044680983E-8,
-5.84921160237358));
#57990=CARTESIAN_POINT('',(-7.78877763349493,-4.62499995727479,-5.84921160237358));
#57991=CARTESIAN_POINT('',(5.71122236650507,-4.6249999572748,-5.84921160237358));
#57992=CARTESIAN_POINT('',(-7.78877763349493,-4.62499995727479,-5.84921160237358));
#57993=CARTESIAN_POINT('',(5.71122236650507,4.6250000427252,-5.84921160237359));
#57994=CARTESIAN_POINT('',(5.71122236650507,-4.6249999572748,-5.84921160237358));
#57995=CARTESIAN_POINT('',(-7.78877763349493,4.6250000427252,-5.84921160237358));
#57996=CARTESIAN_POINT('',(-7.78877763349493,4.6250000427252,-5.84921160237358));
#57997=CARTESIAN_POINT('',(-7.78877763349493,-4.62499995727479,-5.84921160237358));
#57998=CARTESIAN_POINT('Origin',(-7.78877763349493,-4.62499995727479,-22.4641894514267));
#57999=CARTESIAN_POINT('',(5.71122236650507,-4.6249999572748,-22.4641894514267));
#58000=CARTESIAN_POINT('',(-7.78877763349493,-4.62499995727479,-22.4641894514267));
#58001=CARTESIAN_POINT('Origin',(-7.78877763349493,-4.62499995727479,-22.4641894514267));
#58002=CARTESIAN_POINT('',(-7.78877763349493,4.6250000427252,-22.4641894514267));
#58003=CARTESIAN_POINT('Origin',(-7.78877763349493,4.6250000427252,-22.4641894514267));
#58004=CARTESIAN_POINT('',(5.71122236650507,4.6250000427252,-22.4641894514267));
#58005=CARTESIAN_POINT('Origin',(5.71122236650507,-4.6249999572748,-22.4641894514267));
#58006=CARTESIAN_POINT('Origin',(-8.28877763349493,4.2725226612629E-8,-10.3492116023736));
#58007=CARTESIAN_POINT('',(-1.53877763349493,-0.999999957274778,-10.3492116023736));
#58008=CARTESIAN_POINT('Origin',(-1.53877763349493,4.27252241731742E-8,
-10.3492116023736));
#58009=CARTESIAN_POINT('',(-0.538777633494928,-0.999999957274778,-10.3492116023736));
#58010=CARTESIAN_POINT('',(-8.28877763349493,-0.999999957274775,-10.3492116023736));
#58011=CARTESIAN_POINT('Origin',(-0.538777633494929,4.27252238117734E-8,
-10.3492116023736));
#58012=CARTESIAN_POINT('Origin',(-8.28877763349493,4.2725226612629E-8,-10.3492116023736));
#58013=CARTESIAN_POINT('',(-6.53877763349493,-0.999999957274776,-10.3492116023736));
#58014=CARTESIAN_POINT('Origin',(-6.53877763349493,4.27252259801778E-8,
-10.3492116023736));
#58015=CARTESIAN_POINT('',(-5.53877763349493,-0.999999957274776,-10.3492116023736));
#58016=CARTESIAN_POINT('',(-8.28877763349493,-0.999999957274775,-10.3492116023736));
#58017=CARTESIAN_POINT('Origin',(-5.53877763349493,4.27252256187771E-8,
-10.3492116023736));
#58018=CARTESIAN_POINT('Origin',(12.9485298756357,4.6250000427252,55.4311528842592));
#58019=CARTESIAN_POINT('',(-7.78877763349493,4.6250000427252,3.41227095402391));
#58020=CARTESIAN_POINT('',(5.71122236650507,4.6250000427252,-0.0992116023735834));
#58021=CARTESIAN_POINT('Origin',(12.9485298756357,4.6250000427252,55.4311528842592));
#58022=CARTESIAN_POINT('',(-7.78877763349493,-4.6249999572748,3.41227095402391));
#58023=CARTESIAN_POINT('',(-7.78877763349493,4.6250000427252,3.41227095402391));
#58024=CARTESIAN_POINT('',(5.71122236650507,-4.6249999572748,-0.0992116023735834));
#58025=CARTESIAN_POINT('Origin',(12.9485298756357,-4.6249999572748,55.4311528842592));
#58026=CARTESIAN_POINT('',(5.71122236650507,4.6250000427252,-0.0992116023735834));
#58027=CARTESIAN_POINT('Origin',(-0.0387776334949297,-3.74999995727479,
-6.34921160237358));
#58028=CARTESIAN_POINT('',(-0.53877763349493,-3.74999995727479,-6.34921160237358));
#58029=CARTESIAN_POINT('',(-0.53877763349493,-3.74999995727479,-6.09921160237358));
#58030=CARTESIAN_POINT('',(-0.53877763349493,-3.74999995727479,-6.34921160237358));
#58031=CARTESIAN_POINT('',(-0.0387776334949297,-3.74999995727479,-6.34921160237358));
#58032=CARTESIAN_POINT('',(-0.0387776334949297,-3.74999995727479,-6.34921160237358));
#58033=CARTESIAN_POINT('',(-0.0387776334949297,-3.74999995727479,-6.09921160237358));
#58034=CARTESIAN_POINT('',(-0.0387776334949297,-3.74999995727479,-6.34921160237358));
#58035=CARTESIAN_POINT('',(-0.0387776334949297,-3.74999995727479,-6.09921160237358));
#58036=CARTESIAN_POINT('Origin',(-0.0387776334949297,3.75000004272521,-6.34921160237358));
#58037=CARTESIAN_POINT('',(-0.0387776334949297,3.75000004272521,-6.34921160237358));
#58038=CARTESIAN_POINT('',(-0.538777633494927,3.75000004272521,-6.34921160237358));
#58039=CARTESIAN_POINT('',(-0.0387776334949297,3.75000004272521,-6.34921160237358));
#58040=CARTESIAN_POINT('',(-0.53877763349493,3.75000004272521,-6.09921160237358));
#58041=CARTESIAN_POINT('',(-0.53877763349493,3.75000004272521,-6.34921160237358));
#58042=CARTESIAN_POINT('',(-0.0387776334949297,3.75000004272521,-6.09921160237358));
#58043=CARTESIAN_POINT('',(-0.0387776334949297,3.75000004272521,-6.09921160237358));
#58044=CARTESIAN_POINT('',(-0.0387776334949297,3.75000004272521,-6.34921160237358));
#58045=CARTESIAN_POINT('Origin',(-0.0387776334949297,-3.74999995727479,
-6.34921160237358));
#58046=CARTESIAN_POINT('',(-0.53877763349493,-3.74999995727479,-10.0992116023736));
#58047=CARTESIAN_POINT('',(-0.53877763349493,-3.74999995727479,-13.0992116023736));
#58048=CARTESIAN_POINT('',(-1.53877763349493,-3.74999995727479,-6.09921160237358));
#58049=CARTESIAN_POINT('',(-0.0387776334949297,-3.74999995727479,-6.09921160237358));
#58050=CARTESIAN_POINT('',(-1.53877763349493,-3.74999995727479,-6.34921160237358));
#58051=CARTESIAN_POINT('',(-1.53877763349493,-3.74999995727479,-6.34921160237358));
#58052=CARTESIAN_POINT('',(-1.53877763349493,-3.74999995727479,-10.0992116023736));
#58053=CARTESIAN_POINT('',(-1.53877763349493,-3.74999995727479,-13.0992116023736));
#58054=CARTESIAN_POINT('',(6.21122236650507,-3.74999995727479,-10.0992116023736));
#58055=CARTESIAN_POINT('Origin',(-0.0387776334949297,3.75000004272521,-6.34921160237358));
#58056=CARTESIAN_POINT('',(-0.538777633494927,3.75000004272521,-10.0992116023736));
#58057=CARTESIAN_POINT('',(-0.538777633494927,3.75000004272521,-13.0992116023736));
#58058=CARTESIAN_POINT('',(-1.53877763349493,3.75000004272521,-10.0992116023736));
#58059=CARTESIAN_POINT('',(6.21122236650507,3.75000004272521,-10.0992116023736));
#58060=CARTESIAN_POINT('',(-1.53877763349493,3.75000004272521,-6.34921160237358));
#58061=CARTESIAN_POINT('',(-1.53877763349493,3.75000004272521,-13.0992116023736));
#58062=CARTESIAN_POINT('',(-1.53877763349493,3.75000004272521,-6.09921160237358));
#58063=CARTESIAN_POINT('',(-1.53877763349493,3.75000004272521,-6.34921160237358));
#58064=CARTESIAN_POINT('',(-0.0387776334949297,3.75000004272521,-6.09921160237358));
#58065=CARTESIAN_POINT('Origin',(-5.03877763349493,3.75000004272521,-6.34921160237358));
#58066=CARTESIAN_POINT('',(-5.03877763349493,3.75000004272521,-6.34921160237358));
#58067=CARTESIAN_POINT('',(-5.53877763349493,3.75000004272521,-6.34921160237358));
#58068=CARTESIAN_POINT('',(-5.03877763349493,3.75000004272521,-6.34921160237358));
#58069=CARTESIAN_POINT('',(-5.53877763349493,3.75000004272521,-6.09921160237358));
#58070=CARTESIAN_POINT('',(-5.53877763349493,3.75000004272521,-6.34921160237358));
#58071=CARTESIAN_POINT('',(-5.03877763349493,3.75000004272521,-6.09921160237358));
#58072=CARTESIAN_POINT('',(-5.03877763349493,3.75000004272521,-6.09921160237358));
#58073=CARTESIAN_POINT('',(-5.03877763349493,3.75000004272521,-6.34921160237358));
#58074=CARTESIAN_POINT('Origin',(-5.03877763349493,-3.74999995727479,-6.34921160237358));
#58075=CARTESIAN_POINT('',(-5.53877763349493,-3.74999995727479,-6.34921160237358));
#58076=CARTESIAN_POINT('',(-5.53877763349493,-3.74999995727479,-6.09921160237358));
#58077=CARTESIAN_POINT('',(-5.53877763349493,-3.74999995727479,-6.34921160237358));
#58078=CARTESIAN_POINT('',(-5.03877763349493,-3.74999995727479,-6.34921160237358));
#58079=CARTESIAN_POINT('',(-5.03877763349493,-3.74999995727479,-6.34921160237358));
#58080=CARTESIAN_POINT('',(-5.03877763349493,-3.74999995727479,-6.09921160237358));
#58081=CARTESIAN_POINT('',(-5.03877763349493,-3.74999995727479,-6.34921160237358));
#58082=CARTESIAN_POINT('',(-5.03877763349493,-3.74999995727479,-6.09921160237358));
#58083=CARTESIAN_POINT('Origin',(-5.03877763349493,3.75000004272521,-6.34921160237358));
#58084=CARTESIAN_POINT('',(-5.53877763349493,3.75000004272521,-10.0992116023736));
#58085=CARTESIAN_POINT('',(-5.53877763349493,3.75000004272521,-13.0992116023736));
#58086=CARTESIAN_POINT('',(-6.53877763349493,3.75000004272521,-10.0992116023736));
#58087=CARTESIAN_POINT('',(6.21122236650507,3.75000004272521,-10.0992116023736));
#58088=CARTESIAN_POINT('',(-6.53877763349493,3.75000004272521,-6.34921160237358));
#58089=CARTESIAN_POINT('',(-6.53877763349493,3.75000004272521,-13.0992116023736));
#58090=CARTESIAN_POINT('',(-6.53877763349493,3.75000004272521,-6.09921160237358));
#58091=CARTESIAN_POINT('',(-6.53877763349493,3.75000004272521,-6.34921160237358));
#58092=CARTESIAN_POINT('',(-5.03877763349493,3.75000004272521,-6.09921160237358));
#58093=CARTESIAN_POINT('Origin',(-5.03877763349493,-3.74999995727479,-6.34921160237358));
#58094=CARTESIAN_POINT('',(-5.53877763349493,-3.74999995727479,-10.0992116023736));
#58095=CARTESIAN_POINT('',(-5.53877763349493,-3.74999995727479,-13.0992116023736));
#58096=CARTESIAN_POINT('',(-6.53877763349493,-3.74999995727479,-6.09921160237358));
#58097=CARTESIAN_POINT('',(-5.03877763349493,-3.74999995727479,-6.09921160237358));
#58098=CARTESIAN_POINT('',(-6.53877763349493,-3.74999995727479,-6.34921160237358));
#58099=CARTESIAN_POINT('',(-6.53877763349493,-3.74999995727479,-6.34921160237358));
#58100=CARTESIAN_POINT('',(-6.53877763349493,-3.74999995727479,-10.0992116023736));
#58101=CARTESIAN_POINT('',(-6.53877763349493,-3.74999995727479,-13.0992116023736));
#58102=CARTESIAN_POINT('',(6.21122236650507,-3.74999995727479,-10.0992116023736));
#58103=CARTESIAN_POINT('Origin',(-1.03877763349493,4.27252044680983E-8,
-6.09921160237358));
#58104=CARTESIAN_POINT('',(6.08622236650508,-4.9999999572748,-6.09921160237358));
#58105=CARTESIAN_POINT('',(-8.16377763349493,-4.99999995727479,-6.09921160237358));
#58106=CARTESIAN_POINT('',(6.08622236650508,-4.9999999572748,-6.09921160237358));
#58107=CARTESIAN_POINT('',(-8.16377763349493,5.00000004272521,-6.09921160237358));
#58108=CARTESIAN_POINT('',(-8.16377763349493,-4.99999995727479,-6.09921160237358));
#58109=CARTESIAN_POINT('',(6.08622236650508,5.00000004272521,-6.09921160237358));
#58110=CARTESIAN_POINT('',(-8.16377763349493,5.00000004272521,-6.09921160237358));
#58111=CARTESIAN_POINT('',(6.08622236650508,5.00000004272521,-6.09921160237358));
#58112=CARTESIAN_POINT('',(-2.03877763349493,-3.74999995727479,-6.09921160237358));
#58113=CARTESIAN_POINT('',(-2.03877763349493,3.75000004272521,-6.09921160237358));
#58114=CARTESIAN_POINT('',(-2.03877763349493,-3.74999995727479,-6.09921160237358));
#58115=CARTESIAN_POINT('',(-0.0387776334949297,-3.74999995727479,-6.09921160237358));
#58116=CARTESIAN_POINT('',(-0.0387776334949297,-3.74999995727479,-6.09921160237358));
#58117=CARTESIAN_POINT('',(-0.0387776334949297,3.75000004272521,-6.09921160237358));
#58118=CARTESIAN_POINT('',(-7.03877763349493,-3.74999995727479,-6.09921160237358));
#58119=CARTESIAN_POINT('',(-7.03877763349493,3.75000004272521,-6.09921160237358));
#58120=CARTESIAN_POINT('',(-7.03877763349493,-3.74999995727479,-6.09921160237358));
#58121=CARTESIAN_POINT('',(-5.03877763349493,-3.74999995727479,-6.09921160237358));
#58122=CARTESIAN_POINT('',(-5.03877763349493,-3.74999995727479,-6.09921160237358));
#58123=CARTESIAN_POINT('',(-5.03877763349493,3.75000004272521,-6.09921160237358));
#58124=CARTESIAN_POINT('Origin',(-1.03877763349493,4.27252044680983E-8,
-1.09921160237358));
#58125=CARTESIAN_POINT('',(-8.28877763349493,5.1250000427252,-1.09921160237358));
#58126=CARTESIAN_POINT('',(6.21122236650508,5.12500004272521,-1.09921160237358));
#58127=CARTESIAN_POINT('',(-8.28877763349493,5.1250000427252,-1.09921160237358));
#58128=CARTESIAN_POINT('',(6.21122236650507,-5.1249999572748,-1.09921160237358));
#58129=CARTESIAN_POINT('',(6.21122236650507,-5.1249999572748,-1.09921160237358));
#58130=CARTESIAN_POINT('',(-8.28877763349493,-5.1249999572748,-1.09921160237358));
#58131=CARTESIAN_POINT('',(-8.28877763349493,-5.1249999572748,-1.09921160237358));
#58132=CARTESIAN_POINT('',(-8.28877763349493,-5.1249999572748,-1.09921160237358));
#58133=CARTESIAN_POINT('',(6.08622236650507,5.00000004272521,-1.09921160237358));
#58134=CARTESIAN_POINT('',(6.08622236650507,-4.99999995727479,-1.09921160237358));
#58135=CARTESIAN_POINT('',(6.08622236650507,5.00000004272521,-1.09921160237358));
#58136=CARTESIAN_POINT('',(5.88622236650507,5.00000004272521,-1.09921160237358));
#58137=CARTESIAN_POINT('',(6.08622236650507,5.00000004272521,-1.09921160237358));
#58138=CARTESIAN_POINT('',(-1.03877763349493,5.00000004272521,-1.09921160237358));
#58139=CARTESIAN_POINT('',(-8.16377763349493,5.00000004272521,-1.09921160237358));
#58140=CARTESIAN_POINT('',(-7.96377763349493,5.00000004272521,-1.09921160237358));
#58141=CARTESIAN_POINT('',(-8.16377763349493,5.00000004272521,-1.09921160237358));
#58142=CARTESIAN_POINT('',(-8.16377763349493,5.00000004272521,-1.09921160237358));
#58143=CARTESIAN_POINT('',(-8.16377763349493,5.00000004272521,-1.09921160237358));
#58144=CARTESIAN_POINT('',(-8.16377763349493,-4.99999995727479,-1.09921160237358));
#58145=CARTESIAN_POINT('',(-8.16377763349493,5.00000004272521,-1.09921160237358));
#58146=CARTESIAN_POINT('',(-7.96377763349493,-4.99999995727479,-1.09921160237358));
#58147=CARTESIAN_POINT('',(-8.16377763349493,-4.99999995727479,-1.09921160237358));
#58148=CARTESIAN_POINT('',(-1.03877763349493,-4.99999995727479,-1.09921160237358));
#58149=CARTESIAN_POINT('',(6.08622236650508,-4.9999999572748,-1.09921160237358));
#58150=CARTESIAN_POINT('',(5.88622236650507,-4.99999995727479,-1.09921160237358));
#58151=CARTESIAN_POINT('',(6.08622236650508,-4.9999999572748,-1.09921160237358));
#58152=CARTESIAN_POINT('',(6.08622236650507,-4.99999995727479,-1.09921160237358));
#58153=CARTESIAN_POINT('Origin',(-8.28877763349493,-5.1249999572748,-0.349211602373583));
#58154=CARTESIAN_POINT('',(6.21122236650507,-5.1249999572748,-0.349211602373583));
#58155=CARTESIAN_POINT('',(6.21122236650507,-5.1249999572748,-0.349211602373583));
#58156=CARTESIAN_POINT('',(-8.28877763349493,-5.1249999572748,-0.349211602373583));
#58157=CARTESIAN_POINT('',(-8.28877763349493,-5.1249999572748,-0.349211602373583));
#58158=CARTESIAN_POINT('',(-8.28877763349493,-5.1249999572748,-0.349211602373583));
#58159=CARTESIAN_POINT('Origin',(6.21122236650507,-5.1249999572748,-0.349211602373583));
#58160=CARTESIAN_POINT('',(6.21122236650508,5.12500004272521,-0.349211602373583));
#58161=CARTESIAN_POINT('',(6.21122236650508,5.12500004272521,-0.349211602373583));
#58162=CARTESIAN_POINT('',(6.21122236650507,-5.1249999572748,-0.349211602373583));
#58163=CARTESIAN_POINT('Origin',(-8.28877763349493,5.1250000427252,-0.349211602373583));
#58164=CARTESIAN_POINT('',(-8.28877763349493,5.1250000427252,-0.349211602373583));
#58165=CARTESIAN_POINT('',(-8.28877763349493,5.1250000427252,-0.349211602373583));
#58166=CARTESIAN_POINT('',(-8.28877763349493,5.1250000427252,-0.349211602373583));
#58167=CARTESIAN_POINT('Origin',(-8.28877763349493,-5.1249999572748,-0.349211602373583));
#58168=CARTESIAN_POINT('',(-8.28877763349493,-5.1249999572748,-0.349211602373583));
#58169=CARTESIAN_POINT('Origin',(-1.03877763349493,4.27252044680983E-8,
-0.349211602373583));
#58170=CARTESIAN_POINT('',(5.71122236650507,-4.6249999572748,-0.349211602373583));
#58171=CARTESIAN_POINT('',(5.71122236650507,4.6250000427252,-0.349211602373583));
#58172=CARTESIAN_POINT('',(5.71122236650507,-4.6249999572748,-0.349211602373583));
#58173=CARTESIAN_POINT('',(-7.78877763349493,-4.62499995727479,-0.349211602373583));
#58174=CARTESIAN_POINT('',(-7.78877763349493,-4.62499995727479,-0.349211602373583));
#58175=CARTESIAN_POINT('',(-7.78877763349493,4.6250000427252,-0.349211602373583));
#58176=CARTESIAN_POINT('',(-7.78877763349493,-4.62499995727479,-0.349211602373583));
#58177=CARTESIAN_POINT('',(-7.78877763349493,4.6250000427252,-0.349211602373583));
#58178=CARTESIAN_POINT('Origin',(6.08622236650508,-4.9999999572748,-6.09921160237358));
#58179=CARTESIAN_POINT('',(-1.53877763349493,-4.99999995727479,-1.59921160237358));
#58180=CARTESIAN_POINT('Origin',(-1.03877763349493,-4.99999995727479,-1.59921160237358));
#58181=CARTESIAN_POINT('Origin',(-1.03877763349493,-4.99999995727479,-1.59921160237358));
#58182=CARTESIAN_POINT('',(-7.96377763349493,-4.99999995727479,-4.84921160237358));
#58183=CARTESIAN_POINT('',(-7.96377763349493,-4.99999995727479,-6.09921160237359));
#58184=CARTESIAN_POINT('',(-8.2259070743313,-4.99999995727479,-1.65347979957788));
#58185=CARTESIAN_POINT('',(-8.2259070743313,-4.99999995727479,-1.65347979957788));
#58186=CARTESIAN_POINT('',(-7.96377763349493,-4.99999995727479,-1.09921160237358));
#58187=CARTESIAN_POINT('',(-8.4259070743313,-4.99999995727479,-1.65347979957787));
#58188=CARTESIAN_POINT('',(-8.4259070743313,-4.99999995727479,-1.65347979957787));
#58189=CARTESIAN_POINT('',(-8.16377763349493,-4.99999995727479,-4.84921160237358));
#58190=CARTESIAN_POINT('',(-8.16377763349493,-4.99999995727479,-4.84921160237358));
#58191=CARTESIAN_POINT('',(-8.16377763349493,-4.99999995727479,-6.09921160237358));
#58192=CARTESIAN_POINT('',(6.08622236650507,-4.99999995727479,-4.84921160237358));
#58193=CARTESIAN_POINT('',(6.08622236650508,-4.9999999572748,-6.09921160237358));
#58194=CARTESIAN_POINT('',(6.34835180734145,-4.99999995727479,-1.65347979957787));
#58195=CARTESIAN_POINT('',(6.08622236650507,-4.99999995727479,-4.84921160237358));
#58196=CARTESIAN_POINT('',(6.34835180734145,-4.99999995727479,-1.65347979957787));
#58197=CARTESIAN_POINT('',(6.14835180734145,-4.99999995727479,-1.65347979957788));
#58198=CARTESIAN_POINT('',(5.88622236650507,-4.99999995727479,-1.09921160237358));
#58199=CARTESIAN_POINT('',(5.88622236650507,-4.99999995727479,-4.84921160237358));
#58200=CARTESIAN_POINT('',(6.14835180734145,-4.99999995727479,-1.65347979957788));
#58201=CARTESIAN_POINT('',(5.88622236650507,-4.9999999572748,-6.09921160237358));
#58202=CARTESIAN_POINT('Origin',(-8.16377763349493,-4.99999995727479,-6.09921160237358));
#58203=CARTESIAN_POINT('',(-8.16377763349493,5.00000004272521,-4.84921160237358));
#58204=CARTESIAN_POINT('',(-8.16377763349493,5.12500004272521,-4.84921160237358));
#58205=CARTESIAN_POINT('',(-8.16377763349493,5.00000004272521,-6.09921160237358));
#58206=CARTESIAN_POINT('Origin',(-8.16377763349493,5.00000004272521,-6.09921160237358));
#58207=CARTESIAN_POINT('',(-1.53877763349493,5.00000004272521,-1.59921160237358));
#58208=CARTESIAN_POINT('Origin',(-1.03877763349493,5.00000004272521,-1.59921160237358));
#58209=CARTESIAN_POINT('Origin',(-1.03877763349493,5.00000004272521,-1.59921160237358));
#58210=CARTESIAN_POINT('',(5.88622236650507,5.00000004272521,-4.84921160237358));
#58211=CARTESIAN_POINT('',(5.88622236650507,5.00000004272521,-6.09921160237358));
#58212=CARTESIAN_POINT('',(6.14835180734144,5.00000004272521,-1.65347979957788));
#58213=CARTESIAN_POINT('',(6.14835180734144,5.00000004272521,-1.65347979957788));
#58214=CARTESIAN_POINT('',(5.88622236650507,5.00000004272521,-1.09921160237358));
#58215=CARTESIAN_POINT('',(6.34835180734145,5.00000004272521,-1.65347979957787));
#58216=CARTESIAN_POINT('',(6.34835180734145,5.00000004272521,-1.65347979957787));
#58217=CARTESIAN_POINT('',(6.08622236650507,5.00000004272521,-4.84921160237358));
#58218=CARTESIAN_POINT('',(6.08622236650507,5.00000004272521,-4.84921160237358));
#58219=CARTESIAN_POINT('',(6.08622236650508,5.00000004272521,-6.09921160237358));
#58220=CARTESIAN_POINT('',(-8.4259070743313,5.00000004272521,-1.65347979957787));
#58221=CARTESIAN_POINT('',(-8.16377763349493,5.00000004272521,-4.84921160237358));
#58222=CARTESIAN_POINT('',(-8.4259070743313,5.00000004272521,-1.65347979957787));
#58223=CARTESIAN_POINT('',(-8.2259070743313,5.00000004272521,-1.65347979957788));
#58224=CARTESIAN_POINT('',(-7.96377763349493,5.00000004272521,-1.09921160237358));
#58225=CARTESIAN_POINT('',(-7.96377763349493,5.00000004272521,-4.84921160237358));
#58226=CARTESIAN_POINT('',(-8.2259070743313,5.00000004272521,-1.65347979957788));
#58227=CARTESIAN_POINT('',(-7.96377763349493,5.00000004272521,-6.09921160237358));
#58228=CARTESIAN_POINT('Origin',(6.08622236650508,5.00000004272521,-6.09921160237358));
#58229=CARTESIAN_POINT('',(6.08622236650508,5.00000004272521,-4.84921160237358));
#58230=CARTESIAN_POINT('Origin',(-0.0387776334949297,-3.74999995727479,
-6.34921160237358));
#58231=CARTESIAN_POINT('',(-0.0387776334949297,-3.74999995727479,-6.34921160237358));
#58232=CARTESIAN_POINT('Origin',(-0.0387776334949297,-3.74999995727479,
-6.34921160237358));
#58233=CARTESIAN_POINT('',(-2.03877763349493,-3.74999995727479,-6.34921160237358));
#58234=CARTESIAN_POINT('',(-1.53877763349493,-3.74999995727479,-6.34921160237358));
#58235=CARTESIAN_POINT('',(-2.03877763349493,-3.74999995727479,-6.34921160237358));
#58236=CARTESIAN_POINT('Origin',(-0.0387776334949297,3.75000004272521,-6.34921160237358));
#58237=CARTESIAN_POINT('',(-2.03877763349493,3.75000004272521,-6.34921160237358));
#58238=CARTESIAN_POINT('',(-1.53877763349493,3.75000004272521,-6.34921160237358));
#58239=CARTESIAN_POINT('',(-2.03877763349493,3.75000004272521,-6.34921160237358));
#58240=CARTESIAN_POINT('Origin',(-1.03877763349493,4.27252044680983E-8,
-6.34921160237358));
#58241=CARTESIAN_POINT('',(-0.538777633494929,-0.999999957274796,-6.34921160237358));
#58242=CARTESIAN_POINT('',(-0.53877763349493,-3.74999995727479,-6.34921160237358));
#58243=CARTESIAN_POINT('',(-1.53877763349493,-0.999999957274796,-6.34921160237358));
#58244=CARTESIAN_POINT('',(-8.28877763349493,-0.999999957274793,-6.34921160237358));
#58245=CARTESIAN_POINT('',(-1.53877763349493,-3.74999995727479,-6.34921160237358));
#58246=CARTESIAN_POINT('',(-2.03877763349493,-3.74999995727479,-6.34921160237358));
#58247=CARTESIAN_POINT('',(-1.53877763349493,1.0000000427252,-6.34921160237358));
#58248=CARTESIAN_POINT('',(-1.53877763349493,-3.74999995727479,-6.34921160237358));
#58249=CARTESIAN_POINT('',(-0.538777633494928,1.00000004272521,-6.34921160237358));
#58250=CARTESIAN_POINT('',(-8.28877763349493,1.00000004272521,-6.34921160237358));
#58251=CARTESIAN_POINT('',(-0.53877763349493,-3.74999995727479,-6.34921160237358));
#58252=CARTESIAN_POINT('Origin',(-2.03877763349493,-3.74999995727479,-6.34921160237358));
#58253=CARTESIAN_POINT('Origin',(-5.03877763349493,-3.74999995727479,-6.34921160237358));
#58254=CARTESIAN_POINT('',(-5.03877763349493,-3.74999995727479,-6.34921160237358));
#58255=CARTESIAN_POINT('Origin',(-5.03877763349493,-3.74999995727479,-6.34921160237358));
#58256=CARTESIAN_POINT('',(-7.03877763349493,-3.74999995727479,-6.34921160237358));
#58257=CARTESIAN_POINT('',(-6.53877763349493,-3.74999995727479,-6.34921160237358));
#58258=CARTESIAN_POINT('',(-7.03877763349493,-3.74999995727479,-6.34921160237358));
#58259=CARTESIAN_POINT('Origin',(-5.03877763349493,3.75000004272521,-6.34921160237358));
#58260=CARTESIAN_POINT('',(-7.03877763349493,3.75000004272521,-6.34921160237358));
#58261=CARTESIAN_POINT('',(-6.53877763349493,3.75000004272521,-6.34921160237358));
#58262=CARTESIAN_POINT('',(-7.03877763349493,3.75000004272521,-6.34921160237358));
#58263=CARTESIAN_POINT('Origin',(-1.03877763349493,4.27252044680983E-8,
-6.34921160237358));
#58264=CARTESIAN_POINT('',(-5.53877763349493,-0.999999957274794,-6.34921160237358));
#58265=CARTESIAN_POINT('',(-5.53877763349493,-3.74999995727479,-6.34921160237358));
#58266=CARTESIAN_POINT('',(-6.53877763349493,-0.999999957274796,-6.34921160237358));
#58267=CARTESIAN_POINT('',(-8.28877763349493,-0.999999957274793,-6.34921160237358));
#58268=CARTESIAN_POINT('',(-6.53877763349493,-3.74999995727479,-6.34921160237358));
#58269=CARTESIAN_POINT('',(-7.03877763349493,-3.74999995727479,-6.34921160237358));
#58270=CARTESIAN_POINT('',(-6.53877763349493,1.00000004272521,-6.34921160237358));
#58271=CARTESIAN_POINT('',(-6.53877763349493,-3.74999995727479,-6.34921160237358));
#58272=CARTESIAN_POINT('',(-5.53877763349493,1.00000004272521,-6.34921160237358));
#58273=CARTESIAN_POINT('',(-8.28877763349493,1.00000004272521,-6.34921160237358));
#58274=CARTESIAN_POINT('',(-5.53877763349493,-3.74999995727479,-6.34921160237358));
#58275=CARTESIAN_POINT('Origin',(-7.03877763349493,-3.74999995727479,-6.34921160237358));
#58276=CARTESIAN_POINT('Origin',(-0.538777633494929,4.2725204287398E-8,
-13.0992116023736));
#58277=CARTESIAN_POINT('Origin',(-0.538777633494929,4.27252151294197E-8,
-6.34921160237358));
#58278=CARTESIAN_POINT('',(-0.538777633494927,-2.24999995727479,-13.0992116023736));
#58279=CARTESIAN_POINT('',(-0.538777633494929,-1.79999995727478,-13.9992116023736));
#58280=CARTESIAN_POINT('',(-0.538777633494928,2.25000004272521,-13.0992116023736));
#58281=CARTESIAN_POINT('',(-0.538777633494929,4.2725204287398E-8,-13.0992116023736));
#58282=CARTESIAN_POINT('',(-0.538777633494928,1.80000004272521,-13.9992116023736));
#58283=CARTESIAN_POINT('Origin',(-1.53877763349493,4.27252044897824E-8,
-13.0992116023736));
#58284=CARTESIAN_POINT('Origin',(-1.53877763349493,4.27252154908204E-8,
-6.34921160237358));
#58285=CARTESIAN_POINT('',(-1.53877763349493,2.25000004272521,-13.0992116023736));
#58286=CARTESIAN_POINT('',(-1.53877763349493,1.80000004272521,-13.9992116023736));
#58287=CARTESIAN_POINT('',(-1.53877763349493,-2.24999995727479,-13.0992116023736));
#58288=CARTESIAN_POINT('',(-1.53877763349493,4.27252044897824E-8,-13.0992116023736));
#58289=CARTESIAN_POINT('',(-1.53877763349493,-1.79999995727478,-13.9992116023736));
#58290=CARTESIAN_POINT('Origin',(-1.03877763349493,4.27252044680983E-8,
-13.0992116023736));
#58291=CARTESIAN_POINT('',(6.21122236650507,2.25000004272521,-13.0992116023736));
#58292=CARTESIAN_POINT('',(6.21122236650507,-2.24999995727479,-13.0992116023736));
#58293=CARTESIAN_POINT('Origin',(-5.53877763349493,4.27252060293495E-8,
-13.0992116023736));
#58294=CARTESIAN_POINT('Origin',(-5.53877763349493,4.27252169364233E-8,
-6.34921160237358));
#58295=CARTESIAN_POINT('',(-5.53877763349493,-2.24999995727479,-13.0992116023736));
#58296=CARTESIAN_POINT('',(-5.53877763349493,-1.79999995727478,-13.9992116023736));
#58297=CARTESIAN_POINT('',(-5.53877763349493,2.25000004272521,-13.0992116023736));
#58298=CARTESIAN_POINT('',(-5.53877763349493,4.27252060293495E-8,-13.0992116023736));
#58299=CARTESIAN_POINT('',(-5.53877763349493,1.80000004272521,-13.9992116023736));
#58300=CARTESIAN_POINT('Origin',(-6.53877763349493,4.27252044680983E-8,
-13.0992116023736));
#58301=CARTESIAN_POINT('Origin',(-6.53877763349493,4.2725217297824E-8,-6.34921160237358));
#58302=CARTESIAN_POINT('',(-6.53877763349493,2.25000004272521,-13.0992116023736));
#58303=CARTESIAN_POINT('',(-6.53877763349493,3.75000004272521,-10.0992116023736));
#58304=CARTESIAN_POINT('',(-6.53877763349493,-2.24999995727479,-13.0992116023736));
#58305=CARTESIAN_POINT('',(-6.53877763349493,4.27252044680983E-8,-13.0992116023736));
#58306=CARTESIAN_POINT('',(-6.53877763349493,-3.74999995727479,-10.0992116023736));
#58307=CARTESIAN_POINT('Origin',(-1.03877763349493,4.27252044680983E-8,
-13.0992116023736));
#58308=CARTESIAN_POINT('',(-1.03877763349493,2.25000004272521,-13.0992116023736));
#58309=CARTESIAN_POINT('',(-1.03877763349493,-2.24999995727479,-13.0992116023736));
#58310=CARTESIAN_POINT('Origin',(6.21122236650507,-3.74999995727479,-10.0992116023736));
#58311=CARTESIAN_POINT('Origin',(6.21122236650507,3.75000004272521,-10.0992116023736));
#58312=CARTESIAN_POINT('Origin',(6.21122236650507,-3.74999995727479,-10.0992116023736));
#58313=CARTESIAN_POINT('Origin',(6.21122236650507,3.75000004272521,-10.0992116023736));
#58314=CARTESIAN_POINT('Origin',(-8.28877763349493,4.27252179302753E-8,
-6.34921160237358));
#58315=CARTESIAN_POINT('Origin',(-8.28877763349493,4.27252179302753E-8,
-6.34921160237358));
#58316=CARTESIAN_POINT('Origin',(5.88622236650507,5.12500004272521,-4.84921160237358));
#58317=CARTESIAN_POINT('',(5.88622236650507,5.12500004272521,-4.84921160237358));
#58318=CARTESIAN_POINT('',(5.88622236650507,5.12500004272521,-1.09921160237358));
#58319=CARTESIAN_POINT('Origin',(-7.96377763349493,5.12500004272521,-4.84921160237358));
#58320=CARTESIAN_POINT('',(-7.96377763349493,5.12500004272521,-1.09921160237358));
#58321=CARTESIAN_POINT('',(-7.96377763349493,5.12500004272521,-4.84921160237358));
#58322=CARTESIAN_POINT('Origin',(-7.96377763349493,5.00000004272521,-1.09921160237358));
#58323=CARTESIAN_POINT('',(-8.2259070743313,5.00000004272521,-1.65347979957788));
#58324=CARTESIAN_POINT('Origin',(-8.2259070743313,5.00000004272521,-1.65347979957788));
#58325=CARTESIAN_POINT('Origin',(-8.16377763349493,5.00000004272521,-4.84921160237358));
#58326=CARTESIAN_POINT('',(-8.4259070743313,5.00000004272521,-1.65347979957787));
#58327=CARTESIAN_POINT('Origin',(-8.4259070743313,5.00000004272521,-1.65347979957787));
#58328=CARTESIAN_POINT('Origin',(6.34835180734145,5.00000004272521,-1.65347979957787));
#58329=CARTESIAN_POINT('',(6.34835180734145,5.00000004272521,-1.65347979957787));
#58330=CARTESIAN_POINT('Origin',(6.08622236650507,5.00000004272521,-4.84921160237358));
#58331=CARTESIAN_POINT('Origin',(6.14835180734144,5.00000004272521,-1.65347979957788));
#58332=CARTESIAN_POINT('',(6.14835180734144,5.00000004272521,-1.65347979957788));
#58333=CARTESIAN_POINT('Origin',(5.88622236650507,5.00000004272521,-1.09921160237358));
#58334=CARTESIAN_POINT('Origin',(-7.78877763349493,4.6250000427252,-0.0992116023735834));
#58335=CARTESIAN_POINT('',(-7.78877763349493,-4.6249999572748,-0.0992116023735834));
#58336=CARTESIAN_POINT('',(-7.78877763349493,4.6250000427252,-0.0992116023735834));
#58337=CARTESIAN_POINT('Origin',(-7.78877763349493,-4.6249999572748,-0.0992116023735834));
#58338=CARTESIAN_POINT('',(5.71122236650507,-4.6249999572748,-0.0992116023735834));
#58339=CARTESIAN_POINT('Origin',(5.71122236650507,4.6250000427252,-0.0992116023735834));
#58340=CARTESIAN_POINT('',(5.71122236650507,4.6250000427252,-0.0992116023735834));
#58341=CARTESIAN_POINT('Origin',(-7.78877763349493,4.6250000427252,-0.0992116023735834));
#58342=CARTESIAN_POINT('Origin',(-1.03877763349493,-4.99999995727479,-1.59921160237358));
#58343=CARTESIAN_POINT('',(-1.03877763349493,-5.4999999572748,-1.59921160237358));
#58344=CARTESIAN_POINT('Origin',(-1.03877763349493,-4.99999995727479,-1.59921160237358));
#58345=CARTESIAN_POINT('Origin',(-1.03877763349493,5.00000004272521,-1.59921160237358));
#58346=CARTESIAN_POINT('',(-1.03877763349493,5.50000004272521,-1.59921160237358));
#58347=CARTESIAN_POINT('Origin',(-1.03877763349493,5.00000004272521,-1.59921160237358));
#58348=CARTESIAN_POINT('',(0.,0.,0.));
#58349=CARTESIAN_POINT('Origin',(0.,92.5000000000001,-77.5000000000001));
#58350=CARTESIAN_POINT('',(-59.9898979485574,92.6000000000002,-77.5000000000001));
#58351=CARTESIAN_POINT('Origin',(0.,92.6000000000002,-77.5000000000001));
#58352=CARTESIAN_POINT('',(-59.5,93.,-77.5000000000001));
#58353=CARTESIAN_POINT('Origin',(-59.5,92.5000000000001,-77.5000000000001));
#58354=CARTESIAN_POINT('Origin',(0.,93.,-77.5000000000001));
#58355=CARTESIAN_POINT('Origin',(0.,93.,-77.5000000000001));
#58356=CARTESIAN_POINT('',(-60.7737346662472,92.76,-77.5000000000001));
#58357=CARTESIAN_POINT('Origin',(0.,92.76,-77.5000000000001));
#58358=CARTESIAN_POINT('',(-61.9494897427832,91.8000000000001,-77.5000000000001));
#58359=CARTESIAN_POINT('Origin',(-61.9494897427832,93.,-77.5000000000001));
#58360=CARTESIAN_POINT('Origin',(0.,91.8000000000001,-77.5000000000001));
#58361=CARTESIAN_POINT('Origin',(0.,92.5000000000001,-77.5000000000001));
#58362=CARTESIAN_POINT('',(-59.5,93.8,-77.5000000000001));
#58363=CARTESIAN_POINT('Origin',(0.,93.8,-77.5000000000001));
#58364=CARTESIAN_POINT('Origin',(-59.5,92.5000000000001,-77.5000000000001));
#58365=CARTESIAN_POINT('Origin',(0.,93.,-77.5000000000001));
#58366=CARTESIAN_POINT('',(-61.9494897427832,91.0000000000001,-77.5000000000001));
#58367=CARTESIAN_POINT('Origin',(0.,91.0000000000001,-77.5000000000001));
#58368=CARTESIAN_POINT('Origin',(-61.9494897427832,93.,-77.5000000000001));
#58369=CARTESIAN_POINT('Origin',(80.,91.0000000000001,-155.));
#58370=CARTESIAN_POINT('',(-77.6424777960769,91.0000000000001,-57.5));
#58371=CARTESIAN_POINT('',(-79.2,91.,-57.5));
#58372=CARTESIAN_POINT('',(80.,91.0000000000001,-57.5));
#58373=CARTESIAN_POINT('',(-77.6424777960769,91.0000000000001,-97.5));
#58374=CARTESIAN_POINT('',(-77.6424777960769,91.0000000000001,-155.));
#58375=CARTESIAN_POINT('',(-79.2,91.0000000000001,-97.5));
#58376=CARTESIAN_POINT('',(80.,91.0000000000001,-97.5));
#58377=CARTESIAN_POINT('',(-79.2,91.0000000000001,-155.));
#58378=CARTESIAN_POINT('',(-79.2,91.0000000000001,-155.));
#58379=CARTESIAN_POINT('',(79.2,91.0000000000001,-155.));
#58380=CARTESIAN_POINT('',(80.,91.0000000000001,-155.));
#58381=CARTESIAN_POINT('',(79.2,91.0000000000001,-97.5000000000001));
#58382=CARTESIAN_POINT('',(79.2,91.0000000000001,-155.));
#58383=CARTESIAN_POINT('',(77.642477796077,91.0000000000001,-97.5000000000001));
#58384=CARTESIAN_POINT('',(80.,91.0000000000001,-97.5000000000001));
#58385=CARTESIAN_POINT('',(77.642477796077,91.0000000000001,-57.5000000000001));
#58386=CARTESIAN_POINT('',(77.6424777960769,91.0000000000001,-155.));
#58387=CARTESIAN_POINT('',(79.2,91.0000000000001,-57.5000000000001));
#58388=CARTESIAN_POINT('',(80.,91.0000000000001,-57.5000000000001));
#58389=CARTESIAN_POINT('',(79.2,91.0000000000001,0.));
#58390=CARTESIAN_POINT('',(79.2,91.0000000000001,-155.));
#58391=CARTESIAN_POINT('',(-79.2,91.0000000000001,0.));
#58392=CARTESIAN_POINT('',(80.,91.0000000000001,0.));
#58393=CARTESIAN_POINT('',(-79.2,91.0000000000001,-155.));
#58394=CARTESIAN_POINT('Origin',(80.,91.8000000000001,-155.));
#58395=CARTESIAN_POINT('',(-77.6424777960769,91.8000000000001,-57.5));
#58396=CARTESIAN_POINT('',(-77.6424777960769,91.8000000000001,-97.5));
#58397=CARTESIAN_POINT('',(-77.6424777960769,91.8000000000001,-57.5));
#58398=CARTESIAN_POINT('',(-79.2,91.8000000000001,-57.5));
#58399=CARTESIAN_POINT('',(-82.6424777960769,91.8000000000001,-57.5));
#58400=CARTESIAN_POINT('',(-79.2,91.8000000000001,0.));
#58401=CARTESIAN_POINT('',(-79.2,91.8000000000001,-155.));
#58402=CARTESIAN_POINT('',(79.2,91.8000000000001,0.));
#58403=CARTESIAN_POINT('',(80.,91.8000000000001,0.));
#58404=CARTESIAN_POINT('',(79.2,91.8000000000001,-57.5000000000001));
#58405=CARTESIAN_POINT('',(79.2,91.8000000000001,-155.));
#58406=CARTESIAN_POINT('',(77.642477796077,91.8000000000001,-57.5000000000001));
#58407=CARTESIAN_POINT('',(82.642477796077,91.8000000000001,-57.5000000000001));
#58408=CARTESIAN_POINT('',(77.642477796077,91.8000000000001,-97.5000000000001));
#58409=CARTESIAN_POINT('',(77.642477796077,91.8000000000001,-57.5000000000001));
#58410=CARTESIAN_POINT('',(79.2,91.8000000000001,-97.5000000000001));
#58411=CARTESIAN_POINT('',(82.642477796077,91.8000000000001,-97.5000000000001));
#58412=CARTESIAN_POINT('',(79.2,91.8000000000001,-155.));
#58413=CARTESIAN_POINT('',(79.2,91.8000000000001,-155.));
#58414=CARTESIAN_POINT('',(-79.2,91.8000000000001,-155.));
#58415=CARTESIAN_POINT('',(80.,91.8000000000001,-155.));
#58416=CARTESIAN_POINT('',(-79.2,91.8000000000001,-97.5));
#58417=CARTESIAN_POINT('',(-79.2,91.8000000000001,-155.));
#58418=CARTESIAN_POINT('',(-82.6424777960769,91.8000000000001,-97.5));
#58419=CARTESIAN_POINT('Origin',(80.8,90.2,0.));
#58420=CARTESIAN_POINT('',(79.2,91.0000000000001,0.));
#58421=CARTESIAN_POINT('',(-79.2,91.8000000000001,0.));
#58422=CARTESIAN_POINT('Origin',(-80.8,90.2,-155.));
#58423=CARTESIAN_POINT('',(-79.2,91.0000000000001,-155.));
#58424=CARTESIAN_POINT('',(79.2,91.8000000000001,-155.));
#58425=CARTESIAN_POINT('Origin',(-82.6424777960769,81.8000000000001,-57.5));
#58426=CARTESIAN_POINT('',(-79.2,91.8000000000001,-57.5));
#58427=CARTESIAN_POINT('',(-77.6424777960769,81.8000000000001,-57.5));
#58428=CARTESIAN_POINT('Origin',(-82.6424777960769,81.8000000000001,-97.5));
#58429=CARTESIAN_POINT('',(-79.2,91.0000000000001,-97.5));
#58430=CARTESIAN_POINT('',(-77.6424777960769,81.8000000000001,-97.5));
#58431=CARTESIAN_POINT('Origin',(-77.6424777960769,81.8000000000001,-57.5));
#58432=CARTESIAN_POINT('Origin',(82.642477796077,81.8000000000001,-57.5000000000001));
#58433=CARTESIAN_POINT('',(79.2,91.0000000000001,-57.5000000000001));
#58434=CARTESIAN_POINT('',(77.642477796077,81.8000000000001,-57.5000000000001));
#58435=CARTESIAN_POINT('Origin',(77.642477796077,81.8000000000001,-57.5000000000001));
#58436=CARTESIAN_POINT('',(77.642477796077,81.8000000000001,-97.5000000000001));
#58437=CARTESIAN_POINT('Origin',(82.642477796077,81.8000000000001,-97.5000000000001));
#58438=CARTESIAN_POINT('',(79.2,91.8000000000001,-97.5000000000001));
#58439=CARTESIAN_POINT('Origin',(79.2,90.2,-57.5000000000001));
#58440=CARTESIAN_POINT('',(80.8,90.2,-57.5000000000001));
#58441=CARTESIAN_POINT('',(80.0000000000001,90.2,-57.5000000000001));
#58442=CARTESIAN_POINT('',(80.8,90.2,-57.5000000000001));
#58443=CARTESIAN_POINT('Origin',(79.2,90.2,-57.5000000000001));
#58444=CARTESIAN_POINT('Origin',(79.2,90.2,-57.5000000000001));
#58445=CARTESIAN_POINT('Origin',(79.2,90.2,0.));
#58446=CARTESIAN_POINT('',(80.0000000000001,90.2,0.));
#58447=CARTESIAN_POINT('Origin',(79.2,90.2,0.));
#58448=CARTESIAN_POINT('',(80.8000000000001,90.2,0.));
#58449=CARTESIAN_POINT('',(80.8000000000001,90.2,0.));
#58450=CARTESIAN_POINT('Origin',(79.2,90.2,0.));
#58451=CARTESIAN_POINT('Origin',(79.2,90.2,28.7864498173497));
#58452=CARTESIAN_POINT('',(80.8000000000001,90.2,-155.));
#58453=CARTESIAN_POINT('Origin',(79.2,90.2,28.7864498173497));
#58454=CARTESIAN_POINT('',(80.0000000000001,90.2,-155.));
#58455=CARTESIAN_POINT('Origin',(79.2,90.2,-97.5000000000001));
#58456=CARTESIAN_POINT('',(80.0000000000001,90.2,-97.5000000000001));
#58457=CARTESIAN_POINT('Origin',(79.2,90.2,-97.5000000000001));
#58458=CARTESIAN_POINT('',(80.8,90.2,-97.5000000000001));
#58459=CARTESIAN_POINT('',(80.0000000000001,90.2,-97.5000000000001));
#58460=CARTESIAN_POINT('Origin',(79.2,90.2,-97.5000000000001));
#58461=CARTESIAN_POINT('Origin',(79.2,90.2,-155.));
#58462=CARTESIAN_POINT('',(80.0000000000001,90.2,-155.));
#58463=CARTESIAN_POINT('',(80.8,90.2,-155.));
#58464=CARTESIAN_POINT('',(80.0000000000001,90.2,-155.));
#58465=CARTESIAN_POINT('Origin',(79.2,90.2,-155.));
#58466=CARTESIAN_POINT('Origin',(79.2,90.2,-155.));
#58467=CARTESIAN_POINT('Origin',(79.2,90.2,-68.7135501826506));
#58468=CARTESIAN_POINT('',(80.8000000000001,90.2,-155.));
#58469=CARTESIAN_POINT('Origin',(79.2,90.2,-68.7135501826506));
#58470=CARTESIAN_POINT('',(80.0000000000001,90.2,-155.));
#58471=CARTESIAN_POINT('Origin',(80.8000000000001,3.1575222039231,-5.));
#58472=CARTESIAN_POINT('',(80.8000000000001,3.1575222039231,0.));
#58473=CARTESIAN_POINT('',(80.8000000000001,-1.84247779607691,-5.));
#58474=CARTESIAN_POINT('Origin',(80.8000000000001,3.1575222039231,-5.));
#58475=CARTESIAN_POINT('',(80.0000000000001,3.1575222039231,0.));
#58476=CARTESIAN_POINT('',(80.8000000000001,3.1575222039231,0.));
#58477=CARTESIAN_POINT('',(80.0000000000001,-1.84247779607691,-5.));
#58478=CARTESIAN_POINT('Origin',(80.0000000000001,3.1575222039231,-5.));
#58479=CARTESIAN_POINT('',(80.0000000000001,-1.84247779607691,-5.));
#58480=CARTESIAN_POINT('Origin',(70.8,88.6424777960769,-57.5000000000001));
#58481=CARTESIAN_POINT('',(80.0000000000001,88.642477796077,-97.5000000000001));
#58482=CARTESIAN_POINT('',(80.0000000000001,88.6424777960769,-57.5000000000001));
#58483=CARTESIAN_POINT('',(80.0000000000001,88.6424777960771,-155.));
#58484=CARTESIAN_POINT('',(80.8000000000001,88.6424777960769,-57.5000000000001));
#58485=CARTESIAN_POINT('',(70.8,88.6424777960769,-57.5000000000001));
#58486=CARTESIAN_POINT('',(80.8,88.642477796077,-97.5000000000001));
#58487=CARTESIAN_POINT('',(80.8,88.6424777960769,-57.5000000000001));
#58488=CARTESIAN_POINT('',(70.8,88.642477796077,-97.5000000000001));
#58489=CARTESIAN_POINT('Origin',(79.2000000000001,3.1575222039231,-150.));
#58490=CARTESIAN_POINT('',(80.8000000000001,-1.84247779607691,-150.));
#58491=CARTESIAN_POINT('',(80.8000000000001,3.1575222039231,-155.));
#58492=CARTESIAN_POINT('Origin',(80.8000000000001,3.1575222039231,-150.));
#58493=CARTESIAN_POINT('',(80.0000000000001,-1.84247779607691,-150.));
#58494=CARTESIAN_POINT('',(80.8000000000001,-1.84247779607691,-150.));
#58495=CARTESIAN_POINT('',(80.0000000000001,3.1575222039231,-155.));
#58496=CARTESIAN_POINT('Origin',(80.0000000000001,3.1575222039231,-150.));
#58497=CARTESIAN_POINT('',(80.0000000000001,3.1575222039231,-155.));
#58498=CARTESIAN_POINT('Origin',(80.8000000000001,-1.84247779607691,-155.));
#58499=CARTESIAN_POINT('',(80.0000000000001,-1.84247779607691,-155.));
#58500=CARTESIAN_POINT('',(80.8000000000001,-1.84247779607691,-155.));
#58501=CARTESIAN_POINT('Origin',(80.8000000000001,-1.84247779607691,-155.));
#58502=CARTESIAN_POINT('',(80.8000000000001,-1.84247779607691,-155.));
#58503=CARTESIAN_POINT('',(80.8,88.642477796077,-97.5000000000001));
#58504=CARTESIAN_POINT('',(80.8,88.6424777960769,-57.5000000000001));
#58505=CARTESIAN_POINT('',(80.8000000000001,-1.84247779607691,0.));
#58506=CARTESIAN_POINT('Origin',(70.8,88.642477796077,-97.5000000000001));
#58507=CARTESIAN_POINT('',(80.0000000000001,-1.84247779607691,-97.5000000000001));
#58508=CARTESIAN_POINT('Origin',(80.0000000000001,-1.84247779607691,-155.));
#58509=CARTESIAN_POINT('',(80.0000000000001,-1.84247779607691,-155.));
#58510=CARTESIAN_POINT('',(80.0000000000001,-1.84247779607691,0.));
#58511=CARTESIAN_POINT('',(80.0000000000001,-1.84247779607691,-57.5000000000001));
#58512=CARTESIAN_POINT('Origin',(79.2000000000001,91.8000000000001,-155.));
#58513=CARTESIAN_POINT('Origin',(79.2000000000001,90.2,0.));
#58514=CARTESIAN_POINT('Origin',(70.8,88.6424777960769,-57.5000000000001));
#58515=CARTESIAN_POINT('Origin',(-79.2,90.2,-97.5));
#58516=CARTESIAN_POINT('',(-80.8,90.2000000000001,-97.5));
#58517=CARTESIAN_POINT('',(-80.,90.2,-97.5));
#58518=CARTESIAN_POINT('',(-80.8,90.2,-97.5));
#58519=CARTESIAN_POINT('Origin',(-79.2,90.2,-97.5));
#58520=CARTESIAN_POINT('Origin',(-79.2,90.2,-97.5));
#58521=CARTESIAN_POINT('Origin',(-79.2,90.2,-155.));
#58522=CARTESIAN_POINT('',(-80.,90.2,-155.));
#58523=CARTESIAN_POINT('Origin',(-79.2,90.2,-155.));
#58524=CARTESIAN_POINT('',(-80.8,90.2,-155.));
#58525=CARTESIAN_POINT('',(-80.8,90.2,-155.));
#58526=CARTESIAN_POINT('Origin',(-79.2,90.2,-155.));
#58527=CARTESIAN_POINT('Origin',(-79.2,90.2,-183.78644981735));
#58528=CARTESIAN_POINT('',(-80.8,90.2,-155.));
#58529=CARTESIAN_POINT('Origin',(-79.2,90.2,-183.78644981735));
#58530=CARTESIAN_POINT('',(-80.,90.2,-155.));
#58531=CARTESIAN_POINT('Origin',(-79.2,90.2,-57.5));
#58532=CARTESIAN_POINT('',(-80.,90.2,-57.5));
#58533=CARTESIAN_POINT('Origin',(-79.2,90.2,-57.5));
#58534=CARTESIAN_POINT('',(-80.8,90.2,-57.5));
#58535=CARTESIAN_POINT('',(-80.,90.2,-57.5));
#58536=CARTESIAN_POINT('Origin',(-79.2,90.2,-57.5));
#58537=CARTESIAN_POINT('Origin',(-79.2,90.2,0.));
#58538=CARTESIAN_POINT('',(-80.,90.2,0.));
#58539=CARTESIAN_POINT('',(-80.8,90.2000000000001,0.));
#58540=CARTESIAN_POINT('',(-80.,90.2,0.));
#58541=CARTESIAN_POINT('Origin',(-79.2,90.2,0.));
#58542=CARTESIAN_POINT('Origin',(-79.2,90.2,0.));
#58543=CARTESIAN_POINT('Origin',(-79.2,90.2,-86.2864498173496));
#58544=CARTESIAN_POINT('',(-80.8,90.2,-155.));
#58545=CARTESIAN_POINT('Origin',(-79.2,90.2,-86.2864498173496));
#58546=CARTESIAN_POINT('',(-80.,90.2,-155.));
#58547=CARTESIAN_POINT('Origin',(79.2,3.15752220392312,-150.));
#58548=CARTESIAN_POINT('',(-80.,-1.84247779607691,-150.));
#58549=CARTESIAN_POINT('',(-80.,3.15752220392312,-155.));
#58550=CARTESIAN_POINT('Origin',(-80.,3.15752220392312,-150.));
#58551=CARTESIAN_POINT('',(-80.8,-1.84247779607691,-150.));
#58552=CARTESIAN_POINT('',(-80.,-1.84247779607691,-150.));
#58553=CARTESIAN_POINT('',(-80.8,3.15752220392312,-155.));
#58554=CARTESIAN_POINT('Origin',(-80.8,3.15752220392312,-150.));
#58555=CARTESIAN_POINT('',(79.2,3.15752220392312,-155.));
#58556=CARTESIAN_POINT('Origin',(-70.8,88.642477796077,-57.5));
#58557=CARTESIAN_POINT('',(-80.,88.642477796077,-97.5));
#58558=CARTESIAN_POINT('',(-80.8,88.642477796077,-97.5));
#58559=CARTESIAN_POINT('',(-70.8,88.642477796077,-97.5));
#58560=CARTESIAN_POINT('',(-80.8,88.642477796077,-57.5));
#58561=CARTESIAN_POINT('',(-80.8,88.642477796077,-57.5));
#58562=CARTESIAN_POINT('',(-80.,88.642477796077,-57.5));
#58563=CARTESIAN_POINT('',(-70.8,88.642477796077,-57.5));
#58564=CARTESIAN_POINT('',(-80.,88.642477796077,-155.));
#58565=CARTESIAN_POINT('Origin',(-80.,3.1575222039231,-5.));
#58566=CARTESIAN_POINT('',(-80.,3.1575222039231,0.));
#58567=CARTESIAN_POINT('',(-80.,-1.84247779607691,-5.));
#58568=CARTESIAN_POINT('Origin',(-80.,3.1575222039231,-5.));
#58569=CARTESIAN_POINT('',(-80.8,3.1575222039231,0.));
#58570=CARTESIAN_POINT('',(-80.,3.1575222039231,0.));
#58571=CARTESIAN_POINT('',(-80.8,-1.84247779607691,-5.));
#58572=CARTESIAN_POINT('Origin',(-80.8,3.1575222039231,-5.));
#58573=CARTESIAN_POINT('',(-80.8,-1.84247779607691,-5.));
#58574=CARTESIAN_POINT('Origin',(-80.,-1.84247779607691,-155.));
#58575=CARTESIAN_POINT('',(-80.,-1.84247779607691,-155.));
#58576=CARTESIAN_POINT('',(-80.8,-1.84247779607691,-155.));
#58577=CARTESIAN_POINT('Origin',(-80.8,-1.84247779607691,-155.));
#58578=CARTESIAN_POINT('',(-80.8,-1.84247779607691,0.));
#58579=CARTESIAN_POINT('',(-80.8,88.642477796077,-57.5));
#58580=CARTESIAN_POINT('',(-80.8,88.642477796077,-97.5));
#58581=CARTESIAN_POINT('',(-80.8,-1.84247779607691,-155.));
#58582=CARTESIAN_POINT('Origin',(-70.8,88.642477796077,-57.5));
#58583=CARTESIAN_POINT('',(-80.,-1.84247779607691,-57.5));
#58584=CARTESIAN_POINT('Origin',(-80.,-1.84247779607691,-155.));
#58585=CARTESIAN_POINT('',(-80.,-1.84247779607691,0.));
#58586=CARTESIAN_POINT('',(-80.,-1.84247779607691,-155.));
#58587=CARTESIAN_POINT('',(-80.,-1.84247779607691,-97.5));
#58588=CARTESIAN_POINT('Origin',(-79.2,91.8000000000001,0.));
#58589=CARTESIAN_POINT('Origin',(79.2,90.2,-155.));
#58590=CARTESIAN_POINT('Origin',(-70.8,88.642477796077,-97.5));
#58591=CARTESIAN_POINT('Origin',(0.,93.8,-77.5000000000001));
#58592=CARTESIAN_POINT('',(-21.8868869275414,93.8,-69.9335415751337));
#58593=CARTESIAN_POINT('',(-21.4537521251327,93.8,-72.7876136793868));
#58594=CARTESIAN_POINT('',(-21.8868869275414,93.8,-69.9335415751337));
#58595=CARTESIAN_POINT('',(-24.5751532752614,93.8,-68.8816112651563));
#58596=CARTESIAN_POINT('',(-24.5751532752614,93.8,-68.8816112651563));
#58597=CARTESIAN_POINT('',(-26.8302848205727,93.8,-70.683753059432));
#58598=CARTESIAN_POINT('',(-26.8302848205727,93.8,-70.683753059432));
#58599=CARTESIAN_POINT('',(-26.397150018164,93.8,-73.537825163685));
#58600=CARTESIAN_POINT('',(-26.397150018164,93.8,-73.537825163685));
#58601=CARTESIAN_POINT('',(-23.708883670444,93.8,-74.5897554736624));
#58602=CARTESIAN_POINT('',(-23.708883670444,93.8,-74.5897554736624));
#58603=CARTESIAN_POINT('',(-21.4537521251327,93.8,-72.7876136793868));
#58604=CARTESIAN_POINT('',(-14.9025660797482,93.8,-72.6665366894876));
#58605=CARTESIAN_POINT('',(-14.4694312773395,93.8,-75.5206087937407));
#58606=CARTESIAN_POINT('',(-14.9025660797482,93.8,-72.6665366894876));
#58607=CARTESIAN_POINT('',(-17.5908324274683,93.8,-71.6146063795101));
#58608=CARTESIAN_POINT('',(-17.5908324274683,93.8,-71.6146063795101));
#58609=CARTESIAN_POINT('',(-19.8459639727796,93.8,-73.4167481737858));
#58610=CARTESIAN_POINT('',(-19.8459639727796,93.8,-73.4167481737858));
#58611=CARTESIAN_POINT('',(-19.4128291703709,93.8,-76.2708202780389));
#58612=CARTESIAN_POINT('',(-19.4128291703709,93.8,-76.2708202780389));
#58613=CARTESIAN_POINT('',(-16.7245628226509,93.8,-77.3227505880163));
#58614=CARTESIAN_POINT('',(-16.7245628226509,93.8,-77.3227505880163));
#58615=CARTESIAN_POINT('',(-14.4694312773395,93.8,-75.5206087937407));
#58616=CARTESIAN_POINT('',(-7.91824523195512,93.8,-75.3995318038414));
#58617=CARTESIAN_POINT('',(-7.4851104295464,93.8,-78.2536039080945));
#58618=CARTESIAN_POINT('',(-7.91824523195512,93.8,-75.3995318038414));
#58619=CARTESIAN_POINT('',(-10.6065115796751,93.8,-74.347601493864));
#58620=CARTESIAN_POINT('',(-10.6065115796751,93.8,-74.347601493864));
#58621=CARTESIAN_POINT('',(-12.8616431249865,93.8,-76.1497432881397));
#58622=CARTESIAN_POINT('',(-12.8616431249865,93.8,-76.1497432881397));
#58623=CARTESIAN_POINT('',(-12.4285083225778,93.8,-79.0038153923928));
#58624=CARTESIAN_POINT('',(-12.4285083225778,93.8,-79.0038153923928));
#58625=CARTESIAN_POINT('',(-9.74024197485773,93.8,-80.0557457023702));
#58626=CARTESIAN_POINT('',(-9.74024197485773,93.8,-80.0557457023702));
#58627=CARTESIAN_POINT('',(-7.4851104295464,93.8,-78.2536039080945));
#58628=CARTESIAN_POINT('',(-0.933924384161986,93.8,-78.1325269181953));
#58629=CARTESIAN_POINT('',(-0.500789581753268,93.8,-80.9865990224485));
#58630=CARTESIAN_POINT('',(-0.933924384161986,93.8,-78.1325269181953));
#58631=CARTESIAN_POINT('',(-3.622190731882,93.8,-77.0805966082179));
#58632=CARTESIAN_POINT('',(-3.622190731882,93.8,-77.0805966082179));
#58633=CARTESIAN_POINT('',(-5.87732227719335,93.8,-78.8827384024936));
#58634=CARTESIAN_POINT('',(-5.87732227719335,93.8,-78.8827384024936));
#58635=CARTESIAN_POINT('',(-5.44418747478462,93.8,-81.7368105067467));
#58636=CARTESIAN_POINT('',(-5.44418747478462,93.8,-81.7368105067467));
#58637=CARTESIAN_POINT('',(-2.75592112706459,93.8,-82.7887408167241));
#58638=CARTESIAN_POINT('',(-2.75592112706459,93.8,-82.7887408167241));
#58639=CARTESIAN_POINT('',(-0.500789581753269,93.8,-80.9865990224485));
#58640=CARTESIAN_POINT('',(6.05039646363115,93.8,-80.8655220325492));
#58641=CARTESIAN_POINT('',(6.48353126603986,93.8,-83.7195941368023));
#58642=CARTESIAN_POINT('',(6.05039646363115,93.8,-80.8655220325492));
#58643=CARTESIAN_POINT('',(3.36213011591114,93.8,-79.8135917225718));
#58644=CARTESIAN_POINT('',(3.36213011591114,93.8,-79.8135917225718));
#58645=CARTESIAN_POINT('',(1.10699857059978,93.8,-81.6157335168475));
#58646=CARTESIAN_POINT('',(1.10699857059978,93.8,-81.6157335168475));
#58647=CARTESIAN_POINT('',(1.54013337300851,93.8,-84.4698056211006));
#58648=CARTESIAN_POINT('',(1.54013337300851,93.8,-84.4698056211006));
#58649=CARTESIAN_POINT('',(4.22839972072854,93.8,-85.521735931078));
#58650=CARTESIAN_POINT('',(4.22839972072854,93.8,-85.521735931078));
#58651=CARTESIAN_POINT('',(6.48353126603986,93.8,-83.7195941368023));
#58652=CARTESIAN_POINT('',(13.0347173114243,93.8,-83.5985171469031));
#58653=CARTESIAN_POINT('',(13.467852113833,93.8,-86.4525892511562));
#58654=CARTESIAN_POINT('',(13.0347173114243,93.8,-83.5985171469031));
#58655=CARTESIAN_POINT('',(10.3464509637043,93.8,-82.5465868369257));
#58656=CARTESIAN_POINT('',(10.3464509637043,93.8,-82.5465868369257));
#58657=CARTESIAN_POINT('',(8.09131941839291,93.8,-84.3487286312014));
#58658=CARTESIAN_POINT('',(8.09131941839291,93.8,-84.3487286312014));
#58659=CARTESIAN_POINT('',(8.52445422080164,93.8,-87.2028007354545));
#58660=CARTESIAN_POINT('',(8.52445422080164,93.8,-87.2028007354545));
#58661=CARTESIAN_POINT('',(11.2127205685217,93.8,-88.2547310454319));
#58662=CARTESIAN_POINT('',(11.2127205685217,93.8,-88.2547310454319));
#58663=CARTESIAN_POINT('',(13.467852113833,93.8,-86.4525892511562));
#58664=CARTESIAN_POINT('',(20.0190381592174,93.8,-86.331512261257));
#58665=CARTESIAN_POINT('',(20.4521729616261,93.8,-89.1855843655101));
#58666=CARTESIAN_POINT('',(20.0190381592174,93.8,-86.331512261257));
#58667=CARTESIAN_POINT('',(17.3307718114974,93.8,-85.2795819512796));
#58668=CARTESIAN_POINT('',(17.3307718114974,93.8,-85.2795819512796));
#58669=CARTESIAN_POINT('',(15.075640266186,93.8,-87.0817237455553));
#58670=CARTESIAN_POINT('',(15.075640266186,93.8,-87.0817237455553));
#58671=CARTESIAN_POINT('',(15.5087750685948,93.8,-89.9357958498083));
#58672=CARTESIAN_POINT('',(15.5087750685948,93.8,-89.9357958498083));
#58673=CARTESIAN_POINT('',(18.1970414163148,93.8,-90.9877261597858));
#58674=CARTESIAN_POINT('',(18.1970414163148,93.8,-90.9877261597858));
#58675=CARTESIAN_POINT('',(20.4521729616261,93.8,-89.1855843655101));
#58676=CARTESIAN_POINT('',(27.0033590070105,93.8,-89.0645073756109));
#58677=CARTESIAN_POINT('',(27.4364938094193,93.8,-91.918579479864));
#58678=CARTESIAN_POINT('',(27.0033590070105,93.8,-89.0645073756109));
#58679=CARTESIAN_POINT('',(24.3150926592905,93.8,-88.0125770656335));
#58680=CARTESIAN_POINT('',(24.3150926592905,93.8,-88.0125770656335));
#58681=CARTESIAN_POINT('',(22.0599611139792,93.8,-89.8147188599092));
#58682=CARTESIAN_POINT('',(22.0599611139792,93.8,-89.8147188599092));
#58683=CARTESIAN_POINT('',(22.4930959163879,93.8,-92.6687909641622));
#58684=CARTESIAN_POINT('',(22.4930959163879,93.8,-92.6687909641622));
#58685=CARTESIAN_POINT('',(25.1813622641079,93.8,-93.7207212741397));
#58686=CARTESIAN_POINT('',(25.1813622641079,93.8,-93.7207212741397));
#58687=CARTESIAN_POINT('',(27.4364938094193,93.8,-91.918579479864));
#58688=CARTESIAN_POINT('',(-16.0278833061956,93.8,-65.2514398499405));
#58689=CARTESIAN_POINT('',(-15.5947485037869,93.8,-68.1055119541936));
#58690=CARTESIAN_POINT('',(-16.0278833061956,93.8,-65.2514398499405));
#58691=CARTESIAN_POINT('',(-18.7161496539156,93.8,-64.1995095399631));
#58692=CARTESIAN_POINT('',(-18.7161496539156,93.8,-64.1995095399631));
#58693=CARTESIAN_POINT('',(-20.971281199227,93.8,-66.0016513342388));
#58694=CARTESIAN_POINT('',(-20.971281199227,93.8,-66.0016513342388));
#58695=CARTESIAN_POINT('',(-20.5381463968183,93.8,-68.8557234384919));
#58696=CARTESIAN_POINT('',(-20.5381463968183,93.8,-68.8557234384919));
#58697=CARTESIAN_POINT('',(-17.8498800490982,93.8,-69.9076537484693));
#58698=CARTESIAN_POINT('',(-17.8498800490982,93.8,-69.9076537484693));
#58699=CARTESIAN_POINT('',(-15.5947485037869,93.8,-68.1055119541936));
#58700=CARTESIAN_POINT('',(-23.0122041539888,93.8,-62.5184447355866));
#58701=CARTESIAN_POINT('',(-22.57906935158,93.8,-65.3725168398397));
#58702=CARTESIAN_POINT('',(-23.0122041539888,93.8,-62.5184447355866));
#58703=CARTESIAN_POINT('',(-25.7004705017088,93.8,-61.4665144256092));
#58704=CARTESIAN_POINT('',(-25.7004705017088,93.8,-61.4665144256092));
#58705=CARTESIAN_POINT('',(-27.9556020470201,93.8,-63.2686562198849));
#58706=CARTESIAN_POINT('',(-27.9556020470201,93.8,-63.2686562198849));
#58707=CARTESIAN_POINT('',(-27.5224672446114,93.8,-66.122728324138));
#58708=CARTESIAN_POINT('',(-27.5224672446114,93.8,-66.122728324138));
#58709=CARTESIAN_POINT('',(-24.8342008968914,93.8,-67.1746586341154));
#58710=CARTESIAN_POINT('',(-24.8342008968914,93.8,-67.1746586341154));
#58711=CARTESIAN_POINT('',(-22.57906935158,93.8,-65.3725168398397));
#58712=CARTESIAN_POINT('',(-29.9965250017819,93.8,-59.7854496212327));
#58713=CARTESIAN_POINT('',(-29.5633901993732,93.8,-62.6395217254858));
#58714=CARTESIAN_POINT('',(-29.9965250017819,93.8,-59.7854496212327));
#58715=CARTESIAN_POINT('',(-32.6847913495019,93.8,-58.7335193112553));
#58716=CARTESIAN_POINT('',(-32.6847913495019,93.8,-58.7335193112553));
#58717=CARTESIAN_POINT('',(-34.9399228948133,93.8,-60.535661105531));
#58718=CARTESIAN_POINT('',(-34.9399228948133,93.8,-60.535661105531));
#58719=CARTESIAN_POINT('',(-34.5067880924045,93.8,-63.3897332097841));
#58720=CARTESIAN_POINT('',(-34.5067880924045,93.8,-63.3897332097841));
#58721=CARTESIAN_POINT('',(-31.8185217446845,93.8,-64.4416635197615));
#58722=CARTESIAN_POINT('',(-31.8185217446845,93.8,-64.4416635197615));
#58723=CARTESIAN_POINT('',(-29.5633901993732,93.8,-62.6395217254858));
#58724=CARTESIAN_POINT('',(-36.980845849575,93.8,-57.0524545068788));
#58725=CARTESIAN_POINT('',(-36.5477110471663,93.8,-59.9065266111319));
#58726=CARTESIAN_POINT('',(-36.980845849575,93.8,-57.0524545068788));
#58727=CARTESIAN_POINT('',(-39.669112197295,93.8,-56.0005241969014));
#58728=CARTESIAN_POINT('',(-39.669112197295,93.8,-56.0005241969014));
#58729=CARTESIAN_POINT('',(-41.9242437426064,93.8,-57.8026659911771));
#58730=CARTESIAN_POINT('',(-41.9242437426064,93.8,-57.8026659911771));
#58731=CARTESIAN_POINT('',(-41.4911089401976,93.8,-60.6567380954302));
#58732=CARTESIAN_POINT('',(-41.4911089401976,93.8,-60.6567380954302));
#58733=CARTESIAN_POINT('',(-38.8028425924776,93.8,-61.7086684054076));
#58734=CARTESIAN_POINT('',(-38.8028425924776,93.8,-61.7086684054076));
#58735=CARTESIAN_POINT('',(-36.5477110471663,93.8,-59.9065266111319));
#58736=CARTESIAN_POINT('',(33.9876798548037,93.8,-91.7975024899648));
#58737=CARTESIAN_POINT('',(34.4208146572124,93.8,-94.6515745942179));
#58738=CARTESIAN_POINT('',(33.9876798548037,93.8,-91.7975024899648));
#58739=CARTESIAN_POINT('',(31.2994135070836,93.8,-90.7455721799874));
#58740=CARTESIAN_POINT('',(31.2994135070836,93.8,-90.7455721799874));
#58741=CARTESIAN_POINT('',(29.0442819617723,93.8,-92.5477139742631));
#58742=CARTESIAN_POINT('',(29.0442819617723,93.8,-92.5477139742631));
#58743=CARTESIAN_POINT('',(29.477416764181,93.8,-95.4017860785161));
#58744=CARTESIAN_POINT('',(29.477416764181,93.8,-95.4017860785161));
#58745=CARTESIAN_POINT('',(32.1656831119011,93.8,-96.4537163884935));
#58746=CARTESIAN_POINT('',(32.1656831119011,93.8,-96.4537163884935));
#58747=CARTESIAN_POINT('',(34.4208146572124,93.8,-94.6515745942179));
#58748=CARTESIAN_POINT('',(40.9720007025968,93.8,-94.5304976043187));
#58749=CARTESIAN_POINT('',(41.4051355050055,93.8,-97.3845697085718));
#58750=CARTESIAN_POINT('',(40.9720007025968,93.8,-94.5304976043187));
#58751=CARTESIAN_POINT('',(38.2837343548768,93.8,-93.4785672943413));
#58752=CARTESIAN_POINT('',(38.2837343548768,93.8,-93.4785672943413));
#58753=CARTESIAN_POINT('',(36.0286028095654,93.8,-95.280709088617));
#58754=CARTESIAN_POINT('',(36.0286028095654,93.8,-95.280709088617));
#58755=CARTESIAN_POINT('',(36.4617376119742,93.8,-98.13478119287));
#58756=CARTESIAN_POINT('',(36.4617376119742,93.8,-98.13478119287));
#58757=CARTESIAN_POINT('',(39.1500039596942,93.8,-99.1867115028474));
#58758=CARTESIAN_POINT('',(39.1500039596942,93.8,-99.1867115028474));
#58759=CARTESIAN_POINT('',(41.4051355050055,93.8,-97.3845697085718));
#58760=CARTESIAN_POINT('',(47.9563215503899,93.8,-97.2634927186726));
#58761=CARTESIAN_POINT('',(48.3894563527986,93.8,-100.117564822926));
#58762=CARTESIAN_POINT('',(47.9563215503899,93.8,-97.2634927186726));
#58763=CARTESIAN_POINT('',(45.2680552026699,93.8,-96.2115624086952));
#58764=CARTESIAN_POINT('',(45.2680552026699,93.8,-96.2115624086952));
#58765=CARTESIAN_POINT('',(43.0129236573585,93.8,-98.0137042029708));
#58766=CARTESIAN_POINT('',(43.0129236573585,93.8,-98.0137042029708));
#58767=CARTESIAN_POINT('',(43.4460584597673,93.8,-100.867776307224));
#58768=CARTESIAN_POINT('',(43.4460584597673,93.8,-100.867776307224));
#58769=CARTESIAN_POINT('',(46.1343248074873,93.8,-101.919706617201));
#58770=CARTESIAN_POINT('',(46.1343248074873,93.8,-101.919706617201));
#58771=CARTESIAN_POINT('',(48.3894563527986,93.8,-100.117564822926));
#58772=CARTESIAN_POINT('',(-43.9651666973681,93.8,-54.3194593925249));
#58773=CARTESIAN_POINT('',(-43.5320318949594,93.8,-57.1735314967781));
#58774=CARTESIAN_POINT('',(-43.9651666973681,93.8,-54.3194593925249));
#58775=CARTESIAN_POINT('',(-46.6534330450882,93.8,-53.2675290825475));
#58776=CARTESIAN_POINT('',(-46.6534330450882,93.8,-53.2675290825475));
#58777=CARTESIAN_POINT('',(-48.9085645903995,93.8,-55.0696708768232));
#58778=CARTESIAN_POINT('',(-48.9085645903995,93.8,-55.0696708768232));
#58779=CARTESIAN_POINT('',(-48.4754297879908,93.8,-57.9237429810763));
#58780=CARTESIAN_POINT('',(-48.4754297879908,93.8,-57.9237429810763));
#58781=CARTESIAN_POINT('',(-45.7871634402707,93.8,-58.9756732910537));
#58782=CARTESIAN_POINT('',(-45.7871634402707,93.8,-58.9756732910537));
#58783=CARTESIAN_POINT('',(-43.5320318949594,93.8,-57.1735314967781));
#58784=CARTESIAN_POINT('',(-41.7145322444734,93.8,-69.1496530716191));
#58785=CARTESIAN_POINT('',(-41.2813974420647,93.8,-72.0037251758721));
#58786=CARTESIAN_POINT('',(-41.7145322444734,93.8,-69.1496530716191));
#58787=CARTESIAN_POINT('',(-44.4027985921934,93.8,-68.0977227616416));
#58788=CARTESIAN_POINT('',(-44.4027985921934,93.8,-68.0977227616416));
#58789=CARTESIAN_POINT('',(-46.6579301375048,93.8,-69.8998645559173));
#58790=CARTESIAN_POINT('',(-46.6579301375048,93.8,-69.8998645559173));
#58791=CARTESIAN_POINT('',(-46.224795335096,93.8,-72.7539366601704));
#58792=CARTESIAN_POINT('',(-46.224795335096,93.8,-72.7539366601704));
#58793=CARTESIAN_POINT('',(-43.536528987376,93.8,-73.8058669701478));
#58794=CARTESIAN_POINT('',(-43.536528987376,93.8,-73.8058669701478));
#58795=CARTESIAN_POINT('',(-41.2813974420647,93.8,-72.0037251758721));
#58796=CARTESIAN_POINT('',(-34.7302113966803,93.8,-71.8826481859729));
#58797=CARTESIAN_POINT('',(-34.2970765942716,93.8,-74.7367202902261));
#58798=CARTESIAN_POINT('',(-34.7302113966803,93.8,-71.8826481859729));
#58799=CARTESIAN_POINT('',(-37.4184777444003,93.8,-70.8307178759955));
#58800=CARTESIAN_POINT('',(-37.4184777444003,93.8,-70.8307178759955));
#58801=CARTESIAN_POINT('',(-39.6736092897116,93.8,-72.6328596702712));
#58802=CARTESIAN_POINT('',(-39.6736092897116,93.8,-72.6328596702712));
#58803=CARTESIAN_POINT('',(-39.2404744873029,93.8,-75.4869317745243));
#58804=CARTESIAN_POINT('',(-39.2404744873029,93.8,-75.4869317745243));
#58805=CARTESIAN_POINT('',(-36.5522081395829,93.8,-76.5388620845017));
#58806=CARTESIAN_POINT('',(-36.5522081395829,93.8,-76.5388620845017));
#58807=CARTESIAN_POINT('',(-34.2970765942716,93.8,-74.7367202902261));
#58808=CARTESIAN_POINT('',(-27.7458905488871,93.8,-74.6156433003268));
#58809=CARTESIAN_POINT('',(-27.3127557464784,93.8,-77.4697154045799));
#58810=CARTESIAN_POINT('',(-27.7458905488871,93.8,-74.6156433003268));
#58811=CARTESIAN_POINT('',(-30.4341568966072,93.8,-73.5637129903494));
#58812=CARTESIAN_POINT('',(-30.4341568966072,93.8,-73.5637129903494));
#58813=CARTESIAN_POINT('',(-32.6892884419185,93.8,-75.3658547846251));
#58814=CARTESIAN_POINT('',(-32.6892884419185,93.8,-75.3658547846251));
#58815=CARTESIAN_POINT('',(-32.2561536395098,93.8,-78.2199268888782));
#58816=CARTESIAN_POINT('',(-32.2561536395098,93.8,-78.2199268888782));
#58817=CARTESIAN_POINT('',(-29.5678872917897,93.8,-79.2718571988556));
#58818=CARTESIAN_POINT('',(-29.5678872917897,93.8,-79.2718571988556));
#58819=CARTESIAN_POINT('',(-27.3127557464784,93.8,-77.4697154045799));
#58820=CARTESIAN_POINT('',(-20.761569701094,93.8,-77.3486384146807));
#58821=CARTESIAN_POINT('',(-20.3284348986853,93.8,-80.2027105189338));
#58822=CARTESIAN_POINT('',(-20.761569701094,93.8,-77.3486384146807));
#58823=CARTESIAN_POINT('',(-23.449836048814,93.8,-76.2967081047033));
#58824=CARTESIAN_POINT('',(-23.449836048814,93.8,-76.2967081047033));
#58825=CARTESIAN_POINT('',(-25.7049675941254,93.8,-78.098849898979));
#58826=CARTESIAN_POINT('',(-25.7049675941254,93.8,-78.098849898979));
#58827=CARTESIAN_POINT('',(-25.2718327917166,93.8,-80.9529220032321));
#58828=CARTESIAN_POINT('',(-25.2718327917166,93.8,-80.9529220032321));
#58829=CARTESIAN_POINT('',(-22.5835664439966,93.8,-82.0048523132095));
#58830=CARTESIAN_POINT('',(-22.5835664439966,93.8,-82.0048523132095));
#58831=CARTESIAN_POINT('',(-20.3284348986853,93.8,-80.2027105189338));
#58832=CARTESIAN_POINT('',(-13.7772488533009,93.8,-80.0816335290346));
#58833=CARTESIAN_POINT('',(-13.3441140508922,93.8,-82.9357056332877));
#58834=CARTESIAN_POINT('',(-13.7772488533009,93.8,-80.0816335290346));
#58835=CARTESIAN_POINT('',(-16.4655152010209,93.8,-79.0297032190572));
#58836=CARTESIAN_POINT('',(-16.4655152010209,93.8,-79.0297032190572));
#58837=CARTESIAN_POINT('',(-18.7206467463322,93.8,-80.8318450133329));
#58838=CARTESIAN_POINT('',(-18.7206467463322,93.8,-80.8318450133329));
#58839=CARTESIAN_POINT('',(-18.2875119439235,93.8,-83.685917117586));
#58840=CARTESIAN_POINT('',(-18.2875119439235,93.8,-83.685917117586));
#58841=CARTESIAN_POINT('',(-15.5992455962035,93.8,-84.7378474275634));
#58842=CARTESIAN_POINT('',(-15.5992455962035,93.8,-84.7378474275634));
#58843=CARTESIAN_POINT('',(-13.3441140508922,93.8,-82.9357056332877));
#58844=CARTESIAN_POINT('',(-6.79292800550775,93.8,-82.8146286433885));
#58845=CARTESIAN_POINT('',(-6.35979320309903,93.8,-85.6687007476416));
#58846=CARTESIAN_POINT('',(-6.79292800550775,93.8,-82.8146286433885));
#58847=CARTESIAN_POINT('',(-9.48119435322776,93.8,-81.7626983334111));
#58848=CARTESIAN_POINT('',(-9.48119435322776,93.8,-81.7626983334111));
#58849=CARTESIAN_POINT('',(-11.7363258985391,93.8,-83.5648401276868));
#58850=CARTESIAN_POINT('',(-11.7363258985391,93.8,-83.5648401276868));
#58851=CARTESIAN_POINT('',(-11.3031910961304,93.8,-86.4189122319399));
#58852=CARTESIAN_POINT('',(-11.3031910961304,93.8,-86.4189122319399));
#58853=CARTESIAN_POINT('',(-8.61492474841036,93.8,-87.4708425419173));
#58854=CARTESIAN_POINT('',(-8.61492474841036,93.8,-87.4708425419173));
#58855=CARTESIAN_POINT('',(-6.35979320309903,93.8,-85.6687007476416));
#58856=CARTESIAN_POINT('',(0.191392842285382,93.8,-85.5476237577424));
#58857=CARTESIAN_POINT('',(0.6245276446941,93.8,-88.4016958619955));
#58858=CARTESIAN_POINT('',(0.191392842285382,93.8,-85.5476237577424));
#58859=CARTESIAN_POINT('',(-2.49687350543463,93.8,-84.495693447765));
#58860=CARTESIAN_POINT('',(-2.49687350543463,93.8,-84.495693447765));
#58861=CARTESIAN_POINT('',(-4.75200505074598,93.8,-86.2978352420407));
#58862=CARTESIAN_POINT('',(-4.75200505074598,93.8,-86.2978352420407));
#58863=CARTESIAN_POINT('',(-4.31887024833725,93.8,-89.1519073462937));
#58864=CARTESIAN_POINT('',(-4.31887024833725,93.8,-89.1519073462937));
#58865=CARTESIAN_POINT('',(-1.63060390061722,93.8,-90.2038376562712));
#58866=CARTESIAN_POINT('',(-1.63060390061722,93.8,-90.2038376562712));
#58867=CARTESIAN_POINT('',(0.6245276446941,93.8,-88.4016958619955));
#58868=CARTESIAN_POINT('',(7.17571369007852,93.8,-88.2806188720963));
#58869=CARTESIAN_POINT('',(7.60884849248723,93.8,-91.1346909763494));
#58870=CARTESIAN_POINT('',(7.17571369007852,93.8,-88.2806188720963));
#58871=CARTESIAN_POINT('',(4.4874473423585,93.8,-87.2286885621189));
#58872=CARTESIAN_POINT('',(4.4874473423585,93.8,-87.2286885621189));
#58873=CARTESIAN_POINT('',(2.23231579704715,93.8,-89.0308303563946));
#58874=CARTESIAN_POINT('',(2.23231579704715,93.8,-89.0308303563946));
#58875=CARTESIAN_POINT('',(2.66545059945588,93.8,-91.8849024606476));
#58876=CARTESIAN_POINT('',(2.66545059945588,93.8,-91.8849024606476));
#58877=CARTESIAN_POINT('',(5.35371694717591,93.8,-92.936832770625));
#58878=CARTESIAN_POINT('',(5.35371694717591,93.8,-92.936832770625));
#58879=CARTESIAN_POINT('',(7.60884849248723,93.8,-91.1346909763494));
#58880=CARTESIAN_POINT('',(42.0973179290442,93.8,-101.945594443866));
#58881=CARTESIAN_POINT('',(42.5304527314529,93.8,-104.799666548119));
#58882=CARTESIAN_POINT('',(42.0973179290442,93.8,-101.945594443866));
#58883=CARTESIAN_POINT('',(39.4090515813242,93.8,-100.893664133888));
#58884=CARTESIAN_POINT('',(39.4090515813242,93.8,-100.893664133888));
#58885=CARTESIAN_POINT('',(37.1539200360128,93.8,-102.695805928164));
#58886=CARTESIAN_POINT('',(37.1539200360128,93.8,-102.695805928164));
#58887=CARTESIAN_POINT('',(37.5870548384215,93.8,-105.549878032417));
#58888=CARTESIAN_POINT('',(37.5870548384215,93.8,-105.549878032417));
#58889=CARTESIAN_POINT('',(40.2753211861416,93.8,-106.601808342394));
#58890=CARTESIAN_POINT('',(40.2753211861416,93.8,-106.601808342394));
#58891=CARTESIAN_POINT('',(42.5304527314529,93.8,-104.799666548119));
#58892=CARTESIAN_POINT('',(-42.8398494709208,93.8,-61.734556232072));
#58893=CARTESIAN_POINT('',(-42.4067146685121,93.8,-64.5886283363251));
#58894=CARTESIAN_POINT('',(-42.8398494709208,93.8,-61.734556232072));
#58895=CARTESIAN_POINT('',(-45.5281158186408,93.8,-60.6826259220946));
#58896=CARTESIAN_POINT('',(-45.5281158186408,93.8,-60.6826259220946));
#58897=CARTESIAN_POINT('',(-47.7832473639521,93.8,-62.4847677163703));
#58898=CARTESIAN_POINT('',(-47.7832473639521,93.8,-62.4847677163703));
#58899=CARTESIAN_POINT('',(-47.3501125615434,93.8,-65.3388398206233));
#58900=CARTESIAN_POINT('',(-47.3501125615434,93.8,-65.3388398206233));
#58901=CARTESIAN_POINT('',(-44.6618462138234,93.8,-66.3907701306008));
#58902=CARTESIAN_POINT('',(-44.6618462138234,93.8,-66.3907701306008));
#58903=CARTESIAN_POINT('',(-42.4067146685121,93.8,-64.5886283363251));
#58904=CARTESIAN_POINT('',(-35.8555286231276,93.8,-64.4675513464259));
#58905=CARTESIAN_POINT('',(-35.4223938207189,93.8,-67.321623450679));
#58906=CARTESIAN_POINT('',(-35.8555286231276,93.8,-64.4675513464259));
#58907=CARTESIAN_POINT('',(-38.5437949708476,93.8,-63.4156210364485));
#58908=CARTESIAN_POINT('',(-38.5437949708476,93.8,-63.4156210364485));
#58909=CARTESIAN_POINT('',(-40.798926516159,93.8,-65.2177628307242));
#58910=CARTESIAN_POINT('',(-40.798926516159,93.8,-65.2177628307242));
#58911=CARTESIAN_POINT('',(-40.3657917137503,93.8,-68.0718349349772));
#58912=CARTESIAN_POINT('',(-40.3657917137503,93.8,-68.0718349349772));
#58913=CARTESIAN_POINT('',(-37.6775253660303,93.8,-69.1237652449547));
#58914=CARTESIAN_POINT('',(-37.6775253660303,93.8,-69.1237652449547));
#58915=CARTESIAN_POINT('',(-35.4223938207189,93.8,-67.321623450679));
#58916=CARTESIAN_POINT('',(-28.8712077753345,93.8,-67.2005464607798));
#58917=CARTESIAN_POINT('',(-28.4380729729258,93.8,-70.0546185650329));
#58918=CARTESIAN_POINT('',(-28.8712077753345,93.8,-67.2005464607798));
#58919=CARTESIAN_POINT('',(-31.5594741230545,93.8,-66.1486161508024));
#58920=CARTESIAN_POINT('',(-31.5594741230545,93.8,-66.1486161508024));
#58921=CARTESIAN_POINT('',(-33.8146056683659,93.8,-67.9507579450781));
#58922=CARTESIAN_POINT('',(-33.8146056683659,93.8,-67.9507579450781));
#58923=CARTESIAN_POINT('',(-33.3814708659571,93.8,-70.8048300493311));
#58924=CARTESIAN_POINT('',(-33.3814708659571,93.8,-70.8048300493311));
#58925=CARTESIAN_POINT('',(-30.6932045182371,93.8,-71.8567603593086));
#58926=CARTESIAN_POINT('',(-30.6932045182371,93.8,-71.8567603593086));
#58927=CARTESIAN_POINT('',(-28.4380729729258,93.8,-70.0546185650329));
#58928=CARTESIAN_POINT('',(35.112997081251,93.8,-99.2125993295118));
#58929=CARTESIAN_POINT('',(35.5461318836598,93.8,-102.066671433765));
#58930=CARTESIAN_POINT('',(35.112997081251,93.8,-99.2125993295118));
#58931=CARTESIAN_POINT('',(32.424730733531,93.8,-98.1606690195344));
#58932=CARTESIAN_POINT('',(32.424730733531,93.8,-98.1606690195344));
#58933=CARTESIAN_POINT('',(30.1695991882197,93.8,-99.9628108138101));
#58934=CARTESIAN_POINT('',(30.1695991882197,93.8,-99.9628108138101));
#58935=CARTESIAN_POINT('',(30.6027339906284,93.8,-102.816882918063));
#58936=CARTESIAN_POINT('',(30.6027339906284,93.8,-102.816882918063));
#58937=CARTESIAN_POINT('',(33.2910003383484,93.8,-103.868813228041));
#58938=CARTESIAN_POINT('',(33.2910003383484,93.8,-103.868813228041));
#58939=CARTESIAN_POINT('',(35.5461318836598,93.8,-102.066671433765));
#58940=CARTESIAN_POINT('',(28.1286762334579,93.8,-96.479604215158));
#58941=CARTESIAN_POINT('',(28.5618110358666,93.8,-99.333676319411));
#58942=CARTESIAN_POINT('',(28.1286762334579,93.8,-96.479604215158));
#58943=CARTESIAN_POINT('',(25.4404098857379,93.8,-95.4276739051805));
#58944=CARTESIAN_POINT('',(25.4404098857379,93.8,-95.4276739051805));
#58945=CARTESIAN_POINT('',(23.1852783404265,93.8,-97.2298156994562));
#58946=CARTESIAN_POINT('',(23.1852783404265,93.8,-97.2298156994562));
#58947=CARTESIAN_POINT('',(23.6184131428353,93.8,-100.083887803709));
#58948=CARTESIAN_POINT('',(23.6184131428353,93.8,-100.083887803709));
#58949=CARTESIAN_POINT('',(26.3066794905553,93.8,-101.135818113687));
#58950=CARTESIAN_POINT('',(26.3066794905553,93.8,-101.135818113687));
#58951=CARTESIAN_POINT('',(28.5618110358666,93.8,-99.3336763194111));
#58952=CARTESIAN_POINT('',(21.1443553856648,93.8,-93.7466091008041));
#58953=CARTESIAN_POINT('',(21.5774901880735,93.8,-96.6006812050572));
#58954=CARTESIAN_POINT('',(21.1443553856648,93.8,-93.7466091008041));
#58955=CARTESIAN_POINT('',(18.4560890379448,93.8,-92.6946787908267));
#58956=CARTESIAN_POINT('',(18.4560890379448,93.8,-92.6946787908267));
#58957=CARTESIAN_POINT('',(16.2009574926334,93.8,-94.4968205851023));
#58958=CARTESIAN_POINT('',(16.2009574926334,93.8,-94.4968205851023));
#58959=CARTESIAN_POINT('',(16.6340922950421,93.8,-97.3508926893554));
#58960=CARTESIAN_POINT('',(16.6340922950421,93.8,-97.3508926893554));
#58961=CARTESIAN_POINT('',(19.3223586427622,93.8,-98.4028229993328));
#58962=CARTESIAN_POINT('',(19.3223586427622,93.8,-98.4028229993328));
#58963=CARTESIAN_POINT('',(21.5774901880735,93.8,-96.6006812050572));
#58964=CARTESIAN_POINT('',(14.1600345378716,93.8,-91.0136139864502));
#58965=CARTESIAN_POINT('',(14.5931693402804,93.8,-93.8676860907033));
#58966=CARTESIAN_POINT('',(14.1600345378716,93.8,-91.0136139864502));
#58967=CARTESIAN_POINT('',(11.4717681901516,93.8,-89.9616836764728));
#58968=CARTESIAN_POINT('',(11.4717681901516,93.8,-89.9616836764728));
#58969=CARTESIAN_POINT('',(9.21663664484028,93.8,-91.7638254707484));
#58970=CARTESIAN_POINT('',(9.21663664484028,93.8,-91.7638254707484));
#58971=CARTESIAN_POINT('',(9.64977144724901,93.8,-94.6178975750015));
#58972=CARTESIAN_POINT('',(9.64977144724901,93.8,-94.6178975750015));
#58973=CARTESIAN_POINT('',(12.338037794969,93.8,-95.6698278849789));
#58974=CARTESIAN_POINT('',(12.338037794969,93.8,-95.6698278849789));
#58975=CARTESIAN_POINT('',(14.5931693402804,93.8,-93.8676860907033));
#58976=CARTESIAN_POINT('',(38.721366249702,93.8,-79.7003039252246));
#58977=CARTESIAN_POINT('',(39.1545010521108,93.8,-82.5543760294777));
#58978=CARTESIAN_POINT('',(38.721366249702,93.8,-79.7003039252246));
#58979=CARTESIAN_POINT('',(36.033099901982,93.8,-78.6483736152472));
#58980=CARTESIAN_POINT('',(36.033099901982,93.8,-78.6483736152472));
#58981=CARTESIAN_POINT('',(33.7779683566707,93.8,-80.4505154095229));
#58982=CARTESIAN_POINT('',(33.7779683566707,93.8,-80.4505154095229));
#58983=CARTESIAN_POINT('',(34.2111031590794,93.8,-83.3045875137759));
#58984=CARTESIAN_POINT('',(34.2111031590794,93.8,-83.3045875137759));
#58985=CARTESIAN_POINT('',(36.8993695067994,93.8,-84.3565178237533));
#58986=CARTESIAN_POINT('',(36.8993695067994,93.8,-84.3565178237533));
#58987=CARTESIAN_POINT('',(39.1545010521108,93.8,-82.5543760294777));
#58988=CARTESIAN_POINT('',(45.7056870974952,93.8,-82.4332990395785));
#58989=CARTESIAN_POINT('',(46.1388218999039,93.8,-85.2873711438316));
#58990=CARTESIAN_POINT('',(45.7056870974952,93.8,-82.4332990395785));
#58991=CARTESIAN_POINT('',(43.0174207497752,93.8,-81.381368729601));
#58992=CARTESIAN_POINT('',(43.0174207497752,93.8,-81.381368729601));
#58993=CARTESIAN_POINT('',(40.7622892044638,93.8,-83.1835105238767));
#58994=CARTESIAN_POINT('',(40.7622892044638,93.8,-83.1835105238767));
#58995=CARTESIAN_POINT('',(41.1954240068725,93.8,-86.0375826281298));
#58996=CARTESIAN_POINT('',(41.1954240068725,93.8,-86.0375826281298));
#58997=CARTESIAN_POINT('',(43.8836903545926,93.8,-87.0895129381072));
#58998=CARTESIAN_POINT('',(43.8836903545926,93.8,-87.0895129381072));
#58999=CARTESIAN_POINT('',(46.1388218999039,93.8,-85.2873711438316));
#59000=CARTESIAN_POINT('',(52.6900079452883,93.8,-85.1662941539323));
#59001=CARTESIAN_POINT('',(53.123142747697,93.8,-88.0203662581854));
#59002=CARTESIAN_POINT('',(52.6900079452883,93.8,-85.1662941539323));
#59003=CARTESIAN_POINT('',(50.0017415975683,93.8,-84.1143638439549));
#59004=CARTESIAN_POINT('',(50.0017415975683,93.8,-84.1143638439549));
#59005=CARTESIAN_POINT('',(47.7466100522569,93.8,-85.9165056382306));
#59006=CARTESIAN_POINT('',(47.7466100522569,93.8,-85.9165056382306));
#59007=CARTESIAN_POINT('',(48.1797448546657,93.8,-88.7705777424837));
#59008=CARTESIAN_POINT('',(48.1797448546657,93.8,-88.7705777424837));
#59009=CARTESIAN_POINT('',(50.8680112023857,93.8,-89.8225080524611));
#59010=CARTESIAN_POINT('',(50.8680112023857,93.8,-89.8225080524611));
#59011=CARTESIAN_POINT('',(53.123142747697,93.8,-88.0203662581854));
#59012=CARTESIAN_POINT('',(-39.2314803024698,93.8,-42.2222608277847));
#59013=CARTESIAN_POINT('',(-38.798345500061,93.8,-45.0763329320378));
#59014=CARTESIAN_POINT('',(-39.2314803024698,93.8,-42.2222608277847));
#59015=CARTESIAN_POINT('',(-41.9197466501898,93.8,-41.1703305178073));
#59016=CARTESIAN_POINT('',(-41.9197466501898,93.8,-41.1703305178073));
#59017=CARTESIAN_POINT('',(-44.1748781955011,93.8,-42.972472312083));
#59018=CARTESIAN_POINT('',(-44.1748781955011,93.8,-42.972472312083));
#59019=CARTESIAN_POINT('',(-43.7417433930924,93.8,-45.8265444163361));
#59020=CARTESIAN_POINT('',(-43.7417433930924,93.8,-45.8265444163361));
#59021=CARTESIAN_POINT('',(-41.0534770453724,93.8,-46.8784747263135));
#59022=CARTESIAN_POINT('',(-41.0534770453724,93.8,-46.8784747263135));
#59023=CARTESIAN_POINT('',(-38.798345500061,93.8,-45.0763329320378));
#59024=CARTESIAN_POINT('',(31.7370454019089,93.8,-76.9673088108707));
#59025=CARTESIAN_POINT('',(32.1701802043176,93.8,-79.8213809151238));
#59026=CARTESIAN_POINT('',(31.7370454019089,93.8,-76.9673088108707));
#59027=CARTESIAN_POINT('',(29.0487790541889,93.8,-75.9153785008933));
#59028=CARTESIAN_POINT('',(29.0487790541889,93.8,-75.9153785008933));
#59029=CARTESIAN_POINT('',(26.7936475088776,93.8,-77.717520295169));
#59030=CARTESIAN_POINT('',(26.7936475088776,93.8,-77.717520295169));
#59031=CARTESIAN_POINT('',(27.2267823112863,93.8,-80.571592399422));
#59032=CARTESIAN_POINT('',(27.2267823112863,93.8,-80.571592399422));
#59033=CARTESIAN_POINT('',(29.9150486590063,93.8,-81.6235227093995));
#59034=CARTESIAN_POINT('',(29.9150486590063,93.8,-81.6235227093995));
#59035=CARTESIAN_POINT('',(32.1701802043176,93.8,-79.8213809151238));
#59036=CARTESIAN_POINT('',(24.7527245541158,93.8,-74.2343136965168));
#59037=CARTESIAN_POINT('',(25.1858593565245,93.8,-77.0883858007699));
#59038=CARTESIAN_POINT('',(24.7527245541158,93.8,-74.2343136965168));
#59039=CARTESIAN_POINT('',(22.0644582063958,93.8,-73.1823833865394));
#59040=CARTESIAN_POINT('',(22.0644582063958,93.8,-73.1823833865394));
#59041=CARTESIAN_POINT('',(19.8093266610844,93.8,-74.9845251808151));
#59042=CARTESIAN_POINT('',(19.8093266610844,93.8,-74.9845251808151));
#59043=CARTESIAN_POINT('',(20.2424614634932,93.8,-77.8385972850681));
#59044=CARTESIAN_POINT('',(20.2424614634932,93.8,-77.8385972850681));
#59045=CARTESIAN_POINT('',(22.9307278112132,93.8,-78.8905275950456));
#59046=CARTESIAN_POINT('',(22.9307278112132,93.8,-78.8905275950456));
#59047=CARTESIAN_POINT('',(25.1858593565245,93.8,-77.0883858007699));
#59048=CARTESIAN_POINT('',(17.7684037063227,93.8,-71.5013185821629));
#59049=CARTESIAN_POINT('',(18.2015385087314,93.8,-74.355390686416));
#59050=CARTESIAN_POINT('',(17.7684037063227,93.8,-71.5013185821629));
#59051=CARTESIAN_POINT('',(15.0801373586026,93.8,-70.4493882721855));
#59052=CARTESIAN_POINT('',(15.0801373586026,93.8,-70.4493882721855));
#59053=CARTESIAN_POINT('',(12.8250058132913,93.8,-72.2515300664612));
#59054=CARTESIAN_POINT('',(12.8250058132913,93.8,-72.2515300664612));
#59055=CARTESIAN_POINT('',(13.2581406157,93.8,-75.1056021707142));
#59056=CARTESIAN_POINT('',(13.2581406157,93.8,-75.1056021707142));
#59057=CARTESIAN_POINT('',(15.94640696342,93.8,-76.1575324806917));
#59058=CARTESIAN_POINT('',(15.94640696342,93.8,-76.1575324806917));
#59059=CARTESIAN_POINT('',(18.2015385087314,93.8,-74.355390686416));
#59060=CARTESIAN_POINT('',(10.7840828585295,93.8,-68.768323467809));
#59061=CARTESIAN_POINT('',(11.2172176609382,93.8,-71.6223955720621));
#59062=CARTESIAN_POINT('',(10.7840828585295,93.8,-68.768323467809));
#59063=CARTESIAN_POINT('',(8.09581651080951,93.8,-67.7163931578316));
#59064=CARTESIAN_POINT('',(8.09581651080951,93.8,-67.7163931578316));
#59065=CARTESIAN_POINT('',(5.84068496549816,93.8,-69.5185349521073));
#59066=CARTESIAN_POINT('',(5.84068496549816,93.8,-69.5185349521073));
#59067=CARTESIAN_POINT('',(6.27381976790689,93.8,-72.3726070563604));
#59068=CARTESIAN_POINT('',(6.27381976790689,93.8,-72.3726070563604));
#59069=CARTESIAN_POINT('',(8.96208611562692,93.8,-73.4245373663378));
#59070=CARTESIAN_POINT('',(8.96208611562692,93.8,-73.4245373663378));
#59071=CARTESIAN_POINT('',(11.2172176609382,93.8,-71.6223955720621));
#59072=CARTESIAN_POINT('',(-32.2471594546766,93.8,-44.9552559421386));
#59073=CARTESIAN_POINT('',(-31.8140246522679,93.8,-47.8093280463917));
#59074=CARTESIAN_POINT('',(-32.2471594546766,93.8,-44.9552559421386));
#59075=CARTESIAN_POINT('',(-34.9354258023966,93.8,-43.9033256321612));
#59076=CARTESIAN_POINT('',(-34.9354258023966,93.8,-43.9033256321612));
#59077=CARTESIAN_POINT('',(-37.190557347708,93.8,-45.7054674264369));
#59078=CARTESIAN_POINT('',(-37.190557347708,93.8,-45.7054674264369));
#59079=CARTESIAN_POINT('',(-36.7574225452993,93.8,-48.55953953069));
#59080=CARTESIAN_POINT('',(-36.7574225452993,93.8,-48.55953953069));
#59081=CARTESIAN_POINT('',(-34.0691561975792,93.8,-49.6114698406674));
#59082=CARTESIAN_POINT('',(-34.0691561975792,93.8,-49.6114698406674));
#59083=CARTESIAN_POINT('',(-31.8140246522679,93.8,-47.8093280463917));
#59084=CARTESIAN_POINT('',(-25.2628386068835,93.8,-47.6882510564925));
#59085=CARTESIAN_POINT('',(-24.8297038044748,93.8,-50.5423231607456));
#59086=CARTESIAN_POINT('',(-25.2628386068835,93.8,-47.6882510564925));
#59087=CARTESIAN_POINT('',(-27.9511049546035,93.8,-46.6363207465151));
#59088=CARTESIAN_POINT('',(-27.9511049546035,93.8,-46.6363207465151));
#59089=CARTESIAN_POINT('',(-30.2062364999149,93.8,-48.4384625407908));
#59090=CARTESIAN_POINT('',(-30.2062364999149,93.8,-48.4384625407908));
#59091=CARTESIAN_POINT('',(-29.7731016975061,93.8,-51.2925346450439));
#59092=CARTESIAN_POINT('',(-29.7731016975061,93.8,-51.2925346450439));
#59093=CARTESIAN_POINT('',(-27.0848353497861,93.8,-52.3444649550213));
#59094=CARTESIAN_POINT('',(-27.0848353497861,93.8,-52.3444649550213));
#59095=CARTESIAN_POINT('',(-24.8297038044748,93.8,-50.5423231607456));
#59096=CARTESIAN_POINT('',(-18.2785177590904,93.8,-50.4212461708464));
#59097=CARTESIAN_POINT('',(-17.8453829566817,93.8,-53.2753182750995));
#59098=CARTESIAN_POINT('',(-18.2785177590904,93.8,-50.4212461708464));
#59099=CARTESIAN_POINT('',(-20.9667841068104,93.8,-49.369315860869));
#59100=CARTESIAN_POINT('',(-20.9667841068104,93.8,-49.369315860869));
#59101=CARTESIAN_POINT('',(-23.2219156521217,93.8,-51.1714576551447));
#59102=CARTESIAN_POINT('',(-23.2219156521217,93.8,-51.1714576551447));
#59103=CARTESIAN_POINT('',(-22.788780849713,93.8,-54.0255297593977));
#59104=CARTESIAN_POINT('',(-22.788780849713,93.8,-54.0255297593977));
#59105=CARTESIAN_POINT('',(-20.100514501993,93.8,-55.0774600693752));
#59106=CARTESIAN_POINT('',(-20.100514501993,93.8,-55.0774600693752));
#59107=CARTESIAN_POINT('',(-17.8453829566817,93.8,-53.2753182750995));
#59108=CARTESIAN_POINT('',(-11.2941969112972,93.8,-53.1542412852003));
#59109=CARTESIAN_POINT('',(-10.8610621088885,93.8,-56.0083133894534));
#59110=CARTESIAN_POINT('',(-11.2941969112972,93.8,-53.1542412852003));
#59111=CARTESIAN_POINT('',(-13.9824632590173,93.8,-52.1023109752229));
#59112=CARTESIAN_POINT('',(-13.9824632590173,93.8,-52.1023109752229));
#59113=CARTESIAN_POINT('',(-16.2375948043286,93.8,-53.9044527694986));
#59114=CARTESIAN_POINT('',(-16.2375948043286,93.8,-53.9044527694986));
#59115=CARTESIAN_POINT('',(-15.8044600019199,93.8,-56.7585248737516));
#59116=CARTESIAN_POINT('',(-15.8044600019199,93.8,-56.7585248737516));
#59117=CARTESIAN_POINT('',(-13.1161936541999,93.8,-57.8104551837291));
#59118=CARTESIAN_POINT('',(-13.1161936541999,93.8,-57.8104551837291));
#59119=CARTESIAN_POINT('',(-10.8610621088885,93.8,-56.0083133894534));
#59120=CARTESIAN_POINT('',(-4.30987606350412,93.8,-55.8872363995542));
#59121=CARTESIAN_POINT('',(-3.8767412610954,93.8,-58.7413085038073));
#59122=CARTESIAN_POINT('',(-4.30987606350412,93.8,-55.8872363995542));
#59123=CARTESIAN_POINT('',(-6.99814241122413,93.8,-54.8353060895768));
#59124=CARTESIAN_POINT('',(-6.99814241122413,93.8,-54.8353060895768));
#59125=CARTESIAN_POINT('',(-9.25327395653548,93.8,-56.6374478838525));
#59126=CARTESIAN_POINT('',(-9.25327395653548,93.8,-56.6374478838525));
#59127=CARTESIAN_POINT('',(-8.82013915412675,93.8,-59.4915199881055));
#59128=CARTESIAN_POINT('',(-8.82013915412675,93.8,-59.4915199881055));
#59129=CARTESIAN_POINT('',(-6.13187280640672,93.8,-60.543450298083));
#59130=CARTESIAN_POINT('',(-6.13187280640672,93.8,-60.543450298083));
#59131=CARTESIAN_POINT('',(-3.8767412610954,93.8,-58.7413085038073));
#59132=CARTESIAN_POINT('',(2.67444478428902,93.8,-58.6202315139081));
#59133=CARTESIAN_POINT('',(3.10757958669774,93.8,-61.4743036181612));
#59134=CARTESIAN_POINT('',(2.67444478428902,93.8,-58.6202315139081));
#59135=CARTESIAN_POINT('',(-0.0138215634309935,93.8,-57.5683012039307));
#59136=CARTESIAN_POINT('',(-0.0138215634309935,93.8,-57.5683012039307));
#59137=CARTESIAN_POINT('',(-2.26895310874235,93.8,-59.3704429982063));
#59138=CARTESIAN_POINT('',(-2.26895310874235,93.8,-59.3704429982063));
#59139=CARTESIAN_POINT('',(-1.83581830633362,93.8,-62.2245151024594));
#59140=CARTESIAN_POINT('',(-1.83581830633362,93.8,-62.2245151024594));
#59141=CARTESIAN_POINT('',(0.852448041386411,93.8,-63.2764454124368));
#59142=CARTESIAN_POINT('',(0.852448041386411,93.8,-63.2764454124368));
#59143=CARTESIAN_POINT('',(3.10757958669774,93.8,-61.4743036181612));
#59144=CARTESIAN_POINT('',(9.65876563208215,93.8,-61.353226628262));
#59145=CARTESIAN_POINT('',(10.0919004344909,93.8,-64.2072987325151));
#59146=CARTESIAN_POINT('',(9.65876563208215,93.8,-61.353226628262));
#59147=CARTESIAN_POINT('',(6.97049928436214,93.8,-60.3012963182845));
#59148=CARTESIAN_POINT('',(6.97049928436214,93.8,-60.3012963182845));
#59149=CARTESIAN_POINT('',(4.71536773905078,93.8,-62.1034381125602));
#59150=CARTESIAN_POINT('',(4.71536773905078,93.8,-62.1034381125602));
#59151=CARTESIAN_POINT('',(5.14850254145952,93.8,-64.9575102168133));
#59152=CARTESIAN_POINT('',(5.14850254145952,93.8,-64.9575102168133));
#59153=CARTESIAN_POINT('',(7.83676888917954,93.8,-66.0094405267907));
#59154=CARTESIAN_POINT('',(7.83676888917954,93.8,-66.0094405267907));
#59155=CARTESIAN_POINT('',(10.0919004344909,93.8,-64.2072987325151));
#59156=CARTESIAN_POINT('',(16.6430864798753,93.8,-64.0862217426158));
#59157=CARTESIAN_POINT('',(17.076221282284,93.8,-66.940293846869));
#59158=CARTESIAN_POINT('',(16.6430864798753,93.8,-64.0862217426158));
#59159=CARTESIAN_POINT('',(13.9548201321553,93.8,-63.0342914326384));
#59160=CARTESIAN_POINT('',(13.9548201321553,93.8,-63.0342914326384));
#59161=CARTESIAN_POINT('',(11.6996885868439,93.8,-64.8364332269141));
#59162=CARTESIAN_POINT('',(11.6996885868439,93.8,-64.8364332269141));
#59163=CARTESIAN_POINT('',(12.1328233892526,93.8,-67.6905053311672));
#59164=CARTESIAN_POINT('',(12.1328233892526,93.8,-67.6905053311672));
#59165=CARTESIAN_POINT('',(14.8210897369727,93.8,-68.7424356411446));
#59166=CARTESIAN_POINT('',(14.8210897369727,93.8,-68.7424356411446));
#59167=CARTESIAN_POINT('',(17.076221282284,93.8,-66.940293846869));
#59168=CARTESIAN_POINT('',(-9.04356245840249,93.8,-67.9844349642944));
#59169=CARTESIAN_POINT('',(-8.61042765599378,93.8,-70.8385070685475));
#59170=CARTESIAN_POINT('',(-9.04356245840249,93.8,-67.9844349642944));
#59171=CARTESIAN_POINT('',(-11.7318288061225,93.8,-66.932504654317));
#59172=CARTESIAN_POINT('',(-11.7318288061225,93.8,-66.932504654317));
#59173=CARTESIAN_POINT('',(-13.9869603514339,93.8,-68.7346464485927));
#59174=CARTESIAN_POINT('',(-13.9869603514339,93.8,-68.7346464485927));
#59175=CARTESIAN_POINT('',(-13.5538255490251,93.8,-71.5887185528457));
#59176=CARTESIAN_POINT('',(-13.5538255490251,93.8,-71.5887185528457));
#59177=CARTESIAN_POINT('',(-10.8655592013051,93.8,-72.6406488628232));
#59178=CARTESIAN_POINT('',(-10.8655592013051,93.8,-72.6406488628232));
#59179=CARTESIAN_POINT('',(-8.61042765599378,93.8,-70.8385070685475));
#59180=CARTESIAN_POINT('',(-2.05924161060936,93.8,-70.7174300786483));
#59181=CARTESIAN_POINT('',(-1.62610680820064,93.8,-73.5715021829014));
#59182=CARTESIAN_POINT('',(-2.05924161060936,93.8,-70.7174300786483));
#59183=CARTESIAN_POINT('',(-4.74750795832937,93.8,-69.6654997686709));
#59184=CARTESIAN_POINT('',(-4.74750795832937,93.8,-69.6654997686709));
#59185=CARTESIAN_POINT('',(-7.00263950364073,93.8,-71.4676415629466));
#59186=CARTESIAN_POINT('',(-7.00263950364073,93.8,-71.4676415629466));
#59187=CARTESIAN_POINT('',(-6.569504701232,93.8,-74.3217136671996));
#59188=CARTESIAN_POINT('',(-6.569504701232,93.8,-74.3217136671996));
#59189=CARTESIAN_POINT('',(-3.88123835351197,93.8,-75.3736439771771));
#59190=CARTESIAN_POINT('',(-3.88123835351197,93.8,-75.3736439771771));
#59191=CARTESIAN_POINT('',(-1.62610680820064,93.8,-73.5715021829014));
#59192=CARTESIAN_POINT('',(4.92507923718377,93.8,-73.4504251930022));
#59193=CARTESIAN_POINT('',(5.35821403959249,93.8,-76.3044972972553));
#59194=CARTESIAN_POINT('',(4.92507923718377,93.8,-73.4504251930022));
#59195=CARTESIAN_POINT('',(2.23681288946376,93.8,-72.3984948830248));
#59196=CARTESIAN_POINT('',(2.23681288946376,93.8,-72.3984948830248));
#59197=CARTESIAN_POINT('',(-0.0183186558475948,93.8,-74.2006366773005));
#59198=CARTESIAN_POINT('',(-0.0183186558475948,93.8,-74.2006366773005));
#59199=CARTESIAN_POINT('',(0.414816146561137,93.8,-77.0547087815535));
#59200=CARTESIAN_POINT('',(0.414816146561137,93.8,-77.0547087815535));
#59201=CARTESIAN_POINT('',(3.10308249428116,93.8,-78.1066390915309));
#59202=CARTESIAN_POINT('',(3.10308249428116,93.8,-78.1066390915309));
#59203=CARTESIAN_POINT('',(5.35821403959249,93.8,-76.3044972972553));
#59204=CARTESIAN_POINT('',(11.9094000849769,93.8,-76.1834203073561));
#59205=CARTESIAN_POINT('',(12.3425348873856,93.8,-79.0374924116092));
#59206=CARTESIAN_POINT('',(11.9094000849769,93.8,-76.1834203073561));
#59207=CARTESIAN_POINT('',(9.22113373725689,93.8,-75.1314899973787));
#59208=CARTESIAN_POINT('',(9.22113373725689,93.8,-75.1314899973787));
#59209=CARTESIAN_POINT('',(6.96600219194553,93.8,-76.9336317916543));
#59210=CARTESIAN_POINT('',(6.96600219194553,93.8,-76.9336317916543));
#59211=CARTESIAN_POINT('',(7.39913699435427,93.8,-79.7877038959074));
#59212=CARTESIAN_POINT('',(7.39913699435427,93.8,-79.7877038959074));
#59213=CARTESIAN_POINT('',(10.0874033420743,93.8,-80.8396342058848));
#59214=CARTESIAN_POINT('',(10.0874033420743,93.8,-80.8396342058848));
#59215=CARTESIAN_POINT('',(12.3425348873856,93.8,-79.0374924116092));
#59216=CARTESIAN_POINT('',(18.89372093277,93.8,-78.9164154217099));
#59217=CARTESIAN_POINT('',(19.3268557351787,93.8,-81.770487525963));
#59218=CARTESIAN_POINT('',(18.89372093277,93.8,-78.9164154217099));
#59219=CARTESIAN_POINT('',(16.20545458505,93.8,-77.8644851117325));
#59220=CARTESIAN_POINT('',(16.20545458505,93.8,-77.8644851117325));
#59221=CARTESIAN_POINT('',(13.9503230397387,93.8,-79.6666269060082));
#59222=CARTESIAN_POINT('',(13.9503230397387,93.8,-79.6666269060082));
#59223=CARTESIAN_POINT('',(14.3834578421474,93.8,-82.5206990102613));
#59224=CARTESIAN_POINT('',(14.3834578421474,93.8,-82.5206990102613));
#59225=CARTESIAN_POINT('',(17.0717241898674,93.8,-83.5726293202387));
#59226=CARTESIAN_POINT('',(17.0717241898674,93.8,-83.5726293202387));
#59227=CARTESIAN_POINT('',(19.3268557351787,93.8,-81.770487525963));
#59228=CARTESIAN_POINT('',(25.8780417805632,93.8,-81.6494105360638));
#59229=CARTESIAN_POINT('',(26.3111765829719,93.8,-84.5034826403169));
#59230=CARTESIAN_POINT('',(25.8780417805632,93.8,-81.6494105360638));
#59231=CARTESIAN_POINT('',(23.1897754328432,93.8,-80.5974802260864));
#59232=CARTESIAN_POINT('',(23.1897754328432,93.8,-80.5974802260864));
#59233=CARTESIAN_POINT('',(20.9346438875318,93.8,-82.3996220203621));
#59234=CARTESIAN_POINT('',(20.9346438875318,93.8,-82.3996220203621));
#59235=CARTESIAN_POINT('',(21.3677786899405,93.8,-85.2536941246152));
#59236=CARTESIAN_POINT('',(21.3677786899405,93.8,-85.2536941246152));
#59237=CARTESIAN_POINT('',(24.0560450376606,93.8,-86.3056244345926));
#59238=CARTESIAN_POINT('',(24.0560450376606,93.8,-86.3056244345926));
#59239=CARTESIAN_POINT('',(26.3111765829719,93.8,-84.5034826403169));
#59240=CARTESIAN_POINT('',(32.8623626283563,93.8,-84.3824056504177));
#59241=CARTESIAN_POINT('',(33.295497430765,93.8,-87.2364777546708));
#59242=CARTESIAN_POINT('',(32.8623626283563,93.8,-84.3824056504177));
#59243=CARTESIAN_POINT('',(30.1740962806363,93.8,-83.3304753404403));
#59244=CARTESIAN_POINT('',(30.1740962806363,93.8,-83.3304753404403));
#59245=CARTESIAN_POINT('',(27.9189647353249,93.8,-85.132617134716));
#59246=CARTESIAN_POINT('',(27.9189647353249,93.8,-85.132617134716));
#59247=CARTESIAN_POINT('',(28.3520995377337,93.8,-87.9866892389691));
#59248=CARTESIAN_POINT('',(28.3520995377337,93.8,-87.9866892389691));
#59249=CARTESIAN_POINT('',(31.0403658854537,93.8,-89.0386195489465));
#59250=CARTESIAN_POINT('',(31.0403658854537,93.8,-89.0386195489465));
#59251=CARTESIAN_POINT('',(33.295497430765,93.8,-87.2364777546708));
#59252=CARTESIAN_POINT('',(39.8466834761494,93.8,-87.1154007647716));
#59253=CARTESIAN_POINT('',(40.2798182785581,93.8,-89.9694728690247));
#59254=CARTESIAN_POINT('',(39.8466834761494,93.8,-87.1154007647716));
#59255=CARTESIAN_POINT('',(37.1584171284294,93.8,-86.0634704547942));
#59256=CARTESIAN_POINT('',(37.1584171284294,93.8,-86.0634704547942));
#59257=CARTESIAN_POINT('',(34.903285583118,93.8,-87.8656122490699));
#59258=CARTESIAN_POINT('',(34.903285583118,93.8,-87.8656122490699));
#59259=CARTESIAN_POINT('',(35.3364203855268,93.8,-90.719684353323));
#59260=CARTESIAN_POINT('',(35.3364203855268,93.8,-90.719684353323));
#59261=CARTESIAN_POINT('',(38.0246867332468,93.8,-91.7716146633004));
#59262=CARTESIAN_POINT('',(38.0246867332468,93.8,-91.7716146633004));
#59263=CARTESIAN_POINT('',(40.2798182785581,93.8,-89.9694728690247));
#59264=CARTESIAN_POINT('',(3.7997620107364,93.8,-66.0353283534551));
#59265=CARTESIAN_POINT('',(4.23289681314511,93.8,-68.8894004577082));
#59266=CARTESIAN_POINT('',(3.7997620107364,93.8,-66.0353283534551));
#59267=CARTESIAN_POINT('',(1.11149566301639,93.8,-64.9833980434777));
#59268=CARTESIAN_POINT('',(1.11149566301639,93.8,-64.9833980434777));
#59269=CARTESIAN_POINT('',(-1.14363588229497,93.8,-66.7855398377534));
#59270=CARTESIAN_POINT('',(-1.14363588229497,93.8,-66.7855398377534));
#59271=CARTESIAN_POINT('',(-0.710501079886239,93.8,-69.6396119420065));
#59272=CARTESIAN_POINT('',(-0.710501079886239,93.8,-69.6396119420065));
#59273=CARTESIAN_POINT('',(1.97776526783379,93.8,-70.6915422519839));
#59274=CARTESIAN_POINT('',(1.97776526783379,93.8,-70.6915422519839));
#59275=CARTESIAN_POINT('',(4.23289681314511,93.8,-68.8894004577082));
#59276=CARTESIAN_POINT('',(-3.18455883705674,93.8,-63.3023332391012));
#59277=CARTESIAN_POINT('',(-2.75142403464802,93.8,-66.1564053433543));
#59278=CARTESIAN_POINT('',(-3.18455883705674,93.8,-63.3023332391012));
#59279=CARTESIAN_POINT('',(-5.87282518477675,93.8,-62.2504029291238));
#59280=CARTESIAN_POINT('',(-5.87282518477675,93.8,-62.2504029291238));
#59281=CARTESIAN_POINT('',(-8.1279567300881,93.8,-64.0525447233995));
#59282=CARTESIAN_POINT('',(-8.1279567300881,93.8,-64.0525447233995));
#59283=CARTESIAN_POINT('',(-7.69482192767937,93.8,-66.9066168276526));
#59284=CARTESIAN_POINT('',(-7.69482192767937,93.8,-66.9066168276526));
#59285=CARTESIAN_POINT('',(-5.00655557995934,93.8,-67.95854713763));
#59286=CARTESIAN_POINT('',(-5.00655557995934,93.8,-67.95854713763));
#59287=CARTESIAN_POINT('',(-2.75142403464802,93.8,-66.1564053433543));
#59288=CARTESIAN_POINT('',(-10.1688796848499,93.8,-60.5693381247473));
#59289=CARTESIAN_POINT('',(-9.73574488244115,93.8,-63.4234102290004));
#59290=CARTESIAN_POINT('',(-10.1688796848499,93.8,-60.5693381247473));
#59291=CARTESIAN_POINT('',(-12.8571460325699,93.8,-59.5174078147699));
#59292=CARTESIAN_POINT('',(-12.8571460325699,93.8,-59.5174078147699));
#59293=CARTESIAN_POINT('',(-15.1122775778812,93.8,-61.3195496090456));
#59294=CARTESIAN_POINT('',(-15.1122775778812,93.8,-61.3195496090456));
#59295=CARTESIAN_POINT('',(-14.6791427754725,93.8,-64.1736217132987));
#59296=CARTESIAN_POINT('',(-14.6791427754725,93.8,-64.1736217132987));
#59297=CARTESIAN_POINT('',(-11.9908764277525,93.8,-65.2255520232761));
#59298=CARTESIAN_POINT('',(-11.9908764277525,93.8,-65.2255520232761));
#59299=CARTESIAN_POINT('',(-9.73574488244115,93.8,-63.4234102290004));
#59300=CARTESIAN_POINT('',(-17.153200532643,93.8,-57.8363430103935));
#59301=CARTESIAN_POINT('',(-16.7200657302343,93.8,-60.6904151146466));
#59302=CARTESIAN_POINT('',(-17.153200532643,93.8,-57.8363430103935));
#59303=CARTESIAN_POINT('',(-19.841466880363,93.8,-56.784412700416));
#59304=CARTESIAN_POINT('',(-19.841466880363,93.8,-56.784412700416));
#59305=CARTESIAN_POINT('',(-22.0965984256744,93.8,-58.5865544946917));
#59306=CARTESIAN_POINT('',(-22.0965984256744,93.8,-58.5865544946917));
#59307=CARTESIAN_POINT('',(-21.6634636232656,93.8,-61.4406265989448));
#59308=CARTESIAN_POINT('',(-21.6634636232656,93.8,-61.4406265989448));
#59309=CARTESIAN_POINT('',(-18.9751972755456,93.8,-62.4925569089222));
#59310=CARTESIAN_POINT('',(-18.9751972755456,93.8,-62.4925569089222));
#59311=CARTESIAN_POINT('',(-16.7200657302343,93.8,-60.6904151146466));
#59312=CARTESIAN_POINT('',(46.8310043239425,93.8,-89.8483958791255));
#59313=CARTESIAN_POINT('',(47.2641391263513,93.8,-92.7024679833786));
#59314=CARTESIAN_POINT('',(46.8310043239425,93.8,-89.8483958791255));
#59315=CARTESIAN_POINT('',(44.1427379762225,93.8,-88.7964655691481));
#59316=CARTESIAN_POINT('',(44.1427379762225,93.8,-88.7964655691481));
#59317=CARTESIAN_POINT('',(41.8876064309112,93.8,-90.5986073634238));
#59318=CARTESIAN_POINT('',(41.8876064309112,93.8,-90.5986073634238));
#59319=CARTESIAN_POINT('',(42.3207412333199,93.8,-93.4526794676769));
#59320=CARTESIAN_POINT('',(42.3207412333199,93.8,-93.4526794676769));
#59321=CARTESIAN_POINT('',(45.0090075810399,93.8,-94.5046097776543));
#59322=CARTESIAN_POINT('',(45.0090075810399,93.8,-94.5046097776543));
#59323=CARTESIAN_POINT('',(47.2641391263513,93.8,-92.7024679833786));
#59324=CARTESIAN_POINT('',(-38.1061630760224,93.8,-49.6373576673318));
#59325=CARTESIAN_POINT('',(-37.6730282736137,93.8,-52.4914297715849));
#59326=CARTESIAN_POINT('',(-38.1061630760224,93.8,-49.6373576673318));
#59327=CARTESIAN_POINT('',(-40.7944294237424,93.8,-48.5854273573544));
#59328=CARTESIAN_POINT('',(-40.7944294237424,93.8,-48.5854273573544));
#59329=CARTESIAN_POINT('',(-43.0495609690538,93.8,-50.3875691516301));
#59330=CARTESIAN_POINT('',(-43.0495609690538,93.8,-50.3875691516301));
#59331=CARTESIAN_POINT('',(-42.616426166645,93.8,-53.2416412558831));
#59332=CARTESIAN_POINT('',(-42.616426166645,93.8,-53.2416412558831));
#59333=CARTESIAN_POINT('',(-39.928159818925,93.8,-54.2935715658606));
#59334=CARTESIAN_POINT('',(-39.928159818925,93.8,-54.2935715658606));
#59335=CARTESIAN_POINT('',(-37.6730282736137,93.8,-52.4914297715849));
#59336=CARTESIAN_POINT('',(-31.1218422282293,93.8,-52.3703527816857));
#59337=CARTESIAN_POINT('',(-30.6887074258205,93.8,-55.2244248859388));
#59338=CARTESIAN_POINT('',(-31.1218422282293,93.8,-52.3703527816857));
#59339=CARTESIAN_POINT('',(-33.8101085759493,93.8,-51.3184224717083));
#59340=CARTESIAN_POINT('',(-33.8101085759493,93.8,-51.3184224717083));
#59341=CARTESIAN_POINT('',(-36.0652401212606,93.8,-53.120564265984));
#59342=CARTESIAN_POINT('',(-36.0652401212606,93.8,-53.120564265984));
#59343=CARTESIAN_POINT('',(-35.6321053188519,93.8,-55.974636370237));
#59344=CARTESIAN_POINT('',(-35.6321053188519,93.8,-55.974636370237));
#59345=CARTESIAN_POINT('',(-32.9438389711319,93.8,-57.0265666802144));
#59346=CARTESIAN_POINT('',(-32.9438389711319,93.8,-57.0265666802144));
#59347=CARTESIAN_POINT('',(-30.6887074258205,93.8,-55.2244248859388));
#59348=CARTESIAN_POINT('',(-24.1375213804361,93.8,-55.1033478960396));
#59349=CARTESIAN_POINT('',(-23.7043865780274,93.8,-57.9574200002927));
#59350=CARTESIAN_POINT('',(-24.1375213804361,93.8,-55.1033478960396));
#59351=CARTESIAN_POINT('',(-26.8257877281561,93.8,-54.0514175860622));
#59352=CARTESIAN_POINT('',(-26.8257877281561,93.8,-54.0514175860622));
#59353=CARTESIAN_POINT('',(-29.0809192734675,93.8,-55.8535593803378));
#59354=CARTESIAN_POINT('',(-29.0809192734675,93.8,-55.8535593803378));
#59355=CARTESIAN_POINT('',(-28.6477844710588,93.8,-58.7076314845909));
#59356=CARTESIAN_POINT('',(-28.6477844710588,93.8,-58.7076314845909));
#59357=CARTESIAN_POINT('',(-25.9595181233387,93.8,-59.7595617945683));
#59358=CARTESIAN_POINT('',(-25.9595181233387,93.8,-59.7595617945683));
#59359=CARTESIAN_POINT('',(-23.7043865780274,93.8,-57.9574200002927));
#59360=CARTESIAN_POINT('',(-23.2446216430976,93.8,-104.276030658515));
#59361=CARTESIAN_POINT('',(-22.8114868406889,93.8,-107.130102762768));
#59362=CARTESIAN_POINT('',(-23.2446216430976,93.8,-104.276030658515));
#59363=CARTESIAN_POINT('',(-25.9328879908176,93.8,-103.224100348538));
#59364=CARTESIAN_POINT('',(-25.9328879908176,93.8,-103.224100348538));
#59365=CARTESIAN_POINT('',(-28.188019536129,93.8,-105.026242142813));
#59366=CARTESIAN_POINT('',(-28.188019536129,93.8,-105.026242142813));
#59367=CARTESIAN_POINT('',(-27.7548847337203,93.8,-107.880314247066));
#59368=CARTESIAN_POINT('',(-27.7548847337203,93.8,-107.880314247066));
#59369=CARTESIAN_POINT('',(-25.0666183860002,93.8,-108.932244557044));
#59370=CARTESIAN_POINT('',(-25.0666183860002,93.8,-108.932244557044));
#59371=CARTESIAN_POINT('',(-22.8114868406889,93.8,-107.130102762768));
#59372=CARTESIAN_POINT('',(-16.2603007953045,93.8,-107.009025772869));
#59373=CARTESIAN_POINT('',(-15.8271659928958,93.8,-109.863097877122));
#59374=CARTESIAN_POINT('',(-16.2603007953045,93.8,-107.009025772869));
#59375=CARTESIAN_POINT('',(-18.9485671430245,93.8,-105.957095462892));
#59376=CARTESIAN_POINT('',(-18.9485671430245,93.8,-105.957095462892));
#59377=CARTESIAN_POINT('',(-21.2036986883359,93.8,-107.759237257167));
#59378=CARTESIAN_POINT('',(-21.2036986883359,93.8,-107.759237257167));
#59379=CARTESIAN_POINT('',(-20.7705638859271,93.8,-110.61330936142));
#59380=CARTESIAN_POINT('',(-20.7705638859271,93.8,-110.61330936142));
#59381=CARTESIAN_POINT('',(-18.0822975382071,93.8,-111.665239671398));
#59382=CARTESIAN_POINT('',(-18.0822975382071,93.8,-111.665239671398));
#59383=CARTESIAN_POINT('',(-15.8271659928958,93.8,-109.863097877122));
#59384=CARTESIAN_POINT('',(-9.27597994751136,93.8,-109.742020887223));
#59385=CARTESIAN_POINT('',(-8.84284514510264,93.8,-112.596092991476));
#59386=CARTESIAN_POINT('',(-9.27597994751136,93.8,-109.742020887223));
#59387=CARTESIAN_POINT('',(-11.9642462952314,93.8,-108.690090577245));
#59388=CARTESIAN_POINT('',(-11.9642462952314,93.8,-108.690090577245));
#59389=CARTESIAN_POINT('',(-14.2193778405427,93.8,-110.492232371521));
#59390=CARTESIAN_POINT('',(-14.2193778405427,93.8,-110.492232371521));
#59391=CARTESIAN_POINT('',(-13.786243038134,93.8,-113.346304475774));
#59392=CARTESIAN_POINT('',(-13.786243038134,93.8,-113.346304475774));
#59393=CARTESIAN_POINT('',(-11.097976690414,93.8,-114.398234785752));
#59394=CARTESIAN_POINT('',(-11.097976690414,93.8,-114.398234785752));
#59395=CARTESIAN_POINT('',(-8.84284514510264,93.8,-112.596092991476));
#59396=CARTESIAN_POINT('',(-2.29165909971822,93.8,-112.475016001577));
#59397=CARTESIAN_POINT('',(-1.85852429730951,93.8,-115.32908810583));
#59398=CARTESIAN_POINT('',(-2.29165909971822,93.8,-112.475016001577));
#59399=CARTESIAN_POINT('',(-4.97992544743824,93.8,-111.423085691599));
#59400=CARTESIAN_POINT('',(-4.97992544743824,93.8,-111.423085691599));
#59401=CARTESIAN_POINT('',(-7.23505699274959,93.8,-113.225227485875));
#59402=CARTESIAN_POINT('',(-7.23505699274959,93.8,-113.225227485875));
#59403=CARTESIAN_POINT('',(-6.80192219034086,93.8,-116.079299590128));
#59404=CARTESIAN_POINT('',(-6.80192219034086,93.8,-116.079299590128));
#59405=CARTESIAN_POINT('',(-4.11365584262083,93.8,-117.131229900105));
#59406=CARTESIAN_POINT('',(-4.11365584262083,93.8,-117.131229900105));
#59407=CARTESIAN_POINT('',(-1.85852429730951,93.8,-115.32908810583));
#59408=CARTESIAN_POINT('',(4.69266174807491,93.8,-115.208011115931));
#59409=CARTESIAN_POINT('',(5.12579655048363,93.8,-118.062083220184));
#59410=CARTESIAN_POINT('',(4.69266174807491,93.8,-115.208011115931));
#59411=CARTESIAN_POINT('',(2.0043954003549,93.8,-114.156080805953));
#59412=CARTESIAN_POINT('',(2.0043954003549,93.8,-114.156080805953));
#59413=CARTESIAN_POINT('',(-0.250736144956458,93.8,-115.958222600229));
#59414=CARTESIAN_POINT('',(-0.250736144956458,93.8,-115.958222600229));
#59415=CARTESIAN_POINT('',(0.182398657452273,93.8,-118.812294704482));
#59416=CARTESIAN_POINT('',(0.182398657452273,93.8,-118.812294704482));
#59417=CARTESIAN_POINT('',(2.8706650051723,93.8,-119.864225014459));
#59418=CARTESIAN_POINT('',(2.8706650051723,93.8,-119.864225014459));
#59419=CARTESIAN_POINT('',(5.12579655048363,93.8,-118.062083220184));
#59420=CARTESIAN_POINT('',(11.676982595868,93.8,-117.941006230285));
#59421=CARTESIAN_POINT('',(12.1101173982768,93.8,-120.795078334538));
#59422=CARTESIAN_POINT('',(11.676982595868,93.8,-117.941006230285));
#59423=CARTESIAN_POINT('',(8.98871624814803,93.8,-116.889075920307));
#59424=CARTESIAN_POINT('',(8.98871624814803,93.8,-116.889075920307));
#59425=CARTESIAN_POINT('',(6.73358470283667,93.8,-118.691217714583));
#59426=CARTESIAN_POINT('',(6.73358470283667,93.8,-118.691217714583));
#59427=CARTESIAN_POINT('',(7.1667195052454,93.8,-121.545289818836));
#59428=CARTESIAN_POINT('',(7.1667195052454,93.8,-121.545289818836));
#59429=CARTESIAN_POINT('',(9.85498585296543,93.8,-122.597220128813));
#59430=CARTESIAN_POINT('',(9.85498585296543,93.8,-122.597220128813));
#59431=CARTESIAN_POINT('',(12.1101173982768,93.8,-120.795078334538));
#59432=CARTESIAN_POINT('',(18.6613034436612,93.8,-120.674001344638));
#59433=CARTESIAN_POINT('',(19.0944382460699,93.8,-123.528073448892));
#59434=CARTESIAN_POINT('',(18.6613034436612,93.8,-120.674001344638));
#59435=CARTESIAN_POINT('',(15.9730370959412,93.8,-119.622071034661));
#59436=CARTESIAN_POINT('',(15.9730370959412,93.8,-119.622071034661));
#59437=CARTESIAN_POINT('',(13.7179055506298,93.8,-121.424212828937));
#59438=CARTESIAN_POINT('',(13.7179055506298,93.8,-121.424212828937));
#59439=CARTESIAN_POINT('',(14.1510403530385,93.8,-124.27828493319));
#59440=CARTESIAN_POINT('',(14.1510403530385,93.8,-124.27828493319));
#59441=CARTESIAN_POINT('',(16.8393067007586,93.8,-125.330215243167));
#59442=CARTESIAN_POINT('',(16.8393067007586,93.8,-125.330215243167));
#59443=CARTESIAN_POINT('',(19.0944382460699,93.8,-123.528073448892));
#59444=CARTESIAN_POINT('',(25.6456242914543,93.8,-123.406996458992));
#59445=CARTESIAN_POINT('',(26.078759093863,93.8,-126.261068563245));
#59446=CARTESIAN_POINT('',(25.6456242914543,93.8,-123.406996458992));
#59447=CARTESIAN_POINT('',(22.9573579437343,93.8,-122.355066149015));
#59448=CARTESIAN_POINT('',(22.9573579437343,93.8,-122.355066149015));
#59449=CARTESIAN_POINT('',(20.7022263984229,93.8,-124.157207943291));
#59450=CARTESIAN_POINT('',(20.7022263984229,93.8,-124.157207943291));
#59451=CARTESIAN_POINT('',(21.1353612008317,93.8,-127.011280047544));
#59452=CARTESIAN_POINT('',(21.1353612008317,93.8,-127.011280047544));
#59453=CARTESIAN_POINT('',(23.8236275485517,93.8,-128.063210357521));
#59454=CARTESIAN_POINT('',(23.8236275485517,93.8,-128.063210357521));
#59455=CARTESIAN_POINT('',(26.078759093863,93.8,-126.261068563245));
#59456=CARTESIAN_POINT('',(-45.3229014129244,93.8,-88.6619484759063));
#59457=CARTESIAN_POINT('',(-44.8897666105157,93.8,-91.5160205801594));
#59458=CARTESIAN_POINT('',(-45.3229014129244,93.8,-88.6619484759063));
#59459=CARTESIAN_POINT('',(-48.0111677606444,93.8,-87.6100181659289));
#59460=CARTESIAN_POINT('',(-48.0111677606444,93.8,-87.6100181659289));
#59461=CARTESIAN_POINT('',(-50.2662993059558,93.8,-89.4121599602046));
#59462=CARTESIAN_POINT('',(-50.2662993059558,93.8,-89.4121599602046));
#59463=CARTESIAN_POINT('',(-49.833164503547,93.8,-92.2662320644577));
#59464=CARTESIAN_POINT('',(-49.833164503547,93.8,-92.2662320644577));
#59465=CARTESIAN_POINT('',(-47.144898155827,93.8,-93.3181623744351));
#59466=CARTESIAN_POINT('',(-47.144898155827,93.8,-93.3181623744351));
#59467=CARTESIAN_POINT('',(-44.8897666105157,93.8,-91.5160205801594));
#59468=CARTESIAN_POINT('',(-38.3385805651313,93.8,-91.3949435902602));
#59469=CARTESIAN_POINT('',(-37.9054457627226,93.8,-94.2490156945133));
#59470=CARTESIAN_POINT('',(-38.3385805651313,93.8,-91.3949435902602));
#59471=CARTESIAN_POINT('',(-41.0268469128513,93.8,-90.3430132802828));
#59472=CARTESIAN_POINT('',(-41.0268469128513,93.8,-90.3430132802828));
#59473=CARTESIAN_POINT('',(-43.2819784581626,93.8,-92.1451550745585));
#59474=CARTESIAN_POINT('',(-43.2819784581626,93.8,-92.1451550745585));
#59475=CARTESIAN_POINT('',(-42.8488436557539,93.8,-94.9992271788116));
#59476=CARTESIAN_POINT('',(-42.8488436557539,93.8,-94.9992271788116));
#59477=CARTESIAN_POINT('',(-40.1605773080339,93.8,-96.051157488789));
#59478=CARTESIAN_POINT('',(-40.1605773080339,93.8,-96.051157488789));
#59479=CARTESIAN_POINT('',(-37.9054457627226,93.8,-94.2490156945133));
#59480=CARTESIAN_POINT('',(-31.3542597173381,93.8,-94.1279387046141));
#59481=CARTESIAN_POINT('',(-30.9211249149294,93.8,-96.9820108088672));
#59482=CARTESIAN_POINT('',(-31.3542597173381,93.8,-94.1279387046141));
#59483=CARTESIAN_POINT('',(-34.0425260650581,93.8,-93.0760083946367));
#59484=CARTESIAN_POINT('',(-34.0425260650581,93.8,-93.0760083946367));
#59485=CARTESIAN_POINT('',(-36.2976576103695,93.8,-94.8781501889124));
#59486=CARTESIAN_POINT('',(-36.2976576103695,93.8,-94.8781501889124));
#59487=CARTESIAN_POINT('',(-35.8645228079608,93.8,-97.7322222931655));
#59488=CARTESIAN_POINT('',(-35.8645228079608,93.8,-97.7322222931655));
#59489=CARTESIAN_POINT('',(-33.1762564602408,93.8,-98.7841526031429));
#59490=CARTESIAN_POINT('',(-33.1762564602408,93.8,-98.7841526031429));
#59491=CARTESIAN_POINT('',(-30.9211249149294,93.8,-96.9820108088672));
#59492=CARTESIAN_POINT('',(-24.369938869545,93.8,-96.860933818968));
#59493=CARTESIAN_POINT('',(-23.9368040671363,93.8,-99.7150059232211));
#59494=CARTESIAN_POINT('',(-24.369938869545,93.8,-96.860933818968));
#59495=CARTESIAN_POINT('',(-27.058205217265,93.8,-95.8090035089906));
#59496=CARTESIAN_POINT('',(-27.058205217265,93.8,-95.8090035089906));
#59497=CARTESIAN_POINT('',(-29.3133367625764,93.8,-97.6111453032663));
#59498=CARTESIAN_POINT('',(-29.3133367625764,93.8,-97.6111453032663));
#59499=CARTESIAN_POINT('',(-28.8802019601676,93.8,-100.465217407519));
#59500=CARTESIAN_POINT('',(-28.8802019601676,93.8,-100.465217407519));
#59501=CARTESIAN_POINT('',(-26.1919356124476,93.8,-101.517147717497));
#59502=CARTESIAN_POINT('',(-26.1919356124476,93.8,-101.517147717497));
#59503=CARTESIAN_POINT('',(-23.9368040671363,93.8,-99.7150059232211));
#59504=CARTESIAN_POINT('',(-17.3856180217519,93.8,-99.5939289333219));
#59505=CARTESIAN_POINT('',(-16.9524832193432,93.8,-102.448001037575));
#59506=CARTESIAN_POINT('',(-17.3856180217519,93.8,-99.5939289333219));
#59507=CARTESIAN_POINT('',(-20.0738843694719,93.8,-98.5419986233445));
#59508=CARTESIAN_POINT('',(-20.0738843694719,93.8,-98.5419986233445));
#59509=CARTESIAN_POINT('',(-22.3290159147832,93.8,-100.34414041762));
#59510=CARTESIAN_POINT('',(-22.3290159147832,93.8,-100.34414041762));
#59511=CARTESIAN_POINT('',(-21.8958811123745,93.8,-103.198212521873));
#59512=CARTESIAN_POINT('',(-21.8958811123745,93.8,-103.198212521873));
#59513=CARTESIAN_POINT('',(-19.2076147646545,93.8,-104.250142831851));
#59514=CARTESIAN_POINT('',(-19.2076147646545,93.8,-104.250142831851));
#59515=CARTESIAN_POINT('',(-16.9524832193432,93.8,-102.448001037575));
#59516=CARTESIAN_POINT('',(-10.4012971739587,93.8,-102.326924047676));
#59517=CARTESIAN_POINT('',(-9.96816237155003,93.8,-105.180996151929));
#59518=CARTESIAN_POINT('',(-10.4012971739587,93.8,-102.326924047676));
#59519=CARTESIAN_POINT('',(-13.0895635216788,93.8,-101.274993737698));
#59520=CARTESIAN_POINT('',(-13.0895635216788,93.8,-101.274993737698));
#59521=CARTESIAN_POINT('',(-15.3446950669901,93.8,-103.077135531974));
#59522=CARTESIAN_POINT('',(-15.3446950669901,93.8,-103.077135531974));
#59523=CARTESIAN_POINT('',(-14.9115602645814,93.8,-105.931207636227));
#59524=CARTESIAN_POINT('',(-14.9115602645814,93.8,-105.931207636227));
#59525=CARTESIAN_POINT('',(-12.2232939168614,93.8,-106.983137946205));
#59526=CARTESIAN_POINT('',(-12.2232939168614,93.8,-106.983137946205));
#59527=CARTESIAN_POINT('',(-9.96816237155003,93.8,-105.180996151929));
#59528=CARTESIAN_POINT('',(-3.41697632616561,93.8,-105.05991916203));
#59529=CARTESIAN_POINT('',(-2.9838415237569,93.8,-107.913991266283));
#59530=CARTESIAN_POINT('',(-3.41697632616561,93.8,-105.05991916203));
#59531=CARTESIAN_POINT('',(-6.10524267388563,93.8,-104.007988852052));
#59532=CARTESIAN_POINT('',(-6.10524267388563,93.8,-104.007988852052));
#59533=CARTESIAN_POINT('',(-8.36037421919698,93.8,-105.810130646328));
#59534=CARTESIAN_POINT('',(-8.36037421919698,93.8,-105.810130646328));
#59535=CARTESIAN_POINT('',(-7.92723941678825,93.8,-108.664202750581));
#59536=CARTESIAN_POINT('',(-7.92723941678825,93.8,-108.664202750581));
#59537=CARTESIAN_POINT('',(-5.23897306906822,93.8,-109.716133060558));
#59538=CARTESIAN_POINT('',(-5.23897306906822,93.8,-109.716133060558));
#59539=CARTESIAN_POINT('',(-2.9838415237569,93.8,-107.913991266283));
#59540=CARTESIAN_POINT('',(3.56734452162752,93.8,-107.792914276384));
#59541=CARTESIAN_POINT('',(4.00047932403623,93.8,-110.646986380637));
#59542=CARTESIAN_POINT('',(3.56734452162752,93.8,-107.792914276384));
#59543=CARTESIAN_POINT('',(0.879078173907508,93.8,-106.740983966406));
#59544=CARTESIAN_POINT('',(0.879078173907508,93.8,-106.740983966406));
#59545=CARTESIAN_POINT('',(-1.37605337140385,93.8,-108.543125760682));
#59546=CARTESIAN_POINT('',(-1.37605337140385,93.8,-108.543125760682));
#59547=CARTESIAN_POINT('',(-0.942918568995116,93.8,-111.397197864935));
#59548=CARTESIAN_POINT('',(-0.942918568995116,93.8,-111.397197864935));
#59549=CARTESIAN_POINT('',(1.74534777872491,93.8,-112.449128174912));
#59550=CARTESIAN_POINT('',(1.74534777872491,93.8,-112.449128174912));
#59551=CARTESIAN_POINT('',(4.00047932403624,93.8,-110.646986380637));
#59552=CARTESIAN_POINT('',(-20.9939871902029,93.8,-119.106224337609));
#59553=CARTESIAN_POINT('',(-20.5608523877941,93.8,-121.960296441862));
#59554=CARTESIAN_POINT('',(-20.9939871902029,93.8,-119.106224337609));
#59555=CARTESIAN_POINT('',(-23.6822535379229,93.8,-118.054294027632));
#59556=CARTESIAN_POINT('',(-23.6822535379229,93.8,-118.054294027632));
#59557=CARTESIAN_POINT('',(-25.9373850832342,93.8,-119.856435821907));
#59558=CARTESIAN_POINT('',(-25.9373850832342,93.8,-119.856435821907));
#59559=CARTESIAN_POINT('',(-25.5042502808255,93.8,-122.710507926161));
#59560=CARTESIAN_POINT('',(-25.5042502808255,93.8,-122.710507926161));
#59561=CARTESIAN_POINT('',(-22.8159839331055,93.8,-123.762438236138));
#59562=CARTESIAN_POINT('',(-22.8159839331055,93.8,-123.762438236138));
#59563=CARTESIAN_POINT('',(-20.5608523877941,93.8,-121.960296441862));
#59564=CARTESIAN_POINT('',(-14.0096663424097,93.8,-121.839219451963));
#59565=CARTESIAN_POINT('',(-13.576531540001,93.8,-124.693291556216));
#59566=CARTESIAN_POINT('',(-14.0096663424097,93.8,-121.839219451963));
#59567=CARTESIAN_POINT('',(-16.6979326901297,93.8,-120.787289141986));
#59568=CARTESIAN_POINT('',(-16.6979326901297,93.8,-120.787289141986));
#59569=CARTESIAN_POINT('',(-18.9530642354411,93.8,-122.589430936261));
#59570=CARTESIAN_POINT('',(-18.9530642354411,93.8,-122.589430936261));
#59571=CARTESIAN_POINT('',(-18.5199294330324,93.8,-125.443503040514));
#59572=CARTESIAN_POINT('',(-18.5199294330324,93.8,-125.443503040514));
#59573=CARTESIAN_POINT('',(-15.8316630853123,93.8,-126.495433350492));
#59574=CARTESIAN_POINT('',(-15.8316630853123,93.8,-126.495433350492));
#59575=CARTESIAN_POINT('',(-13.576531540001,93.8,-124.693291556216));
#59576=CARTESIAN_POINT('',(-7.02534549461661,93.8,-124.572214566317));
#59577=CARTESIAN_POINT('',(-6.59221069220789,93.8,-127.42628667057));
#59578=CARTESIAN_POINT('',(-7.02534549461661,93.8,-124.572214566317));
#59579=CARTESIAN_POINT('',(-9.71361184233662,93.8,-123.52028425634));
#59580=CARTESIAN_POINT('',(-9.71361184233662,93.8,-123.52028425634));
#59581=CARTESIAN_POINT('',(-11.968743387648,93.8,-125.322426050615));
#59582=CARTESIAN_POINT('',(-11.968743387648,93.8,-125.322426050615));
#59583=CARTESIAN_POINT('',(-11.5356085852392,93.8,-128.176498154868));
#59584=CARTESIAN_POINT('',(-11.5356085852392,93.8,-128.176498154868));
#59585=CARTESIAN_POINT('',(-8.84734223751921,93.8,-129.228428464846));
#59586=CARTESIAN_POINT('',(-8.84734223751921,93.8,-129.228428464846));
#59587=CARTESIAN_POINT('',(-6.59221069220789,93.8,-127.42628667057));
#59588=CARTESIAN_POINT('',(-0.0410246468234739,93.8,-127.305209680671));
#59589=CARTESIAN_POINT('',(0.392110155585244,93.8,-130.159281784924));
#59590=CARTESIAN_POINT('',(-0.0410246468234739,93.8,-127.305209680671));
#59591=CARTESIAN_POINT('',(-2.72929099454348,93.8,-126.253279370693));
#59592=CARTESIAN_POINT('',(-2.72929099454348,93.8,-126.253279370693));
#59593=CARTESIAN_POINT('',(-4.98442253985484,93.8,-128.055421164969));
#59594=CARTESIAN_POINT('',(-4.98442253985484,93.8,-128.055421164969));
#59595=CARTESIAN_POINT('',(-4.55128773744611,93.8,-130.909493269222));
#59596=CARTESIAN_POINT('',(-4.55128773744611,93.8,-130.909493269222));
#59597=CARTESIAN_POINT('',(-1.86302138972608,93.8,-131.9614235792));
#59598=CARTESIAN_POINT('',(-1.86302138972608,93.8,-131.9614235792));
#59599=CARTESIAN_POINT('',(0.392110155585244,93.8,-130.159281784924));
#59600=CARTESIAN_POINT('',(-43.0722669600296,93.8,-103.492142155));
#59601=CARTESIAN_POINT('',(-42.6391321576209,93.8,-106.346214259254));
#59602=CARTESIAN_POINT('',(-43.0722669600296,93.8,-103.492142155));
#59603=CARTESIAN_POINT('',(-45.7605333077496,93.8,-102.440211845023));
#59604=CARTESIAN_POINT('',(-45.7605333077496,93.8,-102.440211845023));
#59605=CARTESIAN_POINT('',(-48.015664853061,93.8,-104.242353639299));
#59606=CARTESIAN_POINT('',(-48.015664853061,93.8,-104.242353639299));
#59607=CARTESIAN_POINT('',(-47.5825300506523,93.8,-107.096425743552));
#59608=CARTESIAN_POINT('',(-47.5825300506523,93.8,-107.096425743552));
#59609=CARTESIAN_POINT('',(-44.8942637029322,93.8,-108.148356053529));
#59610=CARTESIAN_POINT('',(-44.8942637029322,93.8,-108.148356053529));
#59611=CARTESIAN_POINT('',(-42.6391321576209,93.8,-106.346214259254));
#59612=CARTESIAN_POINT('',(-36.0879461122365,93.8,-106.225137269354));
#59613=CARTESIAN_POINT('',(-35.6548113098278,93.8,-109.079209373607));
#59614=CARTESIAN_POINT('',(-36.0879461122365,93.8,-106.225137269354));
#59615=CARTESIAN_POINT('',(-38.7762124599565,93.8,-105.173206959377));
#59616=CARTESIAN_POINT('',(-38.7762124599565,93.8,-105.173206959377));
#59617=CARTESIAN_POINT('',(-41.0313440052679,93.8,-106.975348753653));
#59618=CARTESIAN_POINT('',(-41.0313440052679,93.8,-106.975348753653));
#59619=CARTESIAN_POINT('',(-40.5982092028591,93.8,-109.829420857906));
#59620=CARTESIAN_POINT('',(-40.5982092028591,93.8,-109.829420857906));
#59621=CARTESIAN_POINT('',(-37.9099428551391,93.8,-110.881351167883));
#59622=CARTESIAN_POINT('',(-37.9099428551391,93.8,-110.881351167883));
#59623=CARTESIAN_POINT('',(-35.6548113098278,93.8,-109.079209373607));
#59624=CARTESIAN_POINT('',(-29.1036252644434,93.8,-108.958132383708));
#59625=CARTESIAN_POINT('',(-28.6704904620346,93.8,-111.812204487961));
#59626=CARTESIAN_POINT('',(-29.1036252644434,93.8,-108.958132383708));
#59627=CARTESIAN_POINT('',(-31.7918916121634,93.8,-107.906202073731));
#59628=CARTESIAN_POINT('',(-31.7918916121634,93.8,-107.906202073731));
#59629=CARTESIAN_POINT('',(-34.0470231574747,93.8,-109.708343868006));
#59630=CARTESIAN_POINT('',(-34.0470231574747,93.8,-109.708343868006));
#59631=CARTESIAN_POINT('',(-33.613888355066,93.8,-112.56241597226));
#59632=CARTESIAN_POINT('',(-33.613888355066,93.8,-112.56241597226));
#59633=CARTESIAN_POINT('',(-30.925622007346,93.8,-113.614346282237));
#59634=CARTESIAN_POINT('',(-30.925622007346,93.8,-113.614346282237));
#59635=CARTESIAN_POINT('',(-28.6704904620347,93.8,-111.812204487961));
#59636=CARTESIAN_POINT('',(-22.1193044166502,93.8,-111.691127498062));
#59637=CARTESIAN_POINT('',(-21.6861696142415,93.8,-114.545199602315));
#59638=CARTESIAN_POINT('',(-22.1193044166502,93.8,-111.691127498062));
#59639=CARTESIAN_POINT('',(-24.8075707643703,93.8,-110.639197188085));
#59640=CARTESIAN_POINT('',(-24.8075707643703,93.8,-110.639197188085));
#59641=CARTESIAN_POINT('',(-27.0627023096816,93.8,-112.44133898236));
#59642=CARTESIAN_POINT('',(-27.0627023096816,93.8,-112.44133898236));
#59643=CARTESIAN_POINT('',(-26.6295675072729,93.8,-115.295411086613));
#59644=CARTESIAN_POINT('',(-26.6295675072729,93.8,-115.295411086613));
#59645=CARTESIAN_POINT('',(-23.9413011595528,93.8,-116.347341396591));
#59646=CARTESIAN_POINT('',(-23.9413011595528,93.8,-116.347341396591));
#59647=CARTESIAN_POINT('',(-21.6861696142415,93.8,-114.545199602315));
#59648=CARTESIAN_POINT('',(12.8022998223154,93.8,-125.356103069832));
#59649=CARTESIAN_POINT('',(13.2354346247241,93.8,-128.210175174085));
#59650=CARTESIAN_POINT('',(12.8022998223154,93.8,-125.356103069832));
#59651=CARTESIAN_POINT('',(10.1140334745954,93.8,-124.304172759854));
#59652=CARTESIAN_POINT('',(10.1140334745954,93.8,-124.304172759854));
#59653=CARTESIAN_POINT('',(7.85890192928405,93.8,-126.10631455413));
#59654=CARTESIAN_POINT('',(7.85890192928405,93.8,-126.10631455413));
#59655=CARTESIAN_POINT('',(8.29203673169278,93.8,-128.960386658383));
#59656=CARTESIAN_POINT('',(8.29203673169278,93.8,-128.960386658383));
#59657=CARTESIAN_POINT('',(10.9803030794128,93.8,-130.01231696836));
#59658=CARTESIAN_POINT('',(10.9803030794128,93.8,-130.01231696836));
#59659=CARTESIAN_POINT('',(13.2354346247241,93.8,-128.210175174085));
#59660=CARTESIAN_POINT('',(-44.197584186477,93.8,-96.0770453154534));
#59661=CARTESIAN_POINT('',(-43.7644493840683,93.8,-98.9311174197065));
#59662=CARTESIAN_POINT('',(-44.197584186477,93.8,-96.0770453154534));
#59663=CARTESIAN_POINT('',(-46.885850534197,93.8,-95.025115005476));
#59664=CARTESIAN_POINT('',(-46.885850534197,93.8,-95.025115005476));
#59665=CARTESIAN_POINT('',(-49.1409820795084,93.8,-96.8272567997517));
#59666=CARTESIAN_POINT('',(-49.1409820795084,93.8,-96.8272567997517));
#59667=CARTESIAN_POINT('',(-48.7078472770996,93.8,-99.6813289040047));
#59668=CARTESIAN_POINT('',(-48.7078472770996,93.8,-99.6813289040047));
#59669=CARTESIAN_POINT('',(-46.0195809293796,93.8,-100.733259213982));
#59670=CARTESIAN_POINT('',(-46.0195809293796,93.8,-100.733259213982));
#59671=CARTESIAN_POINT('',(-43.7644493840683,93.8,-98.9311174197065));
#59672=CARTESIAN_POINT('',(-37.2132633386839,93.8,-98.8100404298073));
#59673=CARTESIAN_POINT('',(-36.7801285362752,93.8,-101.66411253406));
#59674=CARTESIAN_POINT('',(-37.2132633386839,93.8,-98.8100404298073));
#59675=CARTESIAN_POINT('',(-39.9015296864039,93.8,-97.7581101198299));
#59676=CARTESIAN_POINT('',(-39.9015296864039,93.8,-97.7581101198299));
#59677=CARTESIAN_POINT('',(-42.1566612317152,93.8,-99.5602519141056));
#59678=CARTESIAN_POINT('',(-42.1566612317152,93.8,-99.5602519141056));
#59679=CARTESIAN_POINT('',(-41.7235264293065,93.8,-102.414324018359));
#59680=CARTESIAN_POINT('',(-41.7235264293065,93.8,-102.414324018359));
#59681=CARTESIAN_POINT('',(-39.0352600815865,93.8,-103.466254328336));
#59682=CARTESIAN_POINT('',(-39.0352600815865,93.8,-103.466254328336));
#59683=CARTESIAN_POINT('',(-36.7801285362752,93.8,-101.66411253406));
#59684=CARTESIAN_POINT('',(-30.2289424908907,93.8,-101.543035544161));
#59685=CARTESIAN_POINT('',(-29.795807688482,93.8,-104.397107648414));
#59686=CARTESIAN_POINT('',(-30.2289424908907,93.8,-101.543035544161));
#59687=CARTESIAN_POINT('',(-32.9172088386108,93.8,-100.491105234184));
#59688=CARTESIAN_POINT('',(-32.9172088386108,93.8,-100.491105234184));
#59689=CARTESIAN_POINT('',(-35.1723403839221,93.8,-102.293247028459));
#59690=CARTESIAN_POINT('',(-35.1723403839221,93.8,-102.293247028459));
#59691=CARTESIAN_POINT('',(-34.7392055815134,93.8,-105.147319132713));
#59692=CARTESIAN_POINT('',(-34.7392055815134,93.8,-105.147319132713));
#59693=CARTESIAN_POINT('',(-32.0509392337934,93.8,-106.19924944269));
#59694=CARTESIAN_POINT('',(-32.0509392337934,93.8,-106.19924944269));
#59695=CARTESIAN_POINT('',(-29.795807688482,93.8,-104.397107648414));
#59696=CARTESIAN_POINT('',(5.81797897452228,93.8,-122.623107955478));
#59697=CARTESIAN_POINT('',(6.251113776931,93.8,-125.477180059731));
#59698=CARTESIAN_POINT('',(5.81797897452228,93.8,-122.623107955478));
#59699=CARTESIAN_POINT('',(3.12971262680227,93.8,-121.5711776455));
#59700=CARTESIAN_POINT('',(3.12971262680227,93.8,-121.5711776455));
#59701=CARTESIAN_POINT('',(0.874581081490917,93.8,-123.373319439776));
#59702=CARTESIAN_POINT('',(0.874581081490917,93.8,-123.373319439776));
#59703=CARTESIAN_POINT('',(1.30771588389965,93.8,-126.227391544029));
#59704=CARTESIAN_POINT('',(1.30771588389965,93.8,-126.227391544029));
#59705=CARTESIAN_POINT('',(3.99598223161968,93.8,-127.279321854006));
#59706=CARTESIAN_POINT('',(3.99598223161968,93.8,-127.279321854006));
#59707=CARTESIAN_POINT('',(6.251113776931,93.8,-125.477180059731));
#59708=CARTESIAN_POINT('',(-1.16634187327085,93.8,-119.890112841124));
#59709=CARTESIAN_POINT('',(-0.733207070862132,93.8,-122.744184945377));
#59710=CARTESIAN_POINT('',(-1.16634187327085,93.8,-119.890112841124));
#59711=CARTESIAN_POINT('',(-3.85460822099086,93.8,-118.838182531146));
#59712=CARTESIAN_POINT('',(-3.85460822099086,93.8,-118.838182531146));
#59713=CARTESIAN_POINT('',(-6.10973976630222,93.8,-120.640324325422));
#59714=CARTESIAN_POINT('',(-6.10973976630222,93.8,-120.640324325422));
#59715=CARTESIAN_POINT('',(-5.67660496389348,93.8,-123.494396429675));
#59716=CARTESIAN_POINT('',(-5.67660496389348,93.8,-123.494396429675));
#59717=CARTESIAN_POINT('',(-2.98833861617346,93.8,-124.546326739653));
#59718=CARTESIAN_POINT('',(-2.98833861617346,93.8,-124.546326739653));
#59719=CARTESIAN_POINT('',(-0.733207070862132,93.8,-122.744184945377));
#59720=CARTESIAN_POINT('',(-8.15066272106398,93.8,-117.15711772677));
#59721=CARTESIAN_POINT('',(-7.71752791865526,93.8,-120.011189831023));
#59722=CARTESIAN_POINT('',(-8.15066272106398,93.8,-117.15711772677));
#59723=CARTESIAN_POINT('',(-10.838929068784,93.8,-116.105187416792));
#59724=CARTESIAN_POINT('',(-10.838929068784,93.8,-116.105187416792));
#59725=CARTESIAN_POINT('',(-13.0940606140953,93.8,-117.907329211068));
#59726=CARTESIAN_POINT('',(-13.0940606140953,93.8,-117.907329211068));
#59727=CARTESIAN_POINT('',(-12.6609258116866,93.8,-120.761401315321));
#59728=CARTESIAN_POINT('',(-12.6609258116866,93.8,-120.761401315321));
#59729=CARTESIAN_POINT('',(-9.97265946396659,93.8,-121.813331625299));
#59730=CARTESIAN_POINT('',(-9.97265946396659,93.8,-121.813331625299));
#59731=CARTESIAN_POINT('',(-7.71752791865526,93.8,-120.011189831023));
#59732=CARTESIAN_POINT('',(-15.1349835688571,93.8,-114.424122612416));
#59733=CARTESIAN_POINT('',(-14.7018487664484,93.8,-117.278194716669));
#59734=CARTESIAN_POINT('',(-15.1349835688571,93.8,-114.424122612416));
#59735=CARTESIAN_POINT('',(-17.8232499165771,93.8,-113.372192302439));
#59736=CARTESIAN_POINT('',(-17.8232499165771,93.8,-113.372192302439));
#59737=CARTESIAN_POINT('',(-20.0783814618885,93.8,-115.174334096714));
#59738=CARTESIAN_POINT('',(-20.0783814618885,93.8,-115.174334096714));
#59739=CARTESIAN_POINT('',(-19.6452466594797,93.8,-118.028406200967));
#59740=CARTESIAN_POINT('',(-19.6452466594797,93.8,-118.028406200967));
#59741=CARTESIAN_POINT('',(-16.9569803117597,93.8,-119.080336510945));
#59742=CARTESIAN_POINT('',(-16.9569803117597,93.8,-119.080336510945));
#59743=CARTESIAN_POINT('',(-14.7018487664484,93.8,-117.278194716669));
#59744=CARTESIAN_POINT('',(-5.66761077906036,93.8,-90.2297254829355));
#59745=CARTESIAN_POINT('',(-5.23447597665164,93.8,-93.0837975871887));
#59746=CARTESIAN_POINT('',(-5.66761077906036,93.8,-90.2297254829355));
#59747=CARTESIAN_POINT('',(-8.35587712678037,93.8,-89.1777951729581));
#59748=CARTESIAN_POINT('',(-8.35587712678037,93.8,-89.1777951729581));
#59749=CARTESIAN_POINT('',(-10.6110086720917,93.8,-90.9799369672338));
#59750=CARTESIAN_POINT('',(-10.6110086720917,93.8,-90.9799369672338));
#59751=CARTESIAN_POINT('',(-10.177873869683,93.8,-93.8340090714869));
#59752=CARTESIAN_POINT('',(-10.177873869683,93.8,-93.8340090714869));
#59753=CARTESIAN_POINT('',(-7.48960752196297,93.8,-94.8859393814643));
#59754=CARTESIAN_POINT('',(-7.48960752196297,93.8,-94.8859393814643));
#59755=CARTESIAN_POINT('',(-5.23447597665164,93.8,-93.0837975871887));
#59756=CARTESIAN_POINT('',(-12.6519316268535,93.8,-87.4967303685817));
#59757=CARTESIAN_POINT('',(-12.2187968244448,93.8,-90.3508024728348));
#59758=CARTESIAN_POINT('',(-12.6519316268535,93.8,-87.4967303685817));
#59759=CARTESIAN_POINT('',(-15.3401979745735,93.8,-86.4448000586042));
#59760=CARTESIAN_POINT('',(-15.3401979745735,93.8,-86.4448000586042));
#59761=CARTESIAN_POINT('',(-17.5953295198849,93.8,-88.2469418528799));
#59762=CARTESIAN_POINT('',(-17.5953295198849,93.8,-88.2469418528799));
#59763=CARTESIAN_POINT('',(-17.1621947174761,93.8,-91.101013957133));
#59764=CARTESIAN_POINT('',(-17.1621947174761,93.8,-91.101013957133));
#59765=CARTESIAN_POINT('',(-14.4739283697561,93.8,-92.1529442671104));
#59766=CARTESIAN_POINT('',(-14.4739283697561,93.8,-92.1529442671104));
#59767=CARTESIAN_POINT('',(-12.2187968244448,93.8,-90.3508024728348));
#59768=CARTESIAN_POINT('',(-19.6362524746466,93.8,-84.7637352542278));
#59769=CARTESIAN_POINT('',(-19.2031176722379,93.8,-87.6178073584809));
#59770=CARTESIAN_POINT('',(-19.6362524746466,93.8,-84.7637352542278));
#59771=CARTESIAN_POINT('',(-22.3245188223666,93.8,-83.7118049442504));
#59772=CARTESIAN_POINT('',(-22.3245188223666,93.8,-83.7118049442504));
#59773=CARTESIAN_POINT('',(-24.579650367678,93.8,-85.5139467385261));
#59774=CARTESIAN_POINT('',(-24.579650367678,93.8,-85.5139467385261));
#59775=CARTESIAN_POINT('',(-24.1465155652693,93.8,-88.3680188427791));
#59776=CARTESIAN_POINT('',(-24.1465155652693,93.8,-88.3680188427791));
#59777=CARTESIAN_POINT('',(-21.4582492175492,93.8,-89.4199491527566));
#59778=CARTESIAN_POINT('',(-21.4582492175492,93.8,-89.4199491527566));
#59779=CARTESIAN_POINT('',(-19.2031176722379,93.8,-87.6178073584809));
#59780=CARTESIAN_POINT('',(-26.6205733224398,93.8,-82.0307401398739));
#59781=CARTESIAN_POINT('',(-26.187438520031,93.8,-84.884812244127));
#59782=CARTESIAN_POINT('',(-26.6205733224398,93.8,-82.0307401398739));
#59783=CARTESIAN_POINT('',(-29.3088396701598,93.8,-80.9788098298965));
#59784=CARTESIAN_POINT('',(-29.3088396701598,93.8,-80.9788098298965));
#59785=CARTESIAN_POINT('',(-31.5639712154711,93.8,-82.7809516241722));
#59786=CARTESIAN_POINT('',(-31.5639712154711,93.8,-82.7809516241722));
#59787=CARTESIAN_POINT('',(-31.1308364130624,93.8,-85.6350237284252));
#59788=CARTESIAN_POINT('',(-31.1308364130624,93.8,-85.6350237284252));
#59789=CARTESIAN_POINT('',(-28.4425700653424,93.8,-86.6869540384027));
#59790=CARTESIAN_POINT('',(-28.4425700653424,93.8,-86.6869540384027));
#59791=CARTESIAN_POINT('',(-26.187438520031,93.8,-84.884812244127));
#59792=CARTESIAN_POINT('',(37.3636315341458,93.8,-114.042793008606));
#59793=CARTESIAN_POINT('',(37.7967663365545,93.8,-116.896865112859));
#59794=CARTESIAN_POINT('',(37.3636315341458,93.8,-114.042793008606));
#59795=CARTESIAN_POINT('',(34.6753651864258,93.8,-112.990862698629));
#59796=CARTESIAN_POINT('',(34.6753651864258,93.8,-112.990862698629));
#59797=CARTESIAN_POINT('',(32.4202336411144,93.8,-114.793004492904));
#59798=CARTESIAN_POINT('',(32.4202336411144,93.8,-114.793004492904));
#59799=CARTESIAN_POINT('',(32.8533684435232,93.8,-117.647076597157));
#59800=CARTESIAN_POINT('',(32.8533684435232,93.8,-117.647076597157));
#59801=CARTESIAN_POINT('',(35.5416347912432,93.8,-118.699006907135));
#59802=CARTESIAN_POINT('',(35.5416347912432,93.8,-118.699006907135));
#59803=CARTESIAN_POINT('',(37.7967663365545,93.8,-116.896865112859));
#59804=CARTESIAN_POINT('',(-47.5735358658191,93.8,-73.8317547968122));
#59805=CARTESIAN_POINT('',(-47.1404010634104,93.8,-76.6858269010653));
#59806=CARTESIAN_POINT('',(-47.5735358658191,93.8,-73.8317547968122));
#59807=CARTESIAN_POINT('',(-50.2618022135392,93.8,-72.7798244868348));
#59808=CARTESIAN_POINT('',(-50.2618022135392,93.8,-72.7798244868348));
#59809=CARTESIAN_POINT('',(-52.5169337588505,93.8,-74.5819662811105));
#59810=CARTESIAN_POINT('',(-52.5169337588505,93.8,-74.5819662811105));
#59811=CARTESIAN_POINT('',(-52.0837989564418,93.8,-77.4360383853636));
#59812=CARTESIAN_POINT('',(-52.0837989564418,93.8,-77.4360383853636));
#59813=CARTESIAN_POINT('',(-49.3955326087217,93.8,-78.487968695341));
#59814=CARTESIAN_POINT('',(-49.3955326087217,93.8,-78.487968695341));
#59815=CARTESIAN_POINT('',(-47.1404010634104,93.8,-76.6858269010653));
#59816=CARTESIAN_POINT('',(-40.589215018026,93.8,-76.5647499111661));
#59817=CARTESIAN_POINT('',(-40.1560802156173,93.8,-79.4188220154192));
#59818=CARTESIAN_POINT('',(-40.589215018026,93.8,-76.5647499111661));
#59819=CARTESIAN_POINT('',(-43.277481365746,93.8,-75.5128196011887));
#59820=CARTESIAN_POINT('',(-43.277481365746,93.8,-75.5128196011887));
#59821=CARTESIAN_POINT('',(-45.5326129110574,93.8,-77.3149613954644));
#59822=CARTESIAN_POINT('',(-45.5326129110574,93.8,-77.3149613954644));
#59823=CARTESIAN_POINT('',(-45.0994781086486,93.8,-80.1690334997174));
#59824=CARTESIAN_POINT('',(-45.0994781086486,93.8,-80.1690334997174));
#59825=CARTESIAN_POINT('',(-42.4112117609286,93.8,-81.2209638096949));
#59826=CARTESIAN_POINT('',(-42.4112117609286,93.8,-81.2209638096949));
#59827=CARTESIAN_POINT('',(-40.1560802156173,93.8,-79.4188220154192));
#59828=CARTESIAN_POINT('',(-33.6048941702329,93.8,-79.29774502552));
#59829=CARTESIAN_POINT('',(-33.1717593678242,93.8,-82.1518171297731));
#59830=CARTESIAN_POINT('',(-33.6048941702329,93.8,-79.29774502552));
#59831=CARTESIAN_POINT('',(-36.2931605179529,93.8,-78.2458147155426));
#59832=CARTESIAN_POINT('',(-36.2931605179529,93.8,-78.2458147155426));
#59833=CARTESIAN_POINT('',(-38.5482920632642,93.8,-80.0479565098183));
#59834=CARTESIAN_POINT('',(-38.5482920632642,93.8,-80.0479565098183));
#59835=CARTESIAN_POINT('',(-38.1151572608555,93.8,-82.9020286140714));
#59836=CARTESIAN_POINT('',(-38.1151572608555,93.8,-82.9020286140714));
#59837=CARTESIAN_POINT('',(-35.4268909131355,93.8,-83.9539589240488));
#59838=CARTESIAN_POINT('',(-35.4268909131355,93.8,-83.9539589240488));
#59839=CARTESIAN_POINT('',(-33.1717593678242,93.8,-82.1518171297731));
#59840=CARTESIAN_POINT('',(29.2539934599053,93.8,-103.894701054705));
#59841=CARTESIAN_POINT('',(29.687128262314,93.8,-106.748773158958));
#59842=CARTESIAN_POINT('',(29.2539934599053,93.8,-103.894701054705));
#59843=CARTESIAN_POINT('',(26.5657271121853,93.8,-102.842770744728));
#59844=CARTESIAN_POINT('',(26.5657271121853,93.8,-102.842770744728));
#59845=CARTESIAN_POINT('',(24.3105955668739,93.8,-104.644912539003));
#59846=CARTESIAN_POINT('',(24.3105955668739,93.8,-104.644912539003));
#59847=CARTESIAN_POINT('',(24.7437303692827,93.8,-107.498984643256));
#59848=CARTESIAN_POINT('',(24.7437303692827,93.8,-107.498984643256));
#59849=CARTESIAN_POINT('',(27.4319967170027,93.8,-108.550914953234));
#59850=CARTESIAN_POINT('',(27.4319967170027,93.8,-108.550914953234));
#59851=CARTESIAN_POINT('',(29.687128262314,93.8,-106.748773158958));
#59852=CARTESIAN_POINT('',(36.2383143076984,93.8,-106.627696169059));
#59853=CARTESIAN_POINT('',(36.6714491101071,93.8,-109.481768273312));
#59854=CARTESIAN_POINT('',(36.2383143076984,93.8,-106.627696169059));
#59855=CARTESIAN_POINT('',(33.5500479599784,93.8,-105.575765859081));
#59856=CARTESIAN_POINT('',(33.5500479599784,93.8,-105.575765859081));
#59857=CARTESIAN_POINT('',(31.2949164146671,93.8,-107.377907653357));
#59858=CARTESIAN_POINT('',(31.2949164146671,93.8,-107.377907653357));
#59859=CARTESIAN_POINT('',(31.7280512170758,93.8,-110.23197975761));
#59860=CARTESIAN_POINT('',(31.7280512170758,93.8,-110.23197975761));
#59861=CARTESIAN_POINT('',(34.4163175647958,93.8,-111.283910067588));
#59862=CARTESIAN_POINT('',(34.4163175647958,93.8,-111.283910067588));
#59863=CARTESIAN_POINT('',(36.6714491101071,93.8,-109.481768273312));
#59864=CARTESIAN_POINT('',(43.2226351554916,93.8,-109.360691283413));
#59865=CARTESIAN_POINT('',(43.6557699579003,93.8,-112.214763387666));
#59866=CARTESIAN_POINT('',(43.2226351554916,93.8,-109.360691283413));
#59867=CARTESIAN_POINT('',(40.5343688077715,93.8,-108.308760973435));
#59868=CARTESIAN_POINT('',(40.5343688077715,93.8,-108.308760973435));
#59869=CARTESIAN_POINT('',(38.2792372624602,93.8,-110.110902767711));
#59870=CARTESIAN_POINT('',(38.2792372624602,93.8,-110.110902767711));
#59871=CARTESIAN_POINT('',(38.7123720648689,93.8,-112.964974871964));
#59872=CARTESIAN_POINT('',(38.7123720648689,93.8,-112.964974871964));
#59873=CARTESIAN_POINT('',(41.4006384125889,93.8,-114.016905181942));
#59874=CARTESIAN_POINT('',(41.4006384125889,93.8,-114.016905181942));
#59875=CARTESIAN_POINT('',(43.6557699579003,93.8,-112.214763387666));
#59876=CARTESIAN_POINT('',(-48.6988530922665,93.8,-66.4166579572652));
#59877=CARTESIAN_POINT('',(-48.2657182898578,93.8,-69.2707300615183));
#59878=CARTESIAN_POINT('',(-48.6988530922665,93.8,-66.4166579572652));
#59879=CARTESIAN_POINT('',(-51.3871194399865,93.8,-65.3647276472878));
#59880=CARTESIAN_POINT('',(-51.3871194399865,93.8,-65.3647276472878));
#59881=CARTESIAN_POINT('',(-53.6422509852979,93.8,-67.1668694415634));
#59882=CARTESIAN_POINT('',(-53.6422509852979,93.8,-67.1668694415634));
#59883=CARTESIAN_POINT('',(-53.2091161828892,93.8,-70.0209415458165));
#59884=CARTESIAN_POINT('',(-53.2091161828892,93.8,-70.0209415458165));
#59885=CARTESIAN_POINT('',(-50.5208498351691,93.8,-71.0728718557939));
#59886=CARTESIAN_POINT('',(-50.5208498351691,93.8,-71.0728718557939));
#59887=CARTESIAN_POINT('',(-48.2657182898578,93.8,-69.2707300615183));
#59888=CARTESIAN_POINT('',(22.2696726121122,93.8,-101.161705940351));
#59889=CARTESIAN_POINT('',(22.7028074145209,93.8,-104.015778044604));
#59890=CARTESIAN_POINT('',(22.2696726121122,93.8,-101.161705940351));
#59891=CARTESIAN_POINT('',(19.5814062643922,93.8,-100.109775630374));
#59892=CARTESIAN_POINT('',(19.5814062643922,93.8,-100.109775630374));
#59893=CARTESIAN_POINT('',(17.3262747190808,93.8,-101.911917424649));
#59894=CARTESIAN_POINT('',(17.3262747190808,93.8,-101.911917424649));
#59895=CARTESIAN_POINT('',(17.7594095214895,93.8,-104.765989528902));
#59896=CARTESIAN_POINT('',(17.7594095214895,93.8,-104.765989528902));
#59897=CARTESIAN_POINT('',(20.4476758692096,93.8,-105.81791983888));
#59898=CARTESIAN_POINT('',(20.4476758692096,93.8,-105.81791983888));
#59899=CARTESIAN_POINT('',(22.7028074145209,93.8,-104.015778044604));
#59900=CARTESIAN_POINT('',(15.285351764319,93.8,-98.4287108259972));
#59901=CARTESIAN_POINT('',(15.7184865667278,93.8,-101.28278293025));
#59902=CARTESIAN_POINT('',(15.285351764319,93.8,-98.4287108259972));
#59903=CARTESIAN_POINT('',(12.597085416599,93.8,-97.3767805160198));
#59904=CARTESIAN_POINT('',(12.597085416599,93.8,-97.3767805160198));
#59905=CARTESIAN_POINT('',(10.3419538712877,93.8,-99.1789223102955));
#59906=CARTESIAN_POINT('',(10.3419538712877,93.8,-99.1789223102955));
#59907=CARTESIAN_POINT('',(10.7750886736964,93.8,-102.032994414549));
#59908=CARTESIAN_POINT('',(10.7750886736964,93.8,-102.032994414549));
#59909=CARTESIAN_POINT('',(13.4633550214164,93.8,-103.084924724526));
#59910=CARTESIAN_POINT('',(13.4633550214164,93.8,-103.084924724526));
#59911=CARTESIAN_POINT('',(15.7184865667278,93.8,-101.28278293025));
#59912=CARTESIAN_POINT('',(8.3010309165259,93.8,-95.6957157116433));
#59913=CARTESIAN_POINT('',(8.73416571893462,93.8,-98.5497878158964));
#59914=CARTESIAN_POINT('',(8.3010309165259,93.8,-95.6957157116433));
#59915=CARTESIAN_POINT('',(5.6127645688059,93.8,-94.6437854016659));
#59916=CARTESIAN_POINT('',(5.6127645688059,93.8,-94.6437854016659));
#59917=CARTESIAN_POINT('',(3.35763302349454,93.8,-96.4459271959416));
#59918=CARTESIAN_POINT('',(3.35763302349454,93.8,-96.4459271959416));
#59919=CARTESIAN_POINT('',(3.79076782590327,93.8,-99.2999993001947));
#59920=CARTESIAN_POINT('',(3.79076782590327,93.8,-99.2999993001947));
#59921=CARTESIAN_POINT('',(6.4790341736233,93.8,-100.351929610172));
#59922=CARTESIAN_POINT('',(6.4790341736233,93.8,-100.351929610172));
#59923=CARTESIAN_POINT('',(8.73416571893462,93.8,-98.5497878158964));
#59924=CARTESIAN_POINT('',(1.31671006873277,93.8,-92.9627205972894));
#59925=CARTESIAN_POINT('',(1.74984487114149,93.8,-95.8167927015425));
#59926=CARTESIAN_POINT('',(1.31671006873277,93.8,-92.9627205972894));
#59927=CARTESIAN_POINT('',(-1.37155627898724,93.8,-91.910790287312));
#59928=CARTESIAN_POINT('',(-1.37155627898724,93.8,-91.910790287312));
#59929=CARTESIAN_POINT('',(-3.6266878242986,93.8,-93.7129320815877));
#59930=CARTESIAN_POINT('',(-3.6266878242986,93.8,-93.7129320815877));
#59931=CARTESIAN_POINT('',(-3.19355302188986,93.8,-96.5670041858408));
#59932=CARTESIAN_POINT('',(-3.19355302188986,93.8,-96.5670041858408));
#59933=CARTESIAN_POINT('',(-0.505286674169835,93.8,-97.6189344958182));
#59934=CARTESIAN_POINT('',(-0.505286674169835,93.8,-97.6189344958182));
#59935=CARTESIAN_POINT('',(1.74984487114149,93.8,-95.8167927015425));
#59936=CARTESIAN_POINT('',(10.5516653694206,93.8,-110.525909390737));
#59937=CARTESIAN_POINT('',(10.9848001718294,93.8,-113.379981494991));
#59938=CARTESIAN_POINT('',(10.5516653694206,93.8,-110.525909390737));
#59939=CARTESIAN_POINT('',(7.86339902170064,93.8,-109.47397908076));
#59940=CARTESIAN_POINT('',(7.86339902170064,93.8,-109.47397908076));
#59941=CARTESIAN_POINT('',(5.60826747638928,93.8,-111.276120875036));
#59942=CARTESIAN_POINT('',(5.60826747638928,93.8,-111.276120875036));
#59943=CARTESIAN_POINT('',(6.04140227879801,93.8,-114.130192979289));
#59944=CARTESIAN_POINT('',(6.04140227879801,93.8,-114.130192979289));
#59945=CARTESIAN_POINT('',(8.72966862651804,93.8,-115.182123289266));
#59946=CARTESIAN_POINT('',(8.72966862651804,93.8,-115.182123289266));
#59947=CARTESIAN_POINT('',(10.9848001718294,93.8,-113.379981494991));
#59948=CARTESIAN_POINT('',(17.5359862172138,93.8,-113.258904505091));
#59949=CARTESIAN_POINT('',(17.9691210196225,93.8,-116.112976609344));
#59950=CARTESIAN_POINT('',(17.5359862172138,93.8,-113.258904505091));
#59951=CARTESIAN_POINT('',(14.8477198694938,93.8,-112.206974195114));
#59952=CARTESIAN_POINT('',(14.8477198694938,93.8,-112.206974195114));
#59953=CARTESIAN_POINT('',(12.5925883241824,93.8,-114.00911598939));
#59954=CARTESIAN_POINT('',(12.5925883241824,93.8,-114.00911598939));
#59955=CARTESIAN_POINT('',(13.0257231265911,93.8,-116.863188093643));
#59956=CARTESIAN_POINT('',(13.0257231265911,93.8,-116.863188093643));
#59957=CARTESIAN_POINT('',(15.7139894743112,93.8,-117.91511840362));
#59958=CARTESIAN_POINT('',(15.7139894743112,93.8,-117.91511840362));
#59959=CARTESIAN_POINT('',(17.9691210196225,93.8,-116.112976609344));
#59960=CARTESIAN_POINT('',(24.5203070650069,93.8,-115.991899619445));
#59961=CARTESIAN_POINT('',(24.9534418674156,93.8,-118.845971723698));
#59962=CARTESIAN_POINT('',(24.5203070650069,93.8,-115.991899619445));
#59963=CARTESIAN_POINT('',(21.8320407172869,93.8,-114.939969309468));
#59964=CARTESIAN_POINT('',(21.8320407172869,93.8,-114.939969309468));
#59965=CARTESIAN_POINT('',(19.5769091719755,93.8,-116.742111103744));
#59966=CARTESIAN_POINT('',(19.5769091719755,93.8,-116.742111103744));
#59967=CARTESIAN_POINT('',(20.0100439743843,93.8,-119.596183207997));
#59968=CARTESIAN_POINT('',(20.0100439743843,93.8,-119.596183207997));
#59969=CARTESIAN_POINT('',(22.6983103221043,93.8,-120.648113517974));
#59970=CARTESIAN_POINT('',(22.6983103221043,93.8,-120.648113517974));
#59971=CARTESIAN_POINT('',(24.9534418674156,93.8,-118.845971723698));
#59972=CARTESIAN_POINT('',(31.5046279128,93.8,-118.724894733799));
#59973=CARTESIAN_POINT('',(31.9377627152088,93.8,-121.578966838052));
#59974=CARTESIAN_POINT('',(31.5046279128,93.8,-118.724894733799));
#59975=CARTESIAN_POINT('',(28.81636156508,93.8,-117.672964423822));
#59976=CARTESIAN_POINT('',(28.81636156508,93.8,-117.672964423822));
#59977=CARTESIAN_POINT('',(26.5612300197687,93.8,-119.475106218097));
#59978=CARTESIAN_POINT('',(26.5612300197687,93.8,-119.475106218097));
#59979=CARTESIAN_POINT('',(26.9943648221774,93.8,-122.32917832235));
#59980=CARTESIAN_POINT('',(26.9943648221774,93.8,-122.32917832235));
#59981=CARTESIAN_POINT('',(29.6826311698974,93.8,-123.381108632328));
#59982=CARTESIAN_POINT('',(29.6826311698974,93.8,-123.381108632328));
#59983=CARTESIAN_POINT('',(31.9377627152088,93.8,-121.578966838052));
#59984=CARTESIAN_POINT('',(-46.4482186393718,93.8,-81.2468516363593));
#59985=CARTESIAN_POINT('',(-46.0150838369631,93.8,-84.1009237406124));
#59986=CARTESIAN_POINT('',(-46.4482186393718,93.8,-81.2468516363593));
#59987=CARTESIAN_POINT('',(-49.1364849870918,93.8,-80.1949213263819));
#59988=CARTESIAN_POINT('',(-49.1364849870918,93.8,-80.1949213263819));
#59989=CARTESIAN_POINT('',(-51.3916165324031,93.8,-81.9970631206576));
#59990=CARTESIAN_POINT('',(-51.3916165324031,93.8,-81.9970631206576));
#59991=CARTESIAN_POINT('',(-50.9584817299944,93.8,-84.8511352249106));
#59992=CARTESIAN_POINT('',(-50.9584817299944,93.8,-84.8511352249106));
#59993=CARTESIAN_POINT('',(-48.2702153822744,93.8,-85.9030655348881));
#59994=CARTESIAN_POINT('',(-48.2702153822744,93.8,-85.9030655348881));
#59995=CARTESIAN_POINT('',(-46.0150838369631,93.8,-84.1009237406124));
#59996=CARTESIAN_POINT('',(-39.4638977915786,93.8,-83.9798467507132));
#59997=CARTESIAN_POINT('',(-39.0307629891699,93.8,-86.8339188549663));
#59998=CARTESIAN_POINT('',(-39.4638977915786,93.8,-83.9798467507132));
#59999=CARTESIAN_POINT('',(-42.1521641392987,93.8,-82.9279164407358));
#60000=CARTESIAN_POINT('',(-42.1521641392987,93.8,-82.9279164407358));
#60001=CARTESIAN_POINT('',(-44.40729568461,93.8,-84.7300582350115));
#60002=CARTESIAN_POINT('',(-44.40729568461,93.8,-84.7300582350115));
#60003=CARTESIAN_POINT('',(-43.9741608822013,93.8,-87.5841303392645));
#60004=CARTESIAN_POINT('',(-43.9741608822013,93.8,-87.5841303392645));
#60005=CARTESIAN_POINT('',(-41.2858945344812,93.8,-88.636060649242));
#60006=CARTESIAN_POINT('',(-41.2858945344812,93.8,-88.636060649242));
#60007=CARTESIAN_POINT('',(-39.0307629891699,93.8,-86.8339188549663));
#60008=CARTESIAN_POINT('',(-32.4795769437855,93.8,-86.7128418650671));
#60009=CARTESIAN_POINT('',(-32.0464421413768,93.8,-89.5669139693202));
#60010=CARTESIAN_POINT('',(-32.4795769437855,93.8,-86.7128418650671));
#60011=CARTESIAN_POINT('',(-35.1678432915055,93.8,-85.6609115550896));
#60012=CARTESIAN_POINT('',(-35.1678432915055,93.8,-85.6609115550896));
#60013=CARTESIAN_POINT('',(-37.4229748368169,93.8,-87.4630533493654));
#60014=CARTESIAN_POINT('',(-37.4229748368169,93.8,-87.4630533493654));
#60015=CARTESIAN_POINT('',(-36.9898400344081,93.8,-90.3171254536184));
#60016=CARTESIAN_POINT('',(-36.9898400344081,93.8,-90.3171254536184));
#60017=CARTESIAN_POINT('',(-34.3015736866881,93.8,-91.3690557635958));
#60018=CARTESIAN_POINT('',(-34.3015736866881,93.8,-91.3690557635958));
#60019=CARTESIAN_POINT('',(-32.0464421413768,93.8,-89.5669139693202));
#60020=CARTESIAN_POINT('',(-25.4952560959924,93.8,-89.4458369794209));
#60021=CARTESIAN_POINT('',(-25.0621212935837,93.8,-92.2999090836741));
#60022=CARTESIAN_POINT('',(-25.4952560959924,93.8,-89.4458369794209));
#60023=CARTESIAN_POINT('',(-28.1835224437124,93.8,-88.3939066694435));
#60024=CARTESIAN_POINT('',(-28.1835224437124,93.8,-88.3939066694435));
#60025=CARTESIAN_POINT('',(-30.4386539890237,93.8,-90.1960484637193));
#60026=CARTESIAN_POINT('',(-30.4386539890237,93.8,-90.1960484637193));
#60027=CARTESIAN_POINT('',(-30.005519186615,93.8,-93.0501205679723));
#60028=CARTESIAN_POINT('',(-30.005519186615,93.8,-93.0501205679723));
#60029=CARTESIAN_POINT('',(-27.317252838895,93.8,-94.1020508779497));
#60030=CARTESIAN_POINT('',(-27.317252838895,93.8,-94.1020508779497));
#60031=CARTESIAN_POINT('',(-25.0621212935837,93.8,-92.2999090836741));
#60032=CARTESIAN_POINT('',(-18.5109352481993,93.8,-92.1788320937748));
#60033=CARTESIAN_POINT('',(-18.0778004457905,93.8,-95.0329041980279));
#60034=CARTESIAN_POINT('',(-18.5109352481993,93.8,-92.1788320937748));
#60035=CARTESIAN_POINT('',(-21.1992015959193,93.8,-91.1269017837974));
#60036=CARTESIAN_POINT('',(-21.1992015959193,93.8,-91.1269017837974));
#60037=CARTESIAN_POINT('',(-23.4543331412306,93.8,-92.9290435780731));
#60038=CARTESIAN_POINT('',(-23.4543331412306,93.8,-92.9290435780731));
#60039=CARTESIAN_POINT('',(-23.0211983388219,93.8,-95.7831156823262));
#60040=CARTESIAN_POINT('',(-23.0211983388219,93.8,-95.7831156823262));
#60041=CARTESIAN_POINT('',(-20.3329319911019,93.8,-96.8350459923036));
#60042=CARTESIAN_POINT('',(-20.3329319911019,93.8,-96.8350459923036));
#60043=CARTESIAN_POINT('',(-18.0778004457905,93.8,-95.0329041980279));
#60044=CARTESIAN_POINT('',(-11.5266144004061,93.8,-94.9118272081287));
#60045=CARTESIAN_POINT('',(-11.0934795979974,93.8,-97.7658993123818));
#60046=CARTESIAN_POINT('',(-11.5266144004061,93.8,-94.9118272081287));
#60047=CARTESIAN_POINT('',(-14.2148807481261,93.8,-93.8598968981513));
#60048=CARTESIAN_POINT('',(-14.2148807481261,93.8,-93.8598968981513));
#60049=CARTESIAN_POINT('',(-16.4700122934375,93.8,-95.662038692427));
#60050=CARTESIAN_POINT('',(-16.4700122934375,93.8,-95.662038692427));
#60051=CARTESIAN_POINT('',(-16.0368774910288,93.8,-98.5161107966801));
#60052=CARTESIAN_POINT('',(-16.0368774910288,93.8,-98.5161107966801));
#60053=CARTESIAN_POINT('',(-13.3486111433087,93.8,-99.5680411066575));
#60054=CARTESIAN_POINT('',(-13.3486111433087,93.8,-99.5680411066575));
#60055=CARTESIAN_POINT('',(-11.0934795979974,93.8,-97.7658993123818));
#60056=CARTESIAN_POINT('',(-4.54229355261299,93.8,-97.6448223224826));
#60057=CARTESIAN_POINT('',(-4.10915875020428,93.8,-100.498894426736));
#60058=CARTESIAN_POINT('',(-4.54229355261299,93.8,-97.6448223224826));
#60059=CARTESIAN_POINT('',(-7.230559900333,93.8,-96.5928920125052));
#60060=CARTESIAN_POINT('',(-7.230559900333,93.8,-96.5928920125052));
#60061=CARTESIAN_POINT('',(-9.48569144564436,93.8,-98.3950338067809));
#60062=CARTESIAN_POINT('',(-9.48569144564436,93.8,-98.3950338067809));
#60063=CARTESIAN_POINT('',(-9.05255664323563,93.8,-101.249105911034));
#60064=CARTESIAN_POINT('',(-9.05255664323563,93.8,-101.249105911034));
#60065=CARTESIAN_POINT('',(-6.3642902955156,93.8,-102.301036221011));
#60066=CARTESIAN_POINT('',(-6.3642902955156,93.8,-102.301036221011));
#60067=CARTESIAN_POINT('',(-4.10915875020428,93.8,-100.498894426736));
#60068=CARTESIAN_POINT('',(2.44202729518014,93.8,-100.377817436837));
#60069=CARTESIAN_POINT('',(2.87516209758886,93.8,-103.23188954109));
#60070=CARTESIAN_POINT('',(2.44202729518014,93.8,-100.377817436837));
#60071=CARTESIAN_POINT('',(-0.246239052539871,93.8,-99.3258871268591));
#60072=CARTESIAN_POINT('',(-0.246239052539871,93.8,-99.3258871268591));
#60073=CARTESIAN_POINT('',(-2.50137059785123,93.8,-101.128028921135));
#60074=CARTESIAN_POINT('',(-2.50137059785123,93.8,-101.128028921135));
#60075=CARTESIAN_POINT('',(-2.06823579544249,93.8,-103.982101025388));
#60076=CARTESIAN_POINT('',(-2.06823579544249,93.8,-103.982101025388));
#60077=CARTESIAN_POINT('',(0.620030552277533,93.8,-105.034031335365));
#60078=CARTESIAN_POINT('',(0.620030552277533,93.8,-105.034031335365));
#60079=CARTESIAN_POINT('',(2.87516209758886,93.8,-103.23188954109));
#60080=CARTESIAN_POINT('',(9.42634814297327,93.8,-103.11081255119));
#60081=CARTESIAN_POINT('',(9.85948294538199,93.8,-105.964884655444));
#60082=CARTESIAN_POINT('',(9.42634814297327,93.8,-103.11081255119));
#60083=CARTESIAN_POINT('',(6.73808179525326,93.8,-102.058882241213));
#60084=CARTESIAN_POINT('',(6.73808179525326,93.8,-102.058882241213));
#60085=CARTESIAN_POINT('',(4.48295024994191,93.8,-103.861024035489));
#60086=CARTESIAN_POINT('',(4.48295024994191,93.8,-103.861024035489));
#60087=CARTESIAN_POINT('',(4.91608505235064,93.8,-106.715096139742));
#60088=CARTESIAN_POINT('',(4.91608505235064,93.8,-106.715096139742));
#60089=CARTESIAN_POINT('',(7.60435140007067,93.8,-107.767026449719));
#60090=CARTESIAN_POINT('',(7.60435140007067,93.8,-107.767026449719));
#60091=CARTESIAN_POINT('',(9.85948294538199,93.8,-105.964884655444));
#60092=CARTESIAN_POINT('',(16.4106689907664,93.8,-105.843807665544));
#60093=CARTESIAN_POINT('',(16.8438037931751,93.8,-108.697879769797));
#60094=CARTESIAN_POINT('',(16.4106689907664,93.8,-105.843807665544));
#60095=CARTESIAN_POINT('',(13.7224026430464,93.8,-104.791877355567));
#60096=CARTESIAN_POINT('',(13.7224026430464,93.8,-104.791877355567));
#60097=CARTESIAN_POINT('',(11.467271097735,93.8,-106.594019149843));
#60098=CARTESIAN_POINT('',(11.467271097735,93.8,-106.594019149843));
#60099=CARTESIAN_POINT('',(11.9004059001438,93.8,-109.448091254096));
#60100=CARTESIAN_POINT('',(11.9004059001438,93.8,-109.448091254096));
#60101=CARTESIAN_POINT('',(14.5886722478638,93.8,-110.500021564073));
#60102=CARTESIAN_POINT('',(14.5886722478638,93.8,-110.500021564073));
#60103=CARTESIAN_POINT('',(16.8438037931751,93.8,-108.697879769797));
#60104=CARTESIAN_POINT('',(23.3949898385595,93.8,-108.576802779898));
#60105=CARTESIAN_POINT('',(23.8281246409682,93.8,-111.430874884151));
#60106=CARTESIAN_POINT('',(23.3949898385595,93.8,-108.576802779898));
#60107=CARTESIAN_POINT('',(20.7067234908395,93.8,-107.524872469921));
#60108=CARTESIAN_POINT('',(20.7067234908395,93.8,-107.524872469921));
#60109=CARTESIAN_POINT('',(18.4515919455282,93.8,-109.327014264196));
#60110=CARTESIAN_POINT('',(18.4515919455282,93.8,-109.327014264196));
#60111=CARTESIAN_POINT('',(18.8847267479369,93.8,-112.18108636845));
#60112=CARTESIAN_POINT('',(18.8847267479369,93.8,-112.18108636845));
#60113=CARTESIAN_POINT('',(21.5729930956569,93.8,-113.233016678427));
#60114=CARTESIAN_POINT('',(21.5729930956569,93.8,-113.233016678427));
#60115=CARTESIAN_POINT('',(23.8281246409682,93.8,-111.430874884151));
#60116=CARTESIAN_POINT('',(30.3793106863527,93.8,-111.309797894252));
#60117=CARTESIAN_POINT('',(30.8124454887614,93.8,-114.163869998505));
#60118=CARTESIAN_POINT('',(30.3793106863527,93.8,-111.309797894252));
#60119=CARTESIAN_POINT('',(27.6910443386327,93.8,-110.257867584275));
#60120=CARTESIAN_POINT('',(27.6910443386327,93.8,-110.257867584275));
#60121=CARTESIAN_POINT('',(25.4359127933213,93.8,-112.06000937855));
#60122=CARTESIAN_POINT('',(25.4359127933213,93.8,-112.06000937855));
#60123=CARTESIAN_POINT('',(25.86904759573,93.8,-114.914081482803));
#60124=CARTESIAN_POINT('',(25.86904759573,93.8,-114.914081482803));
#60125=CARTESIAN_POINT('',(28.5573139434501,93.8,-115.966011792781));
#60126=CARTESIAN_POINT('',(28.5573139434501,93.8,-115.966011792781));
#60127=CARTESIAN_POINT('',(30.8124454887614,93.8,-114.163869998505));
#60128=CARTESIAN_POINT('',(5.15749672629266,93.8,-31.6928392700737));
#60129=CARTESIAN_POINT('',(5.59063152870137,93.8,-34.5469113743268));
#60130=CARTESIAN_POINT('',(5.15749672629266,93.8,-31.6928392700737));
#60131=CARTESIAN_POINT('',(2.46923037857264,93.8,-30.6409089600963));
#60132=CARTESIAN_POINT('',(2.46923037857264,93.8,-30.6409089600963));
#60133=CARTESIAN_POINT('',(0.214098833261289,93.8,-32.443050754372));
#60134=CARTESIAN_POINT('',(0.214098833261289,93.8,-32.443050754372));
#60135=CARTESIAN_POINT('',(0.647233635670021,93.8,-35.2971228586251));
#60136=CARTESIAN_POINT('',(0.647233635670021,93.8,-35.2971228586251));
#60137=CARTESIAN_POINT('',(3.33549998339005,93.8,-36.3490531686025));
#60138=CARTESIAN_POINT('',(3.33549998339005,93.8,-36.3490531686025));
#60139=CARTESIAN_POINT('',(5.59063152870137,93.8,-34.5469113743268));
#60140=CARTESIAN_POINT('',(-1.82682412150048,93.8,-28.9598441557198));
#60141=CARTESIAN_POINT('',(-1.39368931909176,93.8,-31.8139162599729));
#60142=CARTESIAN_POINT('',(-1.82682412150048,93.8,-28.9598441557198));
#60143=CARTESIAN_POINT('',(-4.51509046922049,93.8,-27.9079138457424));
#60144=CARTESIAN_POINT('',(-4.51509046922049,93.8,-27.9079138457424));
#60145=CARTESIAN_POINT('',(-6.77022201453184,93.8,-29.7100556400181));
#60146=CARTESIAN_POINT('',(-6.77022201453184,93.8,-29.7100556400181));
#60147=CARTESIAN_POINT('',(-6.33708721212311,93.8,-32.5641277442712));
#60148=CARTESIAN_POINT('',(-6.33708721212311,93.8,-32.5641277442712));
#60149=CARTESIAN_POINT('',(-3.64882086440308,93.8,-33.6160580542486));
#60150=CARTESIAN_POINT('',(-3.64882086440308,93.8,-33.6160580542486));
#60151=CARTESIAN_POINT('',(-1.39368931909176,93.8,-31.8139162599729));
#60152=CARTESIAN_POINT('',(-8.81114496929361,93.8,-26.2268490413659));
#60153=CARTESIAN_POINT('',(-8.37801016688489,93.8,-29.080921145619));
#60154=CARTESIAN_POINT('',(-8.81114496929361,93.8,-26.2268490413659));
#60155=CARTESIAN_POINT('',(-11.4994113170136,93.8,-25.1749187313885));
#60156=CARTESIAN_POINT('',(-11.4994113170136,93.8,-25.1749187313885));
#60157=CARTESIAN_POINT('',(-13.754542862325,93.8,-26.9770605256642));
#60158=CARTESIAN_POINT('',(-13.754542862325,93.8,-26.9770605256642));
#60159=CARTESIAN_POINT('',(-13.3214080599162,93.8,-29.8311326299173));
#60160=CARTESIAN_POINT('',(-13.3214080599162,93.8,-29.8311326299173));
#60161=CARTESIAN_POINT('',(-10.6331417121962,93.8,-30.8830629398947));
#60162=CARTESIAN_POINT('',(-10.6331417121962,93.8,-30.8830629398947));
#60163=CARTESIAN_POINT('',(-8.37801016688489,93.8,-29.080921145619));
#60164=CARTESIAN_POINT('',(48.1887390394988,93.8,-55.5059067957441));
#60165=CARTESIAN_POINT('',(48.6218738419075,93.8,-58.3599788999972));
#60166=CARTESIAN_POINT('',(48.1887390394988,93.8,-55.5059067957441));
#60167=CARTESIAN_POINT('',(45.5004726917788,93.8,-54.4539764857667));
#60168=CARTESIAN_POINT('',(45.5004726917788,93.8,-54.4539764857667));
#60169=CARTESIAN_POINT('',(43.2453411464674,93.8,-56.2561182800424));
#60170=CARTESIAN_POINT('',(43.2453411464674,93.8,-56.2561182800424));
#60171=CARTESIAN_POINT('',(43.6784759488762,93.8,-59.1101903842955));
#60172=CARTESIAN_POINT('',(43.6784759488762,93.8,-59.1101903842955));
#60173=CARTESIAN_POINT('',(46.3667422965962,93.8,-60.1621206942729));
#60174=CARTESIAN_POINT('',(46.3667422965962,93.8,-60.1621206942729));
#60175=CARTESIAN_POINT('',(48.6218738419075,93.8,-58.3599788999972));
#60176=CARTESIAN_POINT('',(12.1418175740858,93.8,-34.4258343844276));
#60177=CARTESIAN_POINT('',(12.5749523764945,93.8,-37.2799064886807));
#60178=CARTESIAN_POINT('',(12.1418175740858,93.8,-34.4258343844276));
#60179=CARTESIAN_POINT('',(9.45355122636578,93.8,-33.3739040744502));
#60180=CARTESIAN_POINT('',(9.45355122636578,93.8,-33.3739040744502));
#60181=CARTESIAN_POINT('',(7.19841968105442,93.8,-35.1760458687259));
#60182=CARTESIAN_POINT('',(7.19841968105442,93.8,-35.1760458687259));
#60183=CARTESIAN_POINT('',(7.63155448346315,93.8,-38.030117972979));
#60184=CARTESIAN_POINT('',(7.63155448346315,93.8,-38.030117972979));
#60185=CARTESIAN_POINT('',(10.3198208311832,93.8,-39.0820482829564));
#60186=CARTESIAN_POINT('',(10.3198208311832,93.8,-39.0820482829564));
#60187=CARTESIAN_POINT('',(12.5749523764945,93.8,-37.2799064886807));
#60188=CARTESIAN_POINT('',(19.1261384218789,93.8,-37.1588294987815));
#60189=CARTESIAN_POINT('',(19.5592732242876,93.8,-40.0129016030346));
#60190=CARTESIAN_POINT('',(19.1261384218789,93.8,-37.1588294987815));
#60191=CARTESIAN_POINT('',(16.4378720741589,93.8,-36.1068991888041));
#60192=CARTESIAN_POINT('',(16.4378720741589,93.8,-36.1068991888041));
#60193=CARTESIAN_POINT('',(14.1827405288475,93.8,-37.9090409830798));
#60194=CARTESIAN_POINT('',(14.1827405288475,93.8,-37.9090409830798));
#60195=CARTESIAN_POINT('',(14.6158753312563,93.8,-40.7631130873329));
#60196=CARTESIAN_POINT('',(14.6158753312563,93.8,-40.7631130873329));
#60197=CARTESIAN_POINT('',(17.3041416789763,93.8,-41.8150433973103));
#60198=CARTESIAN_POINT('',(17.3041416789763,93.8,-41.8150433973103));
#60199=CARTESIAN_POINT('',(19.5592732242876,93.8,-40.0129016030346));
#60200=CARTESIAN_POINT('',(26.110459269672,93.8,-39.8918246131354));
#60201=CARTESIAN_POINT('',(26.5435940720808,93.8,-42.7458967173885));
#60202=CARTESIAN_POINT('',(26.110459269672,93.8,-39.8918246131354));
#60203=CARTESIAN_POINT('',(23.422192921952,93.8,-38.839894303158));
#60204=CARTESIAN_POINT('',(23.422192921952,93.8,-38.839894303158));
#60205=CARTESIAN_POINT('',(21.1670613766407,93.8,-40.6420360974337));
#60206=CARTESIAN_POINT('',(21.1670613766407,93.8,-40.6420360974337));
#60207=CARTESIAN_POINT('',(21.6001961790494,93.8,-43.4961082016867));
#60208=CARTESIAN_POINT('',(21.6001961790494,93.8,-43.4961082016867));
#60209=CARTESIAN_POINT('',(24.2884625267694,93.8,-44.5480385116642));
#60210=CARTESIAN_POINT('',(24.2884625267694,93.8,-44.5480385116642));
#60211=CARTESIAN_POINT('',(26.5435940720808,93.8,-42.7458967173885));
#60212=CARTESIAN_POINT('',(33.0947801174652,93.8,-42.6248197274893));
#60213=CARTESIAN_POINT('',(33.5279149198739,93.8,-45.4788918317424));
#60214=CARTESIAN_POINT('',(33.0947801174652,93.8,-42.6248197274893));
#60215=CARTESIAN_POINT('',(30.4065137697452,93.8,-41.5728894175119));
#60216=CARTESIAN_POINT('',(30.4065137697452,93.8,-41.5728894175119));
#60217=CARTESIAN_POINT('',(28.1513822244338,93.8,-43.3750312117876));
#60218=CARTESIAN_POINT('',(28.1513822244338,93.8,-43.3750312117876));
#60219=CARTESIAN_POINT('',(28.5845170268425,93.8,-46.2291033160406));
#60220=CARTESIAN_POINT('',(28.5845170268425,93.8,-46.2291033160406));
#60221=CARTESIAN_POINT('',(31.2727833745626,93.8,-47.2810336260181));
#60222=CARTESIAN_POINT('',(31.2727833745626,93.8,-47.2810336260181));
#60223=CARTESIAN_POINT('',(33.5279149198739,93.8,-45.4788918317424));
#60224=CARTESIAN_POINT('',(41.2044181917057,93.8,-52.7729116813902));
#60225=CARTESIAN_POINT('',(41.6375529941144,93.8,-55.6269837856433));
#60226=CARTESIAN_POINT('',(41.2044181917057,93.8,-52.7729116813902));
#60227=CARTESIAN_POINT('',(38.5161518439857,93.8,-51.7209813714128));
#60228=CARTESIAN_POINT('',(38.5161518439857,93.8,-51.7209813714128));
#60229=CARTESIAN_POINT('',(36.2610202986743,93.8,-53.5231231656885));
#60230=CARTESIAN_POINT('',(36.2610202986743,93.8,-53.5231231656885));
#60231=CARTESIAN_POINT('',(36.694155101083,93.8,-56.3771952699416));
#60232=CARTESIAN_POINT('',(36.694155101083,93.8,-56.3771952699416));
#60233=CARTESIAN_POINT('',(39.3824214488031,93.8,-57.429125579919));
#60234=CARTESIAN_POINT('',(39.3824214488031,93.8,-57.429125579919));
#60235=CARTESIAN_POINT('',(41.6375529941144,93.8,-55.6269837856433));
#60236=CARTESIAN_POINT('',(34.2200973439125,93.8,-50.0399165670363));
#60237=CARTESIAN_POINT('',(34.6532321463213,93.8,-52.8939886712894));
#60238=CARTESIAN_POINT('',(34.2200973439125,93.8,-50.0399165670363));
#60239=CARTESIAN_POINT('',(31.5318309961925,93.8,-48.9879862570589));
#60240=CARTESIAN_POINT('',(31.5318309961925,93.8,-48.9879862570589));
#60241=CARTESIAN_POINT('',(29.2766994508812,93.8,-50.7901280513346));
#60242=CARTESIAN_POINT('',(29.2766994508812,93.8,-50.7901280513346));
#60243=CARTESIAN_POINT('',(29.7098342532899,93.8,-53.6442001555877));
#60244=CARTESIAN_POINT('',(29.7098342532899,93.8,-53.6442001555877));
#60245=CARTESIAN_POINT('',(32.3981006010099,93.8,-54.6961304655651));
#60246=CARTESIAN_POINT('',(32.3981006010099,93.8,-54.6961304655651));
#60247=CARTESIAN_POINT('',(34.6532321463213,93.8,-52.8939886712894));
#60248=CARTESIAN_POINT('',(27.2357764961194,93.8,-47.3069214526824));
#60249=CARTESIAN_POINT('',(27.6689112985281,93.8,-50.1609935569356));
#60250=CARTESIAN_POINT('',(27.2357764961194,93.8,-47.3069214526824));
#60251=CARTESIAN_POINT('',(24.5475101483994,93.8,-46.254991142705));
#60252=CARTESIAN_POINT('',(24.5475101483994,93.8,-46.254991142705));
#60253=CARTESIAN_POINT('',(22.2923786030881,93.8,-48.0571329369807));
#60254=CARTESIAN_POINT('',(22.2923786030881,93.8,-48.0571329369807));
#60255=CARTESIAN_POINT('',(22.7255134054968,93.8,-50.9112050412338));
#60256=CARTESIAN_POINT('',(22.7255134054968,93.8,-50.9112050412338));
#60257=CARTESIAN_POINT('',(25.4137797532168,93.8,-51.9631353512112));
#60258=CARTESIAN_POINT('',(25.4137797532168,93.8,-51.9631353512112));
#60259=CARTESIAN_POINT('',(27.6689112985281,93.8,-50.1609935569356));
#60260=CARTESIAN_POINT('',(20.2514556483263,93.8,-44.5739263383286));
#60261=CARTESIAN_POINT('',(20.684590450735,93.8,-47.4279984425817));
#60262=CARTESIAN_POINT('',(20.2514556483263,93.8,-44.5739263383286));
#60263=CARTESIAN_POINT('',(17.5631893006063,93.8,-43.5219960283511));
#60264=CARTESIAN_POINT('',(17.5631893006063,93.8,-43.5219960283511));
#60265=CARTESIAN_POINT('',(15.3080577552949,93.8,-45.3241378226269));
#60266=CARTESIAN_POINT('',(15.3080577552949,93.8,-45.3241378226269));
#60267=CARTESIAN_POINT('',(15.7411925577037,93.8,-48.1782099268799));
#60268=CARTESIAN_POINT('',(15.7411925577037,93.8,-48.1782099268799));
#60269=CARTESIAN_POINT('',(18.4294589054237,93.8,-49.2301402368573));
#60270=CARTESIAN_POINT('',(18.4294589054237,93.8,-49.2301402368573));
#60271=CARTESIAN_POINT('',(20.684590450735,93.8,-47.4279984425817));
#60272=CARTESIAN_POINT('',(13.2671348005332,93.8,-41.8409312239747));
#60273=CARTESIAN_POINT('',(13.7002696029419,93.8,-44.6950033282278));
#60274=CARTESIAN_POINT('',(13.2671348005332,93.8,-41.8409312239747));
#60275=CARTESIAN_POINT('',(10.5788684528132,93.8,-40.7890009139973));
#60276=CARTESIAN_POINT('',(10.5788684528132,93.8,-40.7890009139973));
#60277=CARTESIAN_POINT('',(8.32373690750179,93.8,-42.591142708273));
#60278=CARTESIAN_POINT('',(8.32373690750179,93.8,-42.591142708273));
#60279=CARTESIAN_POINT('',(8.75687170991053,93.8,-45.445214812526));
#60280=CARTESIAN_POINT('',(8.75687170991053,93.8,-45.445214812526));
#60281=CARTESIAN_POINT('',(11.4451380576306,93.8,-46.4971451225034));
#60282=CARTESIAN_POINT('',(11.4451380576306,93.8,-46.4971451225034));
#60283=CARTESIAN_POINT('',(13.7002696029419,93.8,-44.6950033282278));
#60284=CARTESIAN_POINT('',(6.28281395274003,93.8,-39.1079361096208));
#60285=CARTESIAN_POINT('',(6.71594875514875,93.8,-41.9620082138739));
#60286=CARTESIAN_POINT('',(6.28281395274003,93.8,-39.1079361096208));
#60287=CARTESIAN_POINT('',(3.59454760502002,93.8,-38.0560057996434));
#60288=CARTESIAN_POINT('',(3.59454760502002,93.8,-38.0560057996434));
#60289=CARTESIAN_POINT('',(1.33941605970866,93.8,-39.8581475939191));
#60290=CARTESIAN_POINT('',(1.33941605970866,93.8,-39.8581475939191));
#60291=CARTESIAN_POINT('',(1.7725508621174,93.8,-42.7122196981721));
#60292=CARTESIAN_POINT('',(1.7725508621174,93.8,-42.7122196981721));
#60293=CARTESIAN_POINT('',(4.46081720983742,93.8,-43.7641500081495));
#60294=CARTESIAN_POINT('',(4.46081720983742,93.8,-43.7641500081495));
#60295=CARTESIAN_POINT('',(6.71594875514875,93.8,-41.9620082138739));
#60296=CARTESIAN_POINT('',(-0.701506895053102,93.8,-36.3749409952669));
#60297=CARTESIAN_POINT('',(-0.268372092644385,93.8,-39.22901309952));
#60298=CARTESIAN_POINT('',(-0.701506895053102,93.8,-36.3749409952669));
#60299=CARTESIAN_POINT('',(-3.38977324277311,93.8,-35.3230106852895));
#60300=CARTESIAN_POINT('',(-3.38977324277311,93.8,-35.3230106852895));
#60301=CARTESIAN_POINT('',(-5.64490478808447,93.8,-37.1251524795652));
#60302=CARTESIAN_POINT('',(-5.64490478808447,93.8,-37.1251524795652));
#60303=CARTESIAN_POINT('',(-5.21176998567574,93.8,-39.9792245838182));
#60304=CARTESIAN_POINT('',(-5.21176998567574,93.8,-39.9792245838182));
#60305=CARTESIAN_POINT('',(-2.52350363795571,93.8,-41.0311548937957));
#60306=CARTESIAN_POINT('',(-2.52350363795571,93.8,-41.0311548937957));
#60307=CARTESIAN_POINT('',(-0.268372092644385,93.8,-39.22901309952));
#60308=CARTESIAN_POINT('',(-7.68582774284623,93.8,-33.641945880913));
#60309=CARTESIAN_POINT('',(-7.25269294043752,93.8,-36.4960179851661));
#60310=CARTESIAN_POINT('',(-7.68582774284623,93.8,-33.641945880913));
#60311=CARTESIAN_POINT('',(-10.3740940905662,93.8,-32.5900155709356));
#60312=CARTESIAN_POINT('',(-10.3740940905662,93.8,-32.5900155709356));
#60313=CARTESIAN_POINT('',(-12.6292256358776,93.8,-34.3921573652113));
#60314=CARTESIAN_POINT('',(-12.6292256358776,93.8,-34.3921573652113));
#60315=CARTESIAN_POINT('',(-12.1960908334689,93.8,-37.2462294694643));
#60316=CARTESIAN_POINT('',(-12.1960908334689,93.8,-37.2462294694643));
#60317=CARTESIAN_POINT('',(-9.50782448574884,93.8,-38.2981597794418));
#60318=CARTESIAN_POINT('',(-9.50782448574884,93.8,-38.2981597794418));
#60319=CARTESIAN_POINT('',(-7.25269294043752,93.8,-36.4960179851661));
#60320=CARTESIAN_POINT('',(38.9537837388109,93.8,-37.9427180022961));
#60321=CARTESIAN_POINT('',(39.3869185412196,93.8,-40.7967901065492));
#60322=CARTESIAN_POINT('',(38.9537837388109,93.8,-37.9427180022961));
#60323=CARTESIAN_POINT('',(36.2655173910909,93.8,-36.8907876923187));
#60324=CARTESIAN_POINT('',(36.2655173910909,93.8,-36.8907876923187));
#60325=CARTESIAN_POINT('',(34.0103858457796,93.8,-38.6929294865944));
#60326=CARTESIAN_POINT('',(34.0103858457796,93.8,-38.6929294865944));
#60327=CARTESIAN_POINT('',(34.4435206481883,93.8,-41.5470015908475));
#60328=CARTESIAN_POINT('',(34.4435206481883,93.8,-41.5470015908475));
#60329=CARTESIAN_POINT('',(37.1317869959083,93.8,-42.5989319008249));
#60330=CARTESIAN_POINT('',(37.1317869959083,93.8,-42.5989319008249));
#60331=CARTESIAN_POINT('',(39.3869185412196,93.8,-40.7967901065492));
#60332=CARTESIAN_POINT('',(31.9694628910178,93.8,-35.2097228879422));
#60333=CARTESIAN_POINT('',(32.4025976934265,93.8,-38.0637949921953));
#60334=CARTESIAN_POINT('',(31.9694628910178,93.8,-35.2097228879422));
#60335=CARTESIAN_POINT('',(29.2811965432978,93.8,-34.1577925779648));
#60336=CARTESIAN_POINT('',(29.2811965432978,93.8,-34.1577925779648));
#60337=CARTESIAN_POINT('',(27.0260649979864,93.8,-35.9599343722405));
#60338=CARTESIAN_POINT('',(27.0260649979864,93.8,-35.9599343722405));
#60339=CARTESIAN_POINT('',(27.4591998003952,93.8,-38.8140064764936));
#60340=CARTESIAN_POINT('',(27.4591998003952,93.8,-38.8140064764936));
#60341=CARTESIAN_POINT('',(30.1474661481152,93.8,-39.865936786471));
#60342=CARTESIAN_POINT('',(30.1474661481152,93.8,-39.865936786471));
#60343=CARTESIAN_POINT('',(32.4025976934265,93.8,-38.0637949921953));
#60344=CARTESIAN_POINT('',(24.9851420432247,93.8,-32.4767277735883));
#60345=CARTESIAN_POINT('',(25.4182768456334,93.8,-35.3307998778415));
#60346=CARTESIAN_POINT('',(24.9851420432247,93.8,-32.4767277735883));
#60347=CARTESIAN_POINT('',(22.2968756955047,93.8,-31.4247974636109));
#60348=CARTESIAN_POINT('',(22.2968756955047,93.8,-31.4247974636109));
#60349=CARTESIAN_POINT('',(20.0417441501933,93.8,-33.2269392578866));
#60350=CARTESIAN_POINT('',(20.0417441501933,93.8,-33.2269392578866));
#60351=CARTESIAN_POINT('',(20.474878952602,93.8,-36.0810113621397));
#60352=CARTESIAN_POINT('',(20.474878952602,93.8,-36.0810113621397));
#60353=CARTESIAN_POINT('',(23.1631453003221,93.8,-37.1329416721171));
#60354=CARTESIAN_POINT('',(23.1631453003221,93.8,-37.1329416721171));
#60355=CARTESIAN_POINT('',(25.4182768456334,93.8,-35.3307998778414));
#60356=CARTESIAN_POINT('',(18.0008211954315,93.8,-29.7437326592344));
#60357=CARTESIAN_POINT('',(18.4339559978403,93.8,-32.5978047634876));
#60358=CARTESIAN_POINT('',(18.0008211954315,93.8,-29.7437326592344));
#60359=CARTESIAN_POINT('',(15.3125548477115,93.8,-28.691802349257));
#60360=CARTESIAN_POINT('',(15.3125548477115,93.8,-28.691802349257));
#60361=CARTESIAN_POINT('',(13.0574233024002,93.8,-30.4939441435327));
#60362=CARTESIAN_POINT('',(13.0574233024002,93.8,-30.4939441435327));
#60363=CARTESIAN_POINT('',(13.4905581048089,93.8,-33.3480162477858));
#60364=CARTESIAN_POINT('',(13.4905581048089,93.8,-33.3480162477858));
#60365=CARTESIAN_POINT('',(16.1788244525289,93.8,-34.3999465577632));
#60366=CARTESIAN_POINT('',(16.1788244525289,93.8,-34.3999465577632));
#60367=CARTESIAN_POINT('',(18.4339559978403,93.8,-32.5978047634875));
#60368=CARTESIAN_POINT('',(11.0165003476384,93.8,-27.0107375448806));
#60369=CARTESIAN_POINT('',(11.4496351500471,93.8,-29.8648096491337));
#60370=CARTESIAN_POINT('',(11.0165003476384,93.8,-27.0107375448806));
#60371=CARTESIAN_POINT('',(8.3282339999184,93.8,-25.9588072349031));
#60372=CARTESIAN_POINT('',(8.3282339999184,93.8,-25.9588072349031));
#60373=CARTESIAN_POINT('',(6.07310245460704,93.8,-27.7609490291788));
#60374=CARTESIAN_POINT('',(6.07310245460704,93.8,-27.7609490291788));
#60375=CARTESIAN_POINT('',(6.50623725701577,93.8,-30.6150211334319));
#60376=CARTESIAN_POINT('',(6.50623725701577,93.8,-30.6150211334319));
#60377=CARTESIAN_POINT('',(9.1945036047358,93.8,-31.6669514434093));
#60378=CARTESIAN_POINT('',(9.1945036047358,93.8,-31.6669514434093));
#60379=CARTESIAN_POINT('',(11.4496351500471,93.8,-29.8648096491337));
#60380=CARTESIAN_POINT('',(4.03217949984528,93.8,-24.2777424305267));
#60381=CARTESIAN_POINT('',(4.465314302254,93.8,-27.1318145347798));
#60382=CARTESIAN_POINT('',(4.03217949984528,93.8,-24.2777424305267));
#60383=CARTESIAN_POINT('',(1.34391315212527,93.8,-23.2258121205493));
#60384=CARTESIAN_POINT('',(1.34391315212527,93.8,-23.2258121205493));
#60385=CARTESIAN_POINT('',(-0.911218393186086,93.8,-25.0279539148249));
#60386=CARTESIAN_POINT('',(-0.911218393186086,93.8,-25.0279539148249));
#60387=CARTESIAN_POINT('',(-0.478083590777355,93.8,-27.882026019078));
#60388=CARTESIAN_POINT('',(-0.478083590777355,93.8,-27.882026019078));
#60389=CARTESIAN_POINT('',(2.21018275694267,93.8,-28.9339563290554));
#60390=CARTESIAN_POINT('',(2.21018275694267,93.8,-28.9339563290554));
#60391=CARTESIAN_POINT('',(4.465314302254,93.8,-27.1318145347798));
#60392=CARTESIAN_POINT('',(47.0634218130514,93.8,-48.0908099561971));
#60393=CARTESIAN_POINT('',(47.4965566154602,93.8,-50.9448820604502));
#60394=CARTESIAN_POINT('',(47.0634218130514,93.8,-48.0908099561971));
#60395=CARTESIAN_POINT('',(44.3751554653314,93.8,-47.0388796462197));
#60396=CARTESIAN_POINT('',(44.3751554653314,93.8,-47.0388796462197));
#60397=CARTESIAN_POINT('',(42.1200239200201,93.8,-48.8410214404954));
#60398=CARTESIAN_POINT('',(42.1200239200201,93.8,-48.8410214404954));
#60399=CARTESIAN_POINT('',(42.5531587224288,93.8,-51.6950935447484));
#60400=CARTESIAN_POINT('',(42.5531587224288,93.8,-51.6950935447484));
#60401=CARTESIAN_POINT('',(45.2414250701488,93.8,-52.7470238547258));
#60402=CARTESIAN_POINT('',(45.2414250701488,93.8,-52.7470238547258));
#60403=CARTESIAN_POINT('',(47.4965566154602,93.8,-50.9448820604502));
#60404=CARTESIAN_POINT('',(40.0791009652583,93.8,-45.3578148418432));
#60405=CARTESIAN_POINT('',(40.512235767667,93.8,-48.2118869460963));
#60406=CARTESIAN_POINT('',(40.0791009652583,93.8,-45.3578148418432));
#60407=CARTESIAN_POINT('',(37.3908346175383,93.8,-44.3058845318658));
#60408=CARTESIAN_POINT('',(37.3908346175383,93.8,-44.3058845318658));
#60409=CARTESIAN_POINT('',(35.1357030722269,93.8,-46.1080263261415));
#60410=CARTESIAN_POINT('',(35.1357030722269,93.8,-46.1080263261415));
#60411=CARTESIAN_POINT('',(35.5688378746357,93.8,-48.9620984303945));
#60412=CARTESIAN_POINT('',(35.5688378746357,93.8,-48.9620984303945));
#60413=CARTESIAN_POINT('',(38.2571042223557,93.8,-50.014028740372));
#60414=CARTESIAN_POINT('',(38.2571042223557,93.8,-50.014028740372));
#60415=CARTESIAN_POINT('',(40.512235767667,93.8,-48.2118869460963));
#60416=CARTESIAN_POINT('',(36.4707317968073,93.8,-64.8701102461305));
#60417=CARTESIAN_POINT('',(36.903866599216,93.8,-67.7241823503836));
#60418=CARTESIAN_POINT('',(36.4707317968073,93.8,-64.8701102461305));
#60419=CARTESIAN_POINT('',(33.7824654490873,93.8,-63.818179936153));
#60420=CARTESIAN_POINT('',(33.7824654490873,93.8,-63.818179936153));
#60421=CARTESIAN_POINT('',(31.5273339037759,93.8,-65.6203217304287));
#60422=CARTESIAN_POINT('',(31.5273339037759,93.8,-65.6203217304287));
#60423=CARTESIAN_POINT('',(31.9604687061847,93.8,-68.4743938346818));
#60424=CARTESIAN_POINT('',(31.9604687061847,93.8,-68.4743938346818));
#60425=CARTESIAN_POINT('',(34.6487350539047,93.8,-69.5263241446592));
#60426=CARTESIAN_POINT('',(34.6487350539047,93.8,-69.5263241446592));
#60427=CARTESIAN_POINT('',(36.903866599216,93.8,-67.7241823503836));
#60428=CARTESIAN_POINT('',(29.4864109490142,93.8,-62.1371151317766));
#60429=CARTESIAN_POINT('',(29.9195457514229,93.8,-64.9911872360297));
#60430=CARTESIAN_POINT('',(29.4864109490142,93.8,-62.1371151317766));
#60431=CARTESIAN_POINT('',(26.7981446012942,93.8,-61.0851848217992));
#60432=CARTESIAN_POINT('',(26.7981446012942,93.8,-61.0851848217992));
#60433=CARTESIAN_POINT('',(24.5430130559828,93.8,-62.8873266160749));
#60434=CARTESIAN_POINT('',(24.5430130559828,93.8,-62.8873266160749));
#60435=CARTESIAN_POINT('',(24.9761478583915,93.8,-65.7413987203279));
#60436=CARTESIAN_POINT('',(24.9761478583915,93.8,-65.7413987203279));
#60437=CARTESIAN_POINT('',(27.6644142061116,93.8,-66.7933290303053));
#60438=CARTESIAN_POINT('',(27.6644142061116,93.8,-66.7933290303053));
#60439=CARTESIAN_POINT('',(29.9195457514229,93.8,-64.9911872360297));
#60440=CARTESIAN_POINT('',(22.502090101221,93.8,-59.4041200174227));
#60441=CARTESIAN_POINT('',(22.9352249036298,93.8,-62.2581921216758));
#60442=CARTESIAN_POINT('',(22.502090101221,93.8,-59.4041200174227));
#60443=CARTESIAN_POINT('',(19.813823753501,93.8,-58.3521897074453));
#60444=CARTESIAN_POINT('',(19.813823753501,93.8,-58.3521897074453));
#60445=CARTESIAN_POINT('',(17.5586922081897,93.8,-60.154331501721));
#60446=CARTESIAN_POINT('',(17.5586922081897,93.8,-60.154331501721));
#60447=CARTESIAN_POINT('',(17.9918270105984,93.8,-63.008403605974));
#60448=CARTESIAN_POINT('',(17.9918270105984,93.8,-63.008403605974));
#60449=CARTESIAN_POINT('',(20.6800933583184,93.8,-64.0603339159514));
#60450=CARTESIAN_POINT('',(20.6800933583184,93.8,-64.0603339159514));
#60451=CARTESIAN_POINT('',(22.9352249036298,93.8,-62.2581921216758));
#60452=CARTESIAN_POINT('',(15.5177692534279,93.8,-56.6711249030688));
#60453=CARTESIAN_POINT('',(15.9509040558366,93.8,-59.5251970073219));
#60454=CARTESIAN_POINT('',(15.5177692534279,93.8,-56.6711249030688));
#60455=CARTESIAN_POINT('',(12.8295029057079,93.8,-55.6191945930914));
#60456=CARTESIAN_POINT('',(12.8295029057079,93.8,-55.6191945930914));
#60457=CARTESIAN_POINT('',(10.5743713603965,93.8,-57.4213363873671));
#60458=CARTESIAN_POINT('',(10.5743713603965,93.8,-57.4213363873671));
#60459=CARTESIAN_POINT('',(11.0075061628053,93.8,-60.2754084916201));
#60460=CARTESIAN_POINT('',(11.0075061628053,93.8,-60.2754084916201));
#60461=CARTESIAN_POINT('',(13.6957725105253,93.8,-61.3273388015976));
#60462=CARTESIAN_POINT('',(13.6957725105253,93.8,-61.3273388015976));
#60463=CARTESIAN_POINT('',(15.9509040558366,93.8,-59.5251970073219));
#60464=CARTESIAN_POINT('',(8.53344840563478,93.8,-53.9381297887149));
#60465=CARTESIAN_POINT('',(8.9665832080435,93.8,-56.792201892968));
#60466=CARTESIAN_POINT('',(8.53344840563478,93.8,-53.9381297887149));
#60467=CARTESIAN_POINT('',(5.84518205791477,93.8,-52.8861994787375));
#60468=CARTESIAN_POINT('',(5.84518205791477,93.8,-52.8861994787375));
#60469=CARTESIAN_POINT('',(3.59005051260342,93.8,-54.6883412730132));
#60470=CARTESIAN_POINT('',(3.59005051260342,93.8,-54.6883412730132));
#60471=CARTESIAN_POINT('',(4.02318531501215,93.8,-57.5424133772663));
#60472=CARTESIAN_POINT('',(4.02318531501215,93.8,-57.5424133772663));
#60473=CARTESIAN_POINT('',(6.71145166273218,93.8,-58.5943436872437));
#60474=CARTESIAN_POINT('',(6.71145166273218,93.8,-58.5943436872437));
#60475=CARTESIAN_POINT('',(8.9665832080435,93.8,-56.792201892968));
#60476=CARTESIAN_POINT('',(1.54912755784165,93.8,-51.205134674361));
#60477=CARTESIAN_POINT('',(1.98226236025037,93.8,-54.0592067786141));
#60478=CARTESIAN_POINT('',(1.54912755784165,93.8,-51.205134674361));
#60479=CARTESIAN_POINT('',(-1.13913878987836,93.8,-50.1532043643836));
#60480=CARTESIAN_POINT('',(-1.13913878987836,93.8,-50.1532043643836));
#60481=CARTESIAN_POINT('',(-3.39427033518972,93.8,-51.9553461586593));
#60482=CARTESIAN_POINT('',(-3.39427033518972,93.8,-51.9553461586593));
#60483=CARTESIAN_POINT('',(-2.96113553278099,93.8,-54.8094182629124));
#60484=CARTESIAN_POINT('',(-2.96113553278099,93.8,-54.8094182629124));
#60485=CARTESIAN_POINT('',(-0.272869185060958,93.8,-55.8613485728898));
#60486=CARTESIAN_POINT('',(-0.272869185060958,93.8,-55.8613485728898));
#60487=CARTESIAN_POINT('',(1.98226236025037,93.8,-54.0592067786141));
#60488=CARTESIAN_POINT('',(-5.43519328995148,93.8,-48.4721395600071));
#60489=CARTESIAN_POINT('',(-5.00205848754277,93.8,-51.3262116642602));
#60490=CARTESIAN_POINT('',(-5.43519328995148,93.8,-48.4721395600071));
#60491=CARTESIAN_POINT('',(-8.12345963767149,93.8,-47.4202092500297));
#60492=CARTESIAN_POINT('',(-8.12345963767149,93.8,-47.4202092500297));
#60493=CARTESIAN_POINT('',(-10.3785911829829,93.8,-49.2223510443054));
#60494=CARTESIAN_POINT('',(-10.3785911829829,93.8,-49.2223510443054));
#60495=CARTESIAN_POINT('',(-9.94545638057412,93.8,-52.0764231485585));
#60496=CARTESIAN_POINT('',(-9.94545638057412,93.8,-52.0764231485585));
#60497=CARTESIAN_POINT('',(-7.25719003285409,93.8,-53.1283534585359));
#60498=CARTESIAN_POINT('',(-7.25719003285409,93.8,-53.1283534585359));
#60499=CARTESIAN_POINT('',(-5.00205848754277,93.8,-51.3262116642602));
#60500=CARTESIAN_POINT('',(-12.4195141377446,93.8,-45.7391444456532));
#60501=CARTESIAN_POINT('',(-11.9863793353359,93.8,-48.5932165499063));
#60502=CARTESIAN_POINT('',(-12.4195141377446,93.8,-45.7391444456532));
#60503=CARTESIAN_POINT('',(-15.1077804854646,93.8,-44.6872141356758));
#60504=CARTESIAN_POINT('',(-15.1077804854646,93.8,-44.6872141356758));
#60505=CARTESIAN_POINT('',(-17.362912030776,93.8,-46.4893559299515));
#60506=CARTESIAN_POINT('',(-17.362912030776,93.8,-46.4893559299515));
#60507=CARTESIAN_POINT('',(-16.9297772283673,93.8,-49.3434280342046));
#60508=CARTESIAN_POINT('',(-16.9297772283673,93.8,-49.3434280342046));
#60509=CARTESIAN_POINT('',(-14.2415108806472,93.8,-50.395358344182));
#60510=CARTESIAN_POINT('',(-14.2415108806472,93.8,-50.395358344182));
#60511=CARTESIAN_POINT('',(-11.9863793353359,93.8,-48.5932165499063));
#60512=CARTESIAN_POINT('',(23.6274073276684,93.8,-66.8192168569697));
#60513=CARTESIAN_POINT('',(24.0605421300771,93.8,-69.6732889612228));
#60514=CARTESIAN_POINT('',(23.6274073276684,93.8,-66.8192168569697));
#60515=CARTESIAN_POINT('',(20.9391409799484,93.8,-65.7672865469923));
#60516=CARTESIAN_POINT('',(20.9391409799484,93.8,-65.7672865469923));
#60517=CARTESIAN_POINT('',(18.684009434637,93.8,-67.569428341268));
#60518=CARTESIAN_POINT('',(18.684009434637,93.8,-67.569428341268));
#60519=CARTESIAN_POINT('',(19.1171442370458,93.8,-70.4235004455211));
#60520=CARTESIAN_POINT('',(19.1171442370458,93.8,-70.4235004455211));
#60521=CARTESIAN_POINT('',(21.8054105847658,93.8,-71.4754307554985));
#60522=CARTESIAN_POINT('',(21.8054105847658,93.8,-71.4754307554985));
#60523=CARTESIAN_POINT('',(24.0605421300771,93.8,-69.6732889612228));
#60524=CARTESIAN_POINT('',(30.6117281754615,93.8,-69.5522119713236));
#60525=CARTESIAN_POINT('',(31.0448629778703,93.8,-72.4062840755767));
#60526=CARTESIAN_POINT('',(30.6117281754615,93.8,-69.5522119713236));
#60527=CARTESIAN_POINT('',(27.9234618277415,93.8,-68.5002816613462));
#60528=CARTESIAN_POINT('',(27.9234618277415,93.8,-68.5002816613462));
#60529=CARTESIAN_POINT('',(25.6683302824302,93.8,-70.3024234556219));
#60530=CARTESIAN_POINT('',(25.6683302824302,93.8,-70.3024234556219));
#60531=CARTESIAN_POINT('',(26.1014650848389,93.8,-73.156495559875));
#60532=CARTESIAN_POINT('',(26.1014650848389,93.8,-73.156495559875));
#60533=CARTESIAN_POINT('',(28.7897314325589,93.8,-74.2084258698524));
#60534=CARTESIAN_POINT('',(28.7897314325589,93.8,-74.2084258698524));
#60535=CARTESIAN_POINT('',(31.0448629778703,93.8,-72.4062840755767));
#60536=CARTESIAN_POINT('',(37.5960490232547,93.8,-72.2852070856775));
#60537=CARTESIAN_POINT('',(38.0291838256634,93.8,-75.1392791899306));
#60538=CARTESIAN_POINT('',(37.5960490232547,93.8,-72.2852070856775));
#60539=CARTESIAN_POINT('',(34.9077826755347,93.8,-71.2332767757001));
#60540=CARTESIAN_POINT('',(34.9077826755347,93.8,-71.2332767757001));
#60541=CARTESIAN_POINT('',(32.6526511302233,93.8,-73.0354185699758));
#60542=CARTESIAN_POINT('',(32.6526511302233,93.8,-73.0354185699758));
#60543=CARTESIAN_POINT('',(33.085785932632,93.8,-75.8894906742289));
#60544=CARTESIAN_POINT('',(33.085785932632,93.8,-75.8894906742289));
#60545=CARTESIAN_POINT('',(35.7740522803521,93.8,-76.9414209842063));
#60546=CARTESIAN_POINT('',(35.7740522803521,93.8,-76.9414209842063));
#60547=CARTESIAN_POINT('',(38.0291838256634,93.8,-75.1392791899306));
#60548=CARTESIAN_POINT('',(44.5803698710478,93.8,-75.0182022000314));
#60549=CARTESIAN_POINT('',(45.0135046734565,93.8,-77.8722743042845));
#60550=CARTESIAN_POINT('',(44.5803698710478,93.8,-75.0182022000314));
#60551=CARTESIAN_POINT('',(41.8921035233278,93.8,-73.966271890054));
#60552=CARTESIAN_POINT('',(41.8921035233278,93.8,-73.966271890054));
#60553=CARTESIAN_POINT('',(39.6369719780164,93.8,-75.7684136843297));
#60554=CARTESIAN_POINT('',(39.6369719780164,93.8,-75.7684136843297));
#60555=CARTESIAN_POINT('',(40.0701067804252,93.8,-78.6224857885828));
#60556=CARTESIAN_POINT('',(40.0701067804252,93.8,-78.6224857885828));
#60557=CARTESIAN_POINT('',(42.7583731281452,93.8,-79.6744160985602));
#60558=CARTESIAN_POINT('',(42.7583731281452,93.8,-79.6744160985602));
#60559=CARTESIAN_POINT('',(45.0135046734565,93.8,-77.8722743042845));
#60560=CARTESIAN_POINT('',(-19.4038349855377,93.8,-43.0061493312993));
#60561=CARTESIAN_POINT('',(-18.970700183129,93.8,-45.8602214355524));
#60562=CARTESIAN_POINT('',(-19.4038349855377,93.8,-43.0061493312993));
#60563=CARTESIAN_POINT('',(-22.0921013332578,93.8,-41.9542190213219));
#60564=CARTESIAN_POINT('',(-22.0921013332578,93.8,-41.9542190213219));
#60565=CARTESIAN_POINT('',(-24.3472328785691,93.8,-43.7563608155976));
#60566=CARTESIAN_POINT('',(-24.3472328785691,93.8,-43.7563608155976));
#60567=CARTESIAN_POINT('',(-23.9140980761604,93.8,-46.6104329198507));
#60568=CARTESIAN_POINT('',(-23.9140980761604,93.8,-46.6104329198507));
#60569=CARTESIAN_POINT('',(-21.2258317284404,93.8,-47.6623632298281));
#60570=CARTESIAN_POINT('',(-21.2258317284404,93.8,-47.6623632298281));
#60571=CARTESIAN_POINT('',(-18.970700183129,93.8,-45.8602214355524));
#60572=CARTESIAN_POINT('',(-26.3881558333309,93.8,-40.2731542169454));
#60573=CARTESIAN_POINT('',(-25.9550210309222,93.8,-43.1272263211985));
#60574=CARTESIAN_POINT('',(-26.3881558333309,93.8,-40.2731542169454));
#60575=CARTESIAN_POINT('',(-29.0764221810509,93.8,-39.221223906968));
#60576=CARTESIAN_POINT('',(-29.0764221810509,93.8,-39.221223906968));
#60577=CARTESIAN_POINT('',(-31.3315537263622,93.8,-41.0233657012437));
#60578=CARTESIAN_POINT('',(-31.3315537263622,93.8,-41.0233657012437));
#60579=CARTESIAN_POINT('',(-30.8984189239535,93.8,-43.8774378054968));
#60580=CARTESIAN_POINT('',(-30.8984189239535,93.8,-43.8774378054968));
#60581=CARTESIAN_POINT('',(-28.2101525762335,93.8,-44.9293681154742));
#60582=CARTESIAN_POINT('',(-28.2101525762335,93.8,-44.9293681154742));
#60583=CARTESIAN_POINT('',(-25.9550210309222,93.8,-43.1272263211986));
#60584=CARTESIAN_POINT('',(-33.372476681124,93.8,-37.5401591025916));
#60585=CARTESIAN_POINT('',(-32.9393418787153,93.8,-40.3942312068447));
#60586=CARTESIAN_POINT('',(-33.372476681124,93.8,-37.5401591025916));
#60587=CARTESIAN_POINT('',(-36.060743028844,93.8,-36.4882287926142));
#60588=CARTESIAN_POINT('',(-36.060743028844,93.8,-36.4882287926142));
#60589=CARTESIAN_POINT('',(-38.3158745741554,93.8,-38.2903705868898));
#60590=CARTESIAN_POINT('',(-38.3158745741554,93.8,-38.2903705868898));
#60591=CARTESIAN_POINT('',(-37.8827397717466,93.8,-41.1444426911429));
#60592=CARTESIAN_POINT('',(-37.8827397717466,93.8,-41.1444426911429));
#60593=CARTESIAN_POINT('',(-35.1944734240266,93.8,-42.1963730011203));
#60594=CARTESIAN_POINT('',(-35.1944734240266,93.8,-42.1963730011203));
#60595=CARTESIAN_POINT('',(-32.9393418787153,93.8,-40.3942312068447));
#60596=CARTESIAN_POINT('',(51.5646907188409,93.8,-77.7511973143853));
#60597=CARTESIAN_POINT('',(51.9978255212496,93.8,-80.6052694186384));
#60598=CARTESIAN_POINT('',(51.5646907188409,93.8,-77.7511973143853));
#60599=CARTESIAN_POINT('',(48.8764243711209,93.8,-76.6992670044079));
#60600=CARTESIAN_POINT('',(48.8764243711209,93.8,-76.6992670044079));
#60601=CARTESIAN_POINT('',(46.6212928258096,93.8,-78.5014087986836));
#60602=CARTESIAN_POINT('',(46.6212928258096,93.8,-78.5014087986836));
#60603=CARTESIAN_POINT('',(47.0544276282183,93.8,-81.3554809029366));
#60604=CARTESIAN_POINT('',(47.0544276282183,93.8,-81.3554809029366));
#60605=CARTESIAN_POINT('',(49.7426939759383,93.8,-82.4074112129141));
#60606=CARTESIAN_POINT('',(49.7426939759383,93.8,-82.4074112129141));
#60607=CARTESIAN_POINT('',(51.9978255212496,93.8,-80.6052694186384));
#60608=CARTESIAN_POINT('',(14.3924520269805,93.8,-49.2560280635217));
#60609=CARTESIAN_POINT('',(14.8255868293893,93.8,-52.1101001677748));
#60610=CARTESIAN_POINT('',(14.3924520269805,93.8,-49.2560280635217));
#60611=CARTESIAN_POINT('',(11.7041856792605,93.8,-48.2040977535443));
#60612=CARTESIAN_POINT('',(11.7041856792605,93.8,-48.2040977535443));
#60613=CARTESIAN_POINT('',(9.44905413394917,93.8,-50.00623954782));
#60614=CARTESIAN_POINT('',(9.44905413394917,93.8,-50.00623954782));
#60615=CARTESIAN_POINT('',(9.8821889363579,93.8,-52.8603116520731));
#60616=CARTESIAN_POINT('',(9.8821889363579,93.8,-52.8603116520731));
#60617=CARTESIAN_POINT('',(12.5704552840779,93.8,-53.9122419620505));
#60618=CARTESIAN_POINT('',(12.5704552840779,93.8,-53.9122419620505));
#60619=CARTESIAN_POINT('',(14.8255868293893,93.8,-52.1101001677748));
#60620=CARTESIAN_POINT('',(21.3767728747737,93.8,-51.9890231778756));
#60621=CARTESIAN_POINT('',(21.8099076771824,93.8,-54.8430952821287));
#60622=CARTESIAN_POINT('',(21.3767728747737,93.8,-51.9890231778756));
#60623=CARTESIAN_POINT('',(18.6885065270537,93.8,-50.9370928678982));
#60624=CARTESIAN_POINT('',(18.6885065270537,93.8,-50.9370928678982));
#60625=CARTESIAN_POINT('',(16.4333749817423,93.8,-52.7392346621739));
#60626=CARTESIAN_POINT('',(16.4333749817423,93.8,-52.7392346621739));
#60627=CARTESIAN_POINT('',(16.866509784151,93.8,-55.593306766427));
#60628=CARTESIAN_POINT('',(16.866509784151,93.8,-55.593306766427));
#60629=CARTESIAN_POINT('',(19.5547761318711,93.8,-56.6452370764044));
#60630=CARTESIAN_POINT('',(19.5547761318711,93.8,-56.6452370764044));
#60631=CARTESIAN_POINT('',(21.8099076771824,93.8,-54.8430952821287));
#60632=CARTESIAN_POINT('',(28.3610937225668,93.8,-54.7220182922295));
#60633=CARTESIAN_POINT('',(28.7942285249755,93.8,-57.5760903964826));
#60634=CARTESIAN_POINT('',(28.3610937225668,93.8,-54.7220182922295));
#60635=CARTESIAN_POINT('',(25.6728273748468,93.8,-53.6700879822521));
#60636=CARTESIAN_POINT('',(25.6728273748468,93.8,-53.6700879822521));
#60637=CARTESIAN_POINT('',(23.4176958295354,93.8,-55.4722297765278));
#60638=CARTESIAN_POINT('',(23.4176958295354,93.8,-55.4722297765278));
#60639=CARTESIAN_POINT('',(23.8508306319442,93.8,-58.3263018807808));
#60640=CARTESIAN_POINT('',(23.8508306319442,93.8,-58.3263018807808));
#60641=CARTESIAN_POINT('',(26.5390969796642,93.8,-59.3782321907583));
#60642=CARTESIAN_POINT('',(26.5390969796642,93.8,-59.3782321907583));
#60643=CARTESIAN_POINT('',(28.7942285249755,93.8,-57.5760903964826));
#60644=CARTESIAN_POINT('',(35.3454145703599,93.8,-57.4550134065834));
#60645=CARTESIAN_POINT('',(35.7785493727686,93.8,-60.3090855108365));
#60646=CARTESIAN_POINT('',(35.3454145703599,93.8,-57.4550134065834));
#60647=CARTESIAN_POINT('',(32.6571482226399,93.8,-56.403083096606));
#60648=CARTESIAN_POINT('',(32.6571482226399,93.8,-56.403083096606));
#60649=CARTESIAN_POINT('',(30.4020166773286,93.8,-58.2052248908817));
#60650=CARTESIAN_POINT('',(30.4020166773286,93.8,-58.2052248908817));
#60651=CARTESIAN_POINT('',(30.8351514797373,93.8,-61.0592969951347));
#60652=CARTESIAN_POINT('',(30.8351514797373,93.8,-61.0592969951347));
#60653=CARTESIAN_POINT('',(33.5234178274573,93.8,-62.1112273051122));
#60654=CARTESIAN_POINT('',(33.5234178274573,93.8,-62.1112273051122));
#60655=CARTESIAN_POINT('',(35.7785493727686,93.8,-60.3090855108365));
#60656=CARTESIAN_POINT('',(42.3297354181531,93.8,-60.1880085209373));
#60657=CARTESIAN_POINT('',(42.7628702205618,93.8,-63.0420806251904));
#60658=CARTESIAN_POINT('',(42.3297354181531,93.8,-60.1880085209373));
#60659=CARTESIAN_POINT('',(39.641469070433,93.8,-59.1360782109599));
#60660=CARTESIAN_POINT('',(39.641469070433,93.8,-59.1360782109599));
#60661=CARTESIAN_POINT('',(37.3863375251217,93.8,-60.9382200052356));
#60662=CARTESIAN_POINT('',(37.3863375251217,93.8,-60.9382200052356));
#60663=CARTESIAN_POINT('',(37.8194723275304,93.8,-63.7922921094886));
#60664=CARTESIAN_POINT('',(37.8194723275304,93.8,-63.7922921094886));
#60665=CARTESIAN_POINT('',(40.5077386752504,93.8,-64.844222419466));
#60666=CARTESIAN_POINT('',(40.5077386752504,93.8,-64.844222419466));
#60667=CARTESIAN_POINT('',(42.7628702205618,93.8,-63.0420806251904));
#60668=CARTESIAN_POINT('',(49.3140562659462,93.8,-62.9210036352912));
#60669=CARTESIAN_POINT('',(49.7471910683549,93.8,-65.7750757395443));
#60670=CARTESIAN_POINT('',(49.3140562659462,93.8,-62.9210036352912));
#60671=CARTESIAN_POINT('',(46.6257899182262,93.8,-61.8690733253138));
#60672=CARTESIAN_POINT('',(46.6257899182262,93.8,-61.8690733253138));
#60673=CARTESIAN_POINT('',(44.3706583729148,93.8,-63.6712151195895));
#60674=CARTESIAN_POINT('',(44.3706583729148,93.8,-63.6712151195895));
#60675=CARTESIAN_POINT('',(44.8037931753235,93.8,-66.5252872238425));
#60676=CARTESIAN_POINT('',(44.8037931753235,93.8,-66.5252872238425));
#60677=CARTESIAN_POINT('',(47.4920595230436,93.8,-67.5772175338199));
#60678=CARTESIAN_POINT('',(47.4920595230436,93.8,-67.5772175338199));
#60679=CARTESIAN_POINT('',(49.7471910683549,93.8,-65.7750757395443));
#60680=CARTESIAN_POINT('',(-21.6544694384325,93.8,-28.1759556522052));
#60681=CARTESIAN_POINT('',(-21.2213346360238,93.8,-31.0300277564583));
#60682=CARTESIAN_POINT('',(-21.6544694384325,93.8,-28.1759556522052));
#60683=CARTESIAN_POINT('',(-24.3427357861525,93.8,-27.1240253422278));
#60684=CARTESIAN_POINT('',(-24.3427357861525,93.8,-27.1240253422278));
#60685=CARTESIAN_POINT('',(-26.5978673314639,93.8,-28.9261671365035));
#60686=CARTESIAN_POINT('',(-26.5978673314639,93.8,-28.9261671365035));
#60687=CARTESIAN_POINT('',(-26.1647325290551,93.8,-31.7802392407566));
#60688=CARTESIAN_POINT('',(-26.1647325290551,93.8,-31.7802392407566));
#60689=CARTESIAN_POINT('',(-23.4764661813351,93.8,-32.832169550734));
#60690=CARTESIAN_POINT('',(-23.4764661813351,93.8,-32.832169550734));
#60691=CARTESIAN_POINT('',(-21.2213346360238,93.8,-31.0300277564583));
#60692=CARTESIAN_POINT('',(-14.6701485906394,93.8,-30.9089507665591));
#60693=CARTESIAN_POINT('',(-14.2370137882306,93.8,-33.7630228708122));
#60694=CARTESIAN_POINT('',(-14.6701485906394,93.8,-30.9089507665591));
#60695=CARTESIAN_POINT('',(-17.3584149383594,93.8,-29.8570204565817));
#60696=CARTESIAN_POINT('',(-17.3584149383594,93.8,-29.8570204565817));
#60697=CARTESIAN_POINT('',(-19.6135464836707,93.8,-31.6591622508574));
#60698=CARTESIAN_POINT('',(-19.6135464836707,93.8,-31.6591622508574));
#60699=CARTESIAN_POINT('',(-19.180411681262,93.8,-34.5132343551105));
#60700=CARTESIAN_POINT('',(-19.180411681262,93.8,-34.5132343551105));
#60701=CARTESIAN_POINT('',(-16.492145333542,93.8,-35.5651646650879));
#60702=CARTESIAN_POINT('',(-16.492145333542,93.8,-35.5651646650879));
#60703=CARTESIAN_POINT('',(-14.2370137882306,93.8,-33.7630228708122));
#60704=CARTESIAN_POINT('',(43.4550526446004,93.8,-67.6031053604843));
#60705=CARTESIAN_POINT('',(43.8881874470091,93.8,-70.4571774647375));
#60706=CARTESIAN_POINT('',(43.4550526446004,93.8,-67.6031053604843));
#60707=CARTESIAN_POINT('',(40.7667862968804,93.8,-66.5511750505069));
#60708=CARTESIAN_POINT('',(40.7667862968804,93.8,-66.5511750505069));
#60709=CARTESIAN_POINT('',(38.5116547515691,93.8,-68.3533168447826));
#60710=CARTESIAN_POINT('',(38.5116547515691,93.8,-68.3533168447826));
#60711=CARTESIAN_POINT('',(38.9447895539778,93.8,-71.2073889490357));
#60712=CARTESIAN_POINT('',(38.9447895539778,93.8,-71.2073889490357));
#60713=CARTESIAN_POINT('',(41.6330559016978,93.8,-72.2593192590131));
#60714=CARTESIAN_POINT('',(41.6330559016978,93.8,-72.2593192590131));
#60715=CARTESIAN_POINT('',(43.8881874470091,93.8,-70.4571774647375));
#60716=CARTESIAN_POINT('',(50.4393734923936,93.8,-70.3361004748382));
#60717=CARTESIAN_POINT('',(50.8725082948023,93.8,-73.1901725790914));
#60718=CARTESIAN_POINT('',(50.4393734923936,93.8,-70.3361004748382));
#60719=CARTESIAN_POINT('',(47.7511071446736,93.8,-69.2841701648608));
#60720=CARTESIAN_POINT('',(47.7511071446736,93.8,-69.2841701648608));
#60721=CARTESIAN_POINT('',(45.4959755993622,93.8,-71.0863119591365));
#60722=CARTESIAN_POINT('',(45.4959755993622,93.8,-71.0863119591365));
#60723=CARTESIAN_POINT('',(45.9291104017709,93.8,-73.9403840633896));
#60724=CARTESIAN_POINT('',(45.9291104017709,93.8,-73.9403840633896));
#60725=CARTESIAN_POINT('',(48.617376749491,93.8,-74.992314373367));
#60726=CARTESIAN_POINT('',(48.617376749491,93.8,-74.992314373367));
#60727=CARTESIAN_POINT('',(50.8725082948023,93.8,-73.1901725790914));
#60728=CARTESIAN_POINT('',(-27.5134730597783,93.8,-32.8580573773984));
#60729=CARTESIAN_POINT('',(-27.0803382573695,93.8,-35.7121294816515));
#60730=CARTESIAN_POINT('',(-27.5134730597783,93.8,-32.8580573773984));
#60731=CARTESIAN_POINT('',(-30.2017394074983,93.8,-31.806127067421));
#60732=CARTESIAN_POINT('',(-30.2017394074983,93.8,-31.806127067421));
#60733=CARTESIAN_POINT('',(-32.4568709528096,93.8,-33.6082688616967));
#60734=CARTESIAN_POINT('',(-32.4568709528096,93.8,-33.6082688616967));
#60735=CARTESIAN_POINT('',(-32.0237361504009,93.8,-36.4623409659497));
#60736=CARTESIAN_POINT('',(-32.0237361504009,93.8,-36.4623409659497));
#60737=CARTESIAN_POINT('',(-29.3354698026809,93.8,-37.5142712759272));
#60738=CARTESIAN_POINT('',(-29.3354698026809,93.8,-37.5142712759272));
#60739=CARTESIAN_POINT('',(-27.0803382573695,93.8,-35.7121294816515));
#60740=CARTESIAN_POINT('',(-20.5291522119851,93.8,-35.5910524917523));
#60741=CARTESIAN_POINT('',(-20.0960174095764,93.8,-38.4451245960054));
#60742=CARTESIAN_POINT('',(-20.5291522119851,93.8,-35.5910524917523));
#60743=CARTESIAN_POINT('',(-23.2174185597051,93.8,-34.5391221817749));
#60744=CARTESIAN_POINT('',(-23.2174185597051,93.8,-34.5391221817749));
#60745=CARTESIAN_POINT('',(-25.4725501050165,93.8,-36.3412639760506));
#60746=CARTESIAN_POINT('',(-25.4725501050165,93.8,-36.3412639760506));
#60747=CARTESIAN_POINT('',(-25.0394153026078,93.8,-39.1953360803036));
#60748=CARTESIAN_POINT('',(-25.0394153026078,93.8,-39.1953360803036));
#60749=CARTESIAN_POINT('',(-22.3511489548877,93.8,-40.2472663902811));
#60750=CARTESIAN_POINT('',(-22.3511489548877,93.8,-40.2472663902811));
#60751=CARTESIAN_POINT('',(-20.0960174095764,93.8,-38.4451245960054));
#60752=CARTESIAN_POINT('',(-13.544831364192,93.8,-38.3240476061062));
#60753=CARTESIAN_POINT('',(-13.1116965617833,93.8,-41.1781197103593));
#60754=CARTESIAN_POINT('',(-13.544831364192,93.8,-38.3240476061062));
#60755=CARTESIAN_POINT('',(-16.233097711912,93.8,-37.2721172961288));
#60756=CARTESIAN_POINT('',(-16.233097711912,93.8,-37.2721172961288));
#60757=CARTESIAN_POINT('',(-18.4882292572234,93.8,-39.0742590904044));
#60758=CARTESIAN_POINT('',(-18.4882292572234,93.8,-39.0742590904044));
#60759=CARTESIAN_POINT('',(-18.0550944548146,93.8,-41.9283311946575));
#60760=CARTESIAN_POINT('',(-18.0550944548146,93.8,-41.9283311946575));
#60761=CARTESIAN_POINT('',(-15.3668281070946,93.8,-42.9802615046349));
#60762=CARTESIAN_POINT('',(-15.3668281070946,93.8,-42.9802615046349));
#60763=CARTESIAN_POINT('',(-13.1116965617833,93.8,-41.1781197103593));
#60764=CARTESIAN_POINT('',(-6.56051051639886,93.8,-41.0570427204601));
#60765=CARTESIAN_POINT('',(-6.12737571399014,93.8,-43.9111148247132));
#60766=CARTESIAN_POINT('',(-6.56051051639886,93.8,-41.0570427204601));
#60767=CARTESIAN_POINT('',(-9.24877686411887,93.8,-40.0051124104826));
#60768=CARTESIAN_POINT('',(-9.24877686411887,93.8,-40.0051124104826));
#60769=CARTESIAN_POINT('',(-11.5039084094302,93.8,-41.8072542047583));
#60770=CARTESIAN_POINT('',(-11.5039084094302,93.8,-41.8072542047583));
#60771=CARTESIAN_POINT('',(-11.0707736070215,93.8,-44.6613263090114));
#60772=CARTESIAN_POINT('',(-11.0707736070215,93.8,-44.6613263090114));
#60773=CARTESIAN_POINT('',(-8.38250725930147,93.8,-45.7132566189888));
#60774=CARTESIAN_POINT('',(-8.38250725930147,93.8,-45.7132566189888));
#60775=CARTESIAN_POINT('',(-6.12737571399014,93.8,-43.9111148247132));
#60776=CARTESIAN_POINT('',(0.423810331394273,93.8,-43.7900378348139));
#60777=CARTESIAN_POINT('',(0.856945133802991,93.8,-46.6441099390671));
#60778=CARTESIAN_POINT('',(0.423810331394273,93.8,-43.7900378348139));
#60779=CARTESIAN_POINT('',(-2.26445601632574,93.8,-42.7381075248365));
#60780=CARTESIAN_POINT('',(-2.26445601632574,93.8,-42.7381075248365));
#60781=CARTESIAN_POINT('',(-4.51958756163709,93.8,-44.5402493191122));
#60782=CARTESIAN_POINT('',(-4.51958756163709,93.8,-44.5402493191122));
#60783=CARTESIAN_POINT('',(-4.08645275922836,93.8,-47.3943214233653));
#60784=CARTESIAN_POINT('',(-4.08645275922836,93.8,-47.3943214233653));
#60785=CARTESIAN_POINT('',(-1.39818641150833,93.8,-48.4462517333427));
#60786=CARTESIAN_POINT('',(-1.39818641150833,93.8,-48.4462517333427));
#60787=CARTESIAN_POINT('',(0.856945133802991,93.8,-46.6441099390671));
#60788=CARTESIAN_POINT('',(7.40813117918741,93.8,-46.5230329491678));
#60789=CARTESIAN_POINT('',(7.84126598159612,93.8,-49.3771050534209));
#60790=CARTESIAN_POINT('',(7.40813117918741,93.8,-46.5230329491678));
#60791=CARTESIAN_POINT('',(4.7198648314674,93.8,-45.4711026391904));
#60792=CARTESIAN_POINT('',(4.7198648314674,93.8,-45.4711026391904));
#60793=CARTESIAN_POINT('',(2.46473328615604,93.8,-47.2732444334661));
#60794=CARTESIAN_POINT('',(2.46473328615604,93.8,-47.2732444334661));
#60795=CARTESIAN_POINT('',(2.89786808856477,93.8,-50.1273165377192));
#60796=CARTESIAN_POINT('',(2.89786808856477,93.8,-50.1273165377192));
#60797=CARTESIAN_POINT('',(5.5861344362848,93.8,-51.1792468476966));
#60798=CARTESIAN_POINT('',(5.5861344362848,93.8,-51.1792468476966));
#60799=CARTESIAN_POINT('',(7.84126598159612,93.8,-49.3771050534209));
#60800=CARTESIAN_POINT('',(-34.9626288857891,93.8,-113.640234108901));
#60801=CARTESIAN_POINT('',(-34.5294940833804,93.8,-116.494306213155));
#60802=CARTESIAN_POINT('',(-34.9626288857891,93.8,-113.640234108901));
#60803=CARTESIAN_POINT('',(-37.6508952335091,93.8,-112.588303798924));
#60804=CARTESIAN_POINT('',(-37.6508952335091,93.8,-112.588303798924));
#60805=CARTESIAN_POINT('',(-39.9060267788205,93.8,-114.3904455932));
#60806=CARTESIAN_POINT('',(-39.9060267788205,93.8,-114.3904455932));
#60807=CARTESIAN_POINT('',(-39.4728919764118,93.8,-117.244517697453));
#60808=CARTESIAN_POINT('',(-39.4728919764118,93.8,-117.244517697453));
#60809=CARTESIAN_POINT('',(-36.7846256286917,93.8,-118.29644800743));
#60810=CARTESIAN_POINT('',(-36.7846256286917,93.8,-118.29644800743));
#60811=CARTESIAN_POINT('',(-34.5294940833804,93.8,-116.494306213155));
#60812=CARTESIAN_POINT('',(-27.978308037996,93.8,-116.373229223255));
#60813=CARTESIAN_POINT('',(-27.5451732355873,93.8,-119.227301327508));
#60814=CARTESIAN_POINT('',(-27.978308037996,93.8,-116.373229223255));
#60815=CARTESIAN_POINT('',(-30.666574385716,93.8,-115.321298913278));
#60816=CARTESIAN_POINT('',(-30.666574385716,93.8,-115.321298913278));
#60817=CARTESIAN_POINT('',(-32.9217059310274,93.8,-117.123440707554));
#60818=CARTESIAN_POINT('',(-32.9217059310274,93.8,-117.123440707554));
#60819=CARTESIAN_POINT('',(-32.4885711286186,93.8,-119.977512811807));
#60820=CARTESIAN_POINT('',(-32.4885711286186,93.8,-119.977512811807));
#60821=CARTESIAN_POINT('',(-29.8003047808986,93.8,-121.029443121784));
#60822=CARTESIAN_POINT('',(-29.8003047808986,93.8,-121.029443121784));
#60823=CARTESIAN_POINT('',(-27.5451732355873,93.8,-119.227301327508));
#60824=CARTESIAN_POINT('Origin',(0.,93.,-77.5000000000001));
#60825=CARTESIAN_POINT('',(-24.5751532752614,93.,-68.8816112651563));
#60826=CARTESIAN_POINT('',(-21.8868869275414,93.,-69.9335415751337));
#60827=CARTESIAN_POINT('',(-0.338657290464793,93.,-78.3654575200768));
#60828=CARTESIAN_POINT('',(-21.4537521251327,93.,-72.7876136793868));
#60829=CARTESIAN_POINT('',(-20.271717355013,93.,-80.5764416490967));
#60830=CARTESIAN_POINT('',(-23.708883670444,93.,-74.5897554736624));
#60831=CARTESIAN_POINT('',(-10.65925517077,93.,-64.1614144006423));
#60832=CARTESIAN_POINT('',(-26.397150018164,93.,-73.537825163685));
#60833=CARTESIAN_POINT('',(-2.16065403336742,93.,-83.0216714186056));
#60834=CARTESIAN_POINT('',(-26.8302848205727,93.,-70.683753059432));
#60835=CARTESIAN_POINT('',(-25.2151152480443,93.,-81.3266531333951));
#60836=CARTESIAN_POINT('',(-13.7806563208988,93.,-60.2554119864118));
#60837=CARTESIAN_POINT('',(-17.5908324274683,93.,-71.6146063795101));
#60838=CARTESIAN_POINT('',(-14.9025660797482,93.,-72.6665366894876));
#60839=CARTESIAN_POINT('',(-0.338657290464798,93.,-78.3654575200768));
#60840=CARTESIAN_POINT('',(-14.4694312773395,93.,-75.5206087937407));
#60841=CARTESIAN_POINT('',(-13.8500551204435,93.,-79.6018883436771));
#60842=CARTESIAN_POINT('',(-16.7245628226509,93.,-77.3227505880163));
#60843=CARTESIAN_POINT('',(-6.60443613364973,93.,-69.2354603775928));
#60844=CARTESIAN_POINT('',(-19.4128291703709,93.,-76.2708202780389));
#60845=CARTESIAN_POINT('',(-2.16065403336742,93.,-83.0216714186056));
#60846=CARTESIAN_POINT('',(-19.8459639727796,93.,-73.4167481737858));
#60847=CARTESIAN_POINT('',(-18.7934530134748,93.,-80.3520998279754));
#60848=CARTESIAN_POINT('',(-9.72583728377851,93.,-65.3294579633623));
#60849=CARTESIAN_POINT('',(-10.6065115796751,93.,-74.347601493864));
#60850=CARTESIAN_POINT('',(-7.91824523195512,93.,-75.3995318038414));
#60851=CARTESIAN_POINT('',(-0.338657290464803,93.,-78.3654575200768));
#60852=CARTESIAN_POINT('',(-7.4851104295464,93.,-78.2536039080945));
#60853=CARTESIAN_POINT('',(-7.42839288587402,93.,-78.6273350382575));
#60854=CARTESIAN_POINT('',(-9.74024197485773,93.,-80.0557457023702));
#60855=CARTESIAN_POINT('',(-2.54961709652949,93.,-74.3095063545433));
#60856=CARTESIAN_POINT('',(-12.4285083225778,93.,-79.0038153923928));
#60857=CARTESIAN_POINT('',(-2.16065403336741,93.,-83.0216714186056));
#60858=CARTESIAN_POINT('',(-12.8616431249865,93.,-76.1497432881397));
#60859=CARTESIAN_POINT('',(-12.3717907789054,93.,-79.3775465225557));
#60860=CARTESIAN_POINT('',(-5.67101824665826,93.,-70.4035039403128));
#60861=CARTESIAN_POINT('',(-3.622190731882,93.,-77.0805966082179));
#60862=CARTESIAN_POINT('',(-0.933924384161986,93.,-78.1325269181953));
#60863=CARTESIAN_POINT('',(-0.338657290464807,93.,-78.3654575200768));
#60864=CARTESIAN_POINT('',(-0.500789581753269,93.,-80.9865990224485));
#60865=CARTESIAN_POINT('',(-1.00673065130454,93.,-77.6527817328379));
#60866=CARTESIAN_POINT('',(-2.75592112706459,93.,-82.7887408167241));
#60867=CARTESIAN_POINT('',(1.50520194059076,93.,-79.3835523314938));
#60868=CARTESIAN_POINT('',(-5.44418747478462,93.,-81.7368105067467));
#60869=CARTESIAN_POINT('',(-2.16065403336741,93.,-83.0216714186056));
#60870=CARTESIAN_POINT('',(-5.87732227719335,93.,-78.8827384024936));
#60871=CARTESIAN_POINT('',(-5.95012854433591,93.,-78.4029932171361));
#60872=CARTESIAN_POINT('',(-1.61619920953801,93.,-75.4775499172633));
#60873=CARTESIAN_POINT('',(3.36213011591114,93.,-79.8135917225718));
#60874=CARTESIAN_POINT('',(6.05039646363115,93.,-80.8655220325492));
#60875=CARTESIAN_POINT('',(-0.338657290464812,93.,-78.3654575200769));
#60876=CARTESIAN_POINT('',(6.48353126603986,93.,-83.7195941368023));
#60877=CARTESIAN_POINT('',(5.41493158326495,93.,-76.6782284274182));
#60878=CARTESIAN_POINT('',(4.22839972072854,93.,-85.521735931078));
#60879=CARTESIAN_POINT('',(5.56002097771101,93.,-84.4575983084442));
#60880=CARTESIAN_POINT('',(1.54013337300851,93.,-84.4698056211006));
#60881=CARTESIAN_POINT('',(-2.16065403336741,93.,-83.0216714186056));
#60882=CARTESIAN_POINT('',(1.10699857059978,93.,-81.6157335168475));
#60883=CARTESIAN_POINT('',(0.471533690233543,93.,-77.4284399117164));
#60884=CARTESIAN_POINT('',(2.43861982758225,93.,-80.5515958942137));
#60885=CARTESIAN_POINT('',(10.3464509637043,93.,-82.5465868369257));
#60886=CARTESIAN_POINT('',(13.0347173114243,93.,-83.5985171469031));
#60887=CARTESIAN_POINT('',(-0.338657290464817,93.,-78.3654575200769));
#60888=CARTESIAN_POINT('',(13.467852113833,93.,-86.4525892511562));
#60889=CARTESIAN_POINT('',(11.8365938178344,93.,-75.7036751219986));
#60890=CARTESIAN_POINT('',(11.2127205685217,93.,-88.2547310454319));
#60891=CARTESIAN_POINT('',(9.61484001483125,93.,-89.5316442853947));
#60892=CARTESIAN_POINT('',(8.52445422080164,93.,-87.2028007354545));
#60893=CARTESIAN_POINT('',(-2.16065403336741,93.,-83.0216714186056));
#60894=CARTESIAN_POINT('',(8.09131941839291,93.,-84.3487286312014));
#60895=CARTESIAN_POINT('',(6.89319592480299,93.,-76.4538866062968));
#60896=CARTESIAN_POINT('',(6.4934388647025,93.,-85.6256418711642));
#60897=CARTESIAN_POINT('',(17.3307718114974,93.,-85.2795819512796));
#60898=CARTESIAN_POINT('',(20.0190381592174,93.,-86.331512261257));
#60899=CARTESIAN_POINT('',(-0.338657290464822,93.,-78.3654575200769));
#60900=CARTESIAN_POINT('',(20.4521729616261,93.,-89.1855843655101));
#60901=CARTESIAN_POINT('',(18.2582560524039,93.,-74.729121816579));
#60902=CARTESIAN_POINT('',(18.1970414163148,93.,-90.9877261597858));
#60903=CARTESIAN_POINT('',(13.6696590519515,93.,-94.6056902623452));
#60904=CARTESIAN_POINT('',(15.5087750685948,93.,-89.9357958498083));
#60905=CARTESIAN_POINT('',(-2.16065403336741,93.,-83.0216714186056));
#60906=CARTESIAN_POINT('',(15.075640266186,93.,-87.0817237455553));
#60907=CARTESIAN_POINT('',(13.3148581593724,93.,-75.4793333008771));
#60908=CARTESIAN_POINT('',(10.5482579018227,93.,-90.6996878481147));
#60909=CARTESIAN_POINT('',(24.3150926592905,93.,-88.0125770656335));
#60910=CARTESIAN_POINT('',(27.0033590070105,93.,-89.0645073756109));
#60911=CARTESIAN_POINT('',(-0.338657290464827,93.,-78.3654575200769));
#60912=CARTESIAN_POINT('',(27.4364938094193,93.,-91.918579479864));
#60913=CARTESIAN_POINT('',(24.6799182869734,93.,-73.7545685111594));
#60914=CARTESIAN_POINT('',(25.1813622641079,93.,-93.7207212741397));
#60915=CARTESIAN_POINT('',(17.7244780890717,93.,-99.6797362392957));
#60916=CARTESIAN_POINT('',(22.4930959163879,93.,-92.6687909641622));
#60917=CARTESIAN_POINT('',(-2.16065403336741,93.,-83.0216714186056));
#60918=CARTESIAN_POINT('',(22.0599611139792,93.,-89.8147188599092));
#60919=CARTESIAN_POINT('',(19.7365203939419,93.,-74.5047799954575));
#60920=CARTESIAN_POINT('',(14.603076938943,93.,-95.7737338250652));
#60921=CARTESIAN_POINT('',(-18.7161496539156,93.,-64.1995095399631));
#60922=CARTESIAN_POINT('',(-16.0278833061956,93.,-65.2514398499405));
#60923=CARTESIAN_POINT('',(2.02818590698441,93.,-72.3168582377067));
#60924=CARTESIAN_POINT('',(-15.5947485037869,93.,-68.1055119541936));
#60925=CARTESIAN_POINT('',(-13.8500551204436,93.,-79.6018883436771));
#60926=CARTESIAN_POINT('',(-17.8498800490982,93.,-69.9076537484693));
#60927=CARTESIAN_POINT('',(-10.65925517077,93.,-64.1614144006423));
#60928=CARTESIAN_POINT('',(-20.5381463968183,93.,-68.8557234384919));
#60929=CARTESIAN_POINT('',(0.206189164081804,93.,-76.9730721362355));
#60930=CARTESIAN_POINT('',(-20.971281199227,93.,-66.0016513342388));
#60931=CARTESIAN_POINT('',(-18.7934530134748,93.,-80.3520998279754));
#60932=CARTESIAN_POINT('',(-13.7806563208988,93.,-60.2554119864118));
#60933=CARTESIAN_POINT('',(-25.7004705017088,93.,-61.4665144256092));
#60934=CARTESIAN_POINT('',(-23.0122041539888,93.,-62.5184447355866));
#60935=CARTESIAN_POINT('',(2.02818590698442,93.,-72.3168582377067));
#60936=CARTESIAN_POINT('',(-22.57906935158,93.,-65.3725168398397));
#60937=CARTESIAN_POINT('',(-20.2717173550131,93.,-80.5764416490967));
#60938=CARTESIAN_POINT('',(-24.8342008968914,93.,-67.1746586341154));
#60939=CARTESIAN_POINT('',(-14.7140742078902,93.,-59.0873684236919));
#60940=CARTESIAN_POINT('',(-27.5224672446114,93.,-66.122728324138));
#60941=CARTESIAN_POINT('',(0.206189164081802,93.,-76.9730721362355));
#60942=CARTESIAN_POINT('',(-27.9556020470201,93.,-63.2686562198849));
#60943=CARTESIAN_POINT('',(-25.2151152480443,93.,-81.3266531333951));
#60944=CARTESIAN_POINT('',(-17.835475358019,93.,-55.1813660094614));
#60945=CARTESIAN_POINT('',(-32.6847913495019,93.,-58.7335193112553));
#60946=CARTESIAN_POINT('',(-29.9965250017819,93.,-59.7854496212327));
#60947=CARTESIAN_POINT('',(2.02818590698442,93.,-72.3168582377067));
#60948=CARTESIAN_POINT('',(-29.5633901993732,93.,-62.6395217254858));
#60949=CARTESIAN_POINT('',(-26.6933795895825,93.,-81.5509949545163));
#60950=CARTESIAN_POINT('',(-31.8185217446845,93.,-64.4416635197615));
#60951=CARTESIAN_POINT('',(-18.7688932450105,93.,-54.0133224467414));
#60952=CARTESIAN_POINT('',(-34.5067880924045,93.,-63.3897332097841));
#60953=CARTESIAN_POINT('',(0.206189164081802,93.,-76.9730721362355));
#60954=CARTESIAN_POINT('',(-34.9399228948133,93.,-60.535661105531));
#60955=CARTESIAN_POINT('',(-31.6367774826137,93.,-82.3012064388147));
#60956=CARTESIAN_POINT('',(-21.8902943951393,93.,-50.1073200325109));
#60957=CARTESIAN_POINT('',(-39.669112197295,93.,-56.0005241969014));
#60958=CARTESIAN_POINT('',(-36.980845849575,93.,-57.0524545068788));
#60959=CARTESIAN_POINT('',(2.02818590698443,93.,-72.3168582377067));
#60960=CARTESIAN_POINT('',(-36.5477110471663,93.,-59.9065266111319));
#60961=CARTESIAN_POINT('',(-33.115041824152,93.,-82.5255482599359));
#60962=CARTESIAN_POINT('',(-38.8028425924776,93.,-61.7086684054076));
#60963=CARTESIAN_POINT('',(-22.8237122821307,93.,-48.9392764697909));
#60964=CARTESIAN_POINT('',(-41.4911089401976,93.,-60.6567380954302));
#60965=CARTESIAN_POINT('',(0.2061891640818,93.,-76.9730721362355));
#60966=CARTESIAN_POINT('',(-41.9242437426064,93.,-57.8026659911771));
#60967=CARTESIAN_POINT('',(-38.0584397171832,93.,-83.2757597442344));
#60968=CARTESIAN_POINT('',(-25.9451134322595,93.,-45.0332740555604));
#60969=CARTESIAN_POINT('',(31.2994135070836,93.,-90.7455721799874));
#60970=CARTESIAN_POINT('',(33.9876798548037,93.,-91.7975024899648));
#60971=CARTESIAN_POINT('',(-0.338657290464832,93.,-78.3654575200769));
#60972=CARTESIAN_POINT('',(34.4208146572124,93.,-94.6515745942179));
#60973=CARTESIAN_POINT('',(31.1015805215429,93.,-72.7800152057398));
#60974=CARTESIAN_POINT('',(32.1656831119011,93.,-96.4537163884935));
#60975=CARTESIAN_POINT('',(21.779297126192,93.,-104.753782216246));
#60976=CARTESIAN_POINT('',(29.477416764181,93.,-95.4017860785161));
#60977=CARTESIAN_POINT('',(-2.16065403336741,93.,-83.0216714186056));
#60978=CARTESIAN_POINT('',(29.0442819617723,93.,-92.5477139742631));
#60979=CARTESIAN_POINT('',(26.1581826285113,93.,-73.5302266900378));
#60980=CARTESIAN_POINT('',(18.6578959760632,93.,-100.847779802016));
#60981=CARTESIAN_POINT('',(38.2837343548768,93.,-93.4785672943413));
#60982=CARTESIAN_POINT('',(40.9720007025968,93.,-94.5304976043187));
#60983=CARTESIAN_POINT('',(-0.338657290464837,93.,-78.3654575200769));
#60984=CARTESIAN_POINT('',(41.4051355050055,93.,-97.3845697085718));
#60985=CARTESIAN_POINT('',(37.5232427561124,93.,-71.8054619003202));
#60986=CARTESIAN_POINT('',(39.1500039596942,93.,-99.1867115028475));
#60987=CARTESIAN_POINT('',(25.8341161633122,93.,-109.827828193197));
#60988=CARTESIAN_POINT('',(36.4617376119742,93.,-98.13478119287));
#60989=CARTESIAN_POINT('',(-2.16065403336741,93.,-83.0216714186056));
#60990=CARTESIAN_POINT('',(36.0286028095654,93.,-95.280709088617));
#60991=CARTESIAN_POINT('',(32.5798448630808,93.,-72.5556733846182));
#60992=CARTESIAN_POINT('',(22.7127150131835,93.,-105.921825778966));
#60993=CARTESIAN_POINT('',(45.2680552026699,93.,-96.2115624086952));
#60994=CARTESIAN_POINT('',(47.9563215503899,93.,-97.2634927186726));
#60995=CARTESIAN_POINT('',(-0.338657290464843,93.,-78.3654575200769));
#60996=CARTESIAN_POINT('',(48.3894563527986,93.,-100.117564822926));
#60997=CARTESIAN_POINT('',(43.9449049906818,93.,-70.8309085949005));
#60998=CARTESIAN_POINT('',(46.1343248074873,93.,-101.919706617201));
#60999=CARTESIAN_POINT('',(29.8889352004325,93.,-114.901874170147));
#61000=CARTESIAN_POINT('',(43.4460584597673,93.,-100.867776307224));
#61001=CARTESIAN_POINT('',(-2.16065403336741,93.,-83.0216714186056));
#61002=CARTESIAN_POINT('',(43.0129236573585,93.,-98.0137042029708));
#61003=CARTESIAN_POINT('',(39.0015070976502,93.,-71.5811200791985));
#61004=CARTESIAN_POINT('',(26.7675340503037,93.,-110.995871755917));
#61005=CARTESIAN_POINT('',(-46.6534330450882,93.,-53.2675290825475));
#61006=CARTESIAN_POINT('',(-43.9651666973681,93.,-54.3194593925249));
#61007=CARTESIAN_POINT('',(2.02818590698443,93.,-72.3168582377067));
#61008=CARTESIAN_POINT('',(-43.5320318949594,93.,-57.1735314967781));
#61009=CARTESIAN_POINT('',(-39.5367040587215,93.,-83.5001015653555));
#61010=CARTESIAN_POINT('',(-45.7871634402707,93.,-58.9756732910537));
#61011=CARTESIAN_POINT('',(-26.878531319251,93.,-43.8652304928404));
#61012=CARTESIAN_POINT('',(-48.4754297879908,93.,-57.9237429810763));
#61013=CARTESIAN_POINT('',(0.206189164081799,93.,-76.9730721362355));
#61014=CARTESIAN_POINT('',(-48.9085645903995,93.,-55.0696708768232));
#61015=CARTESIAN_POINT('',(-44.4801019517526,93.,-84.250313049654));
#61016=CARTESIAN_POINT('',(-29.9999324693798,93.,-39.9592280786099));
#61017=CARTESIAN_POINT('',(-44.4027985921934,93.,-68.0977227616416));
#61018=CARTESIAN_POINT('',(-41.7145322444734,93.,-69.1496530716191));
#61019=CARTESIAN_POINT('',(-2.70550048791399,93.,-84.4140568024469));
#61020=CARTESIAN_POINT('',(-41.2813974420647,93.,-72.0037251758721));
#61021=CARTESIAN_POINT('',(-39.5367040587214,93.,-83.5001015653555));
#61022=CARTESIAN_POINT('',(-43.536528987376,93.,-73.8058669701478));
#61023=CARTESIAN_POINT('',(-18.7688932450105,93.,-54.0133224467414));
#61024=CARTESIAN_POINT('',(-46.224795335096,93.,-72.7539366601704));
#61025=CARTESIAN_POINT('',(-4.52749723081664,93.,-89.0702707009757));
#61026=CARTESIAN_POINT('',(-46.6579301375048,93.,-69.8998645559173));
#61027=CARTESIAN_POINT('',(-44.4801019517526,93.,-84.250313049654));
#61028=CARTESIAN_POINT('',(-21.8902943951393,93.,-50.1073200325109));
#61029=CARTESIAN_POINT('',(-37.4184777444003,93.,-70.8307178759955));
#61030=CARTESIAN_POINT('',(-34.7302113966803,93.,-71.8826481859729));
#61031=CARTESIAN_POINT('',(-2.70550048791399,93.,-84.4140568024469));
#61032=CARTESIAN_POINT('',(-34.2970765942716,93.,-74.7367202902261));
#61033=CARTESIAN_POINT('',(-33.1150418241519,93.,-82.5255482599359));
#61034=CARTESIAN_POINT('',(-36.5522081395829,93.,-76.5388620845017));
#61035=CARTESIAN_POINT('',(-14.7140742078902,93.,-59.0873684236919));
#61036=CARTESIAN_POINT('',(-39.2404744873029,93.,-75.4869317745243));
#61037=CARTESIAN_POINT('',(-4.52749723081664,93.,-89.0702707009757));
#61038=CARTESIAN_POINT('',(-39.6736092897116,93.,-72.6328596702712));
#61039=CARTESIAN_POINT('',(-38.0584397171832,93.,-83.2757597442344));
#61040=CARTESIAN_POINT('',(-17.835475358019,93.,-55.1813660094614));
#61041=CARTESIAN_POINT('',(-30.4341568966072,93.,-73.5637129903494));
#61042=CARTESIAN_POINT('',(-27.7458905488871,93.,-74.6156433003268));
#61043=CARTESIAN_POINT('',(-2.705500487914,93.,-84.4140568024469));
#61044=CARTESIAN_POINT('',(-27.3127557464784,93.,-77.4697154045799));
#61045=CARTESIAN_POINT('',(-26.6933795895824,93.,-81.5509949545163));
#61046=CARTESIAN_POINT('',(-29.5678872917897,93.,-79.2718571988556));
#61047=CARTESIAN_POINT('',(-10.65925517077,93.,-64.1614144006423));
#61048=CARTESIAN_POINT('',(-32.2561536395098,93.,-78.2199268888782));
#61049=CARTESIAN_POINT('',(-4.52749723081664,93.,-89.0702707009757));
#61050=CARTESIAN_POINT('',(-32.6892884419185,93.,-75.3658547846251));
#61051=CARTESIAN_POINT('',(-31.6367774826137,93.,-82.3012064388147));
#61052=CARTESIAN_POINT('',(-13.7806563208988,93.,-60.2554119864118));
#61053=CARTESIAN_POINT('',(-23.449836048814,93.,-76.2967081047033));
#61054=CARTESIAN_POINT('',(-20.761569701094,93.,-77.3486384146807));
#61055=CARTESIAN_POINT('',(-2.705500487914,93.,-84.4140568024469));
#61056=CARTESIAN_POINT('',(-20.3284348986853,93.,-80.2027105189338));
#61057=CARTESIAN_POINT('',(-20.2717173550129,93.,-80.5764416490967));
#61058=CARTESIAN_POINT('',(-22.5835664439966,93.,-82.0048523132095));
#61059=CARTESIAN_POINT('',(-6.60443613364973,93.,-69.2354603775928));
#61060=CARTESIAN_POINT('',(-25.2718327917166,93.,-80.9529220032321));
#61061=CARTESIAN_POINT('',(-4.52749723081664,93.,-89.0702707009757));
#61062=CARTESIAN_POINT('',(-25.7049675941254,93.,-78.098849898979));
#61063=CARTESIAN_POINT('',(-25.2151152480443,93.,-81.3266531333951));
#61064=CARTESIAN_POINT('',(-9.72583728377851,93.,-65.3294579633623));
#61065=CARTESIAN_POINT('',(-16.4655152010209,93.,-79.0297032190572));
#61066=CARTESIAN_POINT('',(-13.7772488533009,93.,-80.0816335290346));
#61067=CARTESIAN_POINT('',(-2.70550048791401,93.,-84.4140568024469));
#61068=CARTESIAN_POINT('',(-13.3441140508922,93.,-82.9357056332877));
#61069=CARTESIAN_POINT('',(-13.8500551204434,93.,-79.6018883436771));
#61070=CARTESIAN_POINT('',(-15.5992455962035,93.,-84.7378474275634));
#61071=CARTESIAN_POINT('',(-2.54961709652949,93.,-74.3095063545433));
#61072=CARTESIAN_POINT('',(-18.2875119439235,93.,-83.685917117586));
#61073=CARTESIAN_POINT('',(-4.52749723081664,93.,-89.0702707009757));
#61074=CARTESIAN_POINT('',(-18.7206467463322,93.,-80.8318450133329));
#61075=CARTESIAN_POINT('',(-18.7934530134748,93.,-80.3520998279754));
#61076=CARTESIAN_POINT('',(-5.67101824665826,93.,-70.4035039403128));
#61077=CARTESIAN_POINT('',(-9.48119435322776,93.,-81.7626983334111));
#61078=CARTESIAN_POINT('',(-6.79292800550775,93.,-82.8146286433885));
#61079=CARTESIAN_POINT('',(-2.70550048791401,93.,-84.414056802447));
#61080=CARTESIAN_POINT('',(-6.35979320309903,93.,-85.6687007476416));
#61081=CARTESIAN_POINT('',(-7.42839288587396,93.,-78.6273350382574));
#61082=CARTESIAN_POINT('',(-8.61492474841036,93.,-87.4708425419172));
#61083=CARTESIAN_POINT('',(1.50520194059076,93.,-79.3835523314937));
#61084=CARTESIAN_POINT('',(-11.3031910961304,93.,-86.4189122319399));
#61085=CARTESIAN_POINT('',(-4.52749723081664,93.,-89.0702707009757));
#61086=CARTESIAN_POINT('',(-11.7363258985391,93.,-83.5648401276868));
#61087=CARTESIAN_POINT('',(-12.3717907789053,93.,-79.3775465225557));
#61088=CARTESIAN_POINT('',(-1.61619920953801,93.,-75.4775499172633));
#61089=CARTESIAN_POINT('',(-2.49687350543463,93.,-84.495693447765));
#61090=CARTESIAN_POINT('',(0.191392842285382,93.,-85.5476237577424));
#61091=CARTESIAN_POINT('',(-2.70550048791402,93.,-84.414056802447));
#61092=CARTESIAN_POINT('',(0.6245276446941,93.,-88.4016958619955));
#61093=CARTESIAN_POINT('',(-1.00673065130447,93.,-77.6527817328378));
#61094=CARTESIAN_POINT('',(-1.63060390061722,93.,-90.2038376562712));
#61095=CARTESIAN_POINT('',(5.560020977711,93.,-84.4575983084442));
#61096=CARTESIAN_POINT('',(-4.31887024833725,93.,-89.1519073462937));
#61097=CARTESIAN_POINT('',(-4.52749723081663,93.,-89.0702707009757));
#61098=CARTESIAN_POINT('',(-4.75200505074598,93.,-86.2978352420407));
#61099=CARTESIAN_POINT('',(-5.9501285443359,93.,-78.4029932171361));
#61100=CARTESIAN_POINT('',(2.43861982758224,93.,-80.5515958942137));
#61101=CARTESIAN_POINT('',(4.4874473423585,93.,-87.2286885621189));
#61102=CARTESIAN_POINT('',(7.17571369007852,93.,-88.2806188720963));
#61103=CARTESIAN_POINT('',(-2.70550048791402,93.,-84.414056802447));
#61104=CARTESIAN_POINT('',(7.60884849248723,93.,-91.1346909763494));
#61105=CARTESIAN_POINT('',(5.41493158326502,93.,-76.6782284274182));
#61106=CARTESIAN_POINT('',(5.35371694717591,93.,-92.936832770625));
#61107=CARTESIAN_POINT('',(9.61484001483125,93.,-89.5316442853947));
#61108=CARTESIAN_POINT('',(2.66545059945588,93.,-91.8849024606476));
#61109=CARTESIAN_POINT('',(-4.52749723081663,93.,-89.0702707009757));
#61110=CARTESIAN_POINT('',(2.23231579704715,93.,-89.0308303563946));
#61111=CARTESIAN_POINT('',(0.471533690233556,93.,-77.4284399117164));
#61112=CARTESIAN_POINT('',(6.49343886470249,93.,-85.6256418711642));
#61113=CARTESIAN_POINT('',(39.4090515813242,93.,-100.893664133888));
#61114=CARTESIAN_POINT('',(42.0973179290442,93.,-101.945594443866));
#61115=CARTESIAN_POINT('',(-2.70550048791405,93.,-84.414056802447));
#61116=CARTESIAN_POINT('',(42.5304527314529,93.,-104.799666548119));
#61117=CARTESIAN_POINT('',(37.5232427561124,93.,-71.8054619003202));
#61118=CARTESIAN_POINT('',(40.2753211861416,93.,-106.601808342394));
#61119=CARTESIAN_POINT('',(29.8889352004325,93.,-114.901874170147));
#61120=CARTESIAN_POINT('',(37.5870548384215,93.,-105.549878032417));
#61121=CARTESIAN_POINT('',(-4.52749723081663,93.,-89.0702707009757));
#61122=CARTESIAN_POINT('',(37.1539200360128,93.,-102.695805928164));
#61123=CARTESIAN_POINT('',(32.5798448630808,93.,-72.5556733846182));
#61124=CARTESIAN_POINT('',(26.7675340503037,93.,-110.995871755917));
#61125=CARTESIAN_POINT('',(-45.5281158186408,93.,-60.6826259220946));
#61126=CARTESIAN_POINT('',(-42.8398494709208,93.,-61.734556232072));
#61127=CARTESIAN_POINT('',(-0.338657290464777,93.,-78.3654575200768));
#61128=CARTESIAN_POINT('',(-42.4067146685121,93.,-64.5886283363251));
#61129=CARTESIAN_POINT('',(-39.5367040587214,93.,-83.5001015653555));
#61130=CARTESIAN_POINT('',(-44.6618462138234,93.,-66.3907701306008));
#61131=CARTESIAN_POINT('',(-22.8237122821307,93.,-48.9392764697909));
#61132=CARTESIAN_POINT('',(-47.3501125615434,93.,-65.3388398206233));
#61133=CARTESIAN_POINT('',(-2.16065403336742,93.,-83.0216714186056));
#61134=CARTESIAN_POINT('',(-47.7832473639521,93.,-62.4847677163703));
#61135=CARTESIAN_POINT('',(-44.4801019517526,93.,-84.250313049654));
#61136=CARTESIAN_POINT('',(-25.9451134322595,93.,-45.0332740555604));
#61137=CARTESIAN_POINT('',(-38.5437949708476,93.,-63.4156210364485));
#61138=CARTESIAN_POINT('',(-35.8555286231276,93.,-64.4675513464259));
#61139=CARTESIAN_POINT('',(-0.338657290464782,93.,-78.3654575200768));
#61140=CARTESIAN_POINT('',(-35.4223938207189,93.,-67.321623450679));
#61141=CARTESIAN_POINT('',(-33.1150418241519,93.,-82.5255482599359));
#61142=CARTESIAN_POINT('',(-37.6775253660303,93.,-69.1237652449547));
#61143=CARTESIAN_POINT('',(-18.7688932450105,93.,-54.0133224467414));
#61144=CARTESIAN_POINT('',(-40.3657917137503,93.,-68.0718349349772));
#61145=CARTESIAN_POINT('',(-2.16065403336742,93.,-83.0216714186056));
#61146=CARTESIAN_POINT('',(-40.798926516159,93.,-65.2177628307242));
#61147=CARTESIAN_POINT('',(-38.0584397171832,93.,-83.2757597442344));
#61148=CARTESIAN_POINT('',(-21.8902943951393,93.,-50.1073200325109));
#61149=CARTESIAN_POINT('',(-31.5594741230545,93.,-66.1486161508024));
#61150=CARTESIAN_POINT('',(-28.8712077753345,93.,-67.2005464607798));
#61151=CARTESIAN_POINT('',(-0.338657290464787,93.,-78.3654575200768));
#61152=CARTESIAN_POINT('',(-28.4380729729258,93.,-70.0546185650329));
#61153=CARTESIAN_POINT('',(-26.6933795895825,93.,-81.5509949545163));
#61154=CARTESIAN_POINT('',(-30.6932045182371,93.,-71.8567603593086));
#61155=CARTESIAN_POINT('',(-14.7140742078902,93.,-59.0873684236919));
#61156=CARTESIAN_POINT('',(-33.3814708659571,93.,-70.8048300493311));
#61157=CARTESIAN_POINT('',(-2.16065403336742,93.,-83.0216714186056));
#61158=CARTESIAN_POINT('',(-33.8146056683659,93.,-67.9507579450781));
#61159=CARTESIAN_POINT('',(-31.6367774826137,93.,-82.3012064388147));
#61160=CARTESIAN_POINT('',(-17.835475358019,93.,-55.1813660094614));
#61161=CARTESIAN_POINT('',(32.424730733531,93.,-98.1606690195344));
#61162=CARTESIAN_POINT('',(35.112997081251,93.,-99.2125993295118));
#61163=CARTESIAN_POINT('',(-2.70550048791404,93.,-84.414056802447));
#61164=CARTESIAN_POINT('',(35.5461318836598,93.,-102.066671433765));
#61165=CARTESIAN_POINT('',(31.1015805215429,93.,-72.7800152057398));
#61166=CARTESIAN_POINT('',(33.2910003383484,93.,-103.868813228041));
#61167=CARTESIAN_POINT('',(25.8341161633122,93.,-109.827828193197));
#61168=CARTESIAN_POINT('',(30.6027339906284,93.,-102.816882918063));
#61169=CARTESIAN_POINT('',(-4.52749723081663,93.,-89.0702707009757));
#61170=CARTESIAN_POINT('',(30.1695991882197,93.,-99.9628108138101));
#61171=CARTESIAN_POINT('',(26.1581826285114,93.,-73.5302266900378));
#61172=CARTESIAN_POINT('',(22.7127150131835,93.,-105.921825778966));
#61173=CARTESIAN_POINT('',(25.4404098857379,93.,-95.4276739051805));
#61174=CARTESIAN_POINT('',(28.1286762334579,93.,-96.479604215158));
#61175=CARTESIAN_POINT('',(-2.70550048791404,93.,-84.414056802447));
#61176=CARTESIAN_POINT('',(28.5618110358666,93.,-99.3336763194111));
#61177=CARTESIAN_POINT('',(24.6799182869735,93.,-73.7545685111594));
#61178=CARTESIAN_POINT('',(26.3066794905553,93.,-101.135818113687));
#61179=CARTESIAN_POINT('',(21.779297126192,93.,-104.753782216246));
#61180=CARTESIAN_POINT('',(23.6184131428353,93.,-100.083887803709));
#61181=CARTESIAN_POINT('',(-4.52749723081663,93.,-89.0702707009757));
#61182=CARTESIAN_POINT('',(23.1852783404265,93.,-97.2298156994562));
#61183=CARTESIAN_POINT('',(19.7365203939419,93.,-74.5047799954575));
#61184=CARTESIAN_POINT('',(18.6578959760632,93.,-100.847779802016));
#61185=CARTESIAN_POINT('',(18.4560890379448,93.,-92.6946787908267));
#61186=CARTESIAN_POINT('',(21.1443553856648,93.,-93.7466091008041));
#61187=CARTESIAN_POINT('',(-2.70550048791403,93.,-84.414056802447));
#61188=CARTESIAN_POINT('',(21.5774901880735,93.,-96.6006812050572));
#61189=CARTESIAN_POINT('',(18.258256052404,93.,-74.729121816579));
#61190=CARTESIAN_POINT('',(19.3223586427622,93.,-98.4028229993328));
#61191=CARTESIAN_POINT('',(17.7244780890717,93.,-99.6797362392957));
#61192=CARTESIAN_POINT('',(16.6340922950421,93.,-97.3508926893554));
#61193=CARTESIAN_POINT('',(-4.52749723081663,93.,-89.0702707009757));
#61194=CARTESIAN_POINT('',(16.2009574926334,93.,-94.4968205851023));
#61195=CARTESIAN_POINT('',(13.3148581593725,93.,-75.4793333008771));
#61196=CARTESIAN_POINT('',(14.603076938943,93.,-95.7737338250652));
#61197=CARTESIAN_POINT('',(11.4717681901516,93.,-89.9616836764728));
#61198=CARTESIAN_POINT('',(14.1600345378716,93.,-91.0136139864502));
#61199=CARTESIAN_POINT('',(-2.70550048791403,93.,-84.414056802447));
#61200=CARTESIAN_POINT('',(14.5931693402804,93.,-93.8676860907033));
#61201=CARTESIAN_POINT('',(11.8365938178345,93.,-75.7036751219986));
#61202=CARTESIAN_POINT('',(12.338037794969,93.,-95.6698278849789));
#61203=CARTESIAN_POINT('',(13.6696590519515,93.,-94.6056902623452));
#61204=CARTESIAN_POINT('',(9.64977144724901,93.,-94.6178975750015));
#61205=CARTESIAN_POINT('',(-4.52749723081663,93.,-89.0702707009757));
#61206=CARTESIAN_POINT('',(9.21663664484028,93.,-91.7638254707484));
#61207=CARTESIAN_POINT('',(6.89319592480301,93.,-76.4538866062968));
#61208=CARTESIAN_POINT('',(10.5482579018227,93.,-90.6996878481147));
#61209=CARTESIAN_POINT('',(36.033099901982,93.,-78.6483736152472));
#61210=CARTESIAN_POINT('',(38.721366249702,93.,-79.7003039252246));
#61211=CARTESIAN_POINT('',(4.39502910443358,93.,-66.2682589553367));
#61212=CARTESIAN_POINT('',(39.1545010521108,93.,-82.5543760294777));
#61213=CARTESIAN_POINT('',(37.5232427561122,93.,-71.8054619003202));
#61214=CARTESIAN_POINT('',(36.8993695067994,93.,-84.3565178237533));
#61215=CARTESIAN_POINT('',(17.7244780890717,93.,-99.6797362392957));
#61216=CARTESIAN_POINT('',(34.2111031590794,93.,-83.3045875137759));
#61217=CARTESIAN_POINT('',(2.57303236153103,93.,-70.9244728538654));
#61218=CARTESIAN_POINT('',(33.7779683566707,93.,-80.4505154095229));
#61219=CARTESIAN_POINT('',(32.5798448630807,93.,-72.5556733846182));
#61220=CARTESIAN_POINT('',(14.603076938943,93.,-95.7737338250652));
#61221=CARTESIAN_POINT('',(43.0174207497752,93.,-81.381368729601));
#61222=CARTESIAN_POINT('',(45.7056870974952,93.,-82.4332990395785));
#61223=CARTESIAN_POINT('',(4.39502910443358,93.,-66.2682589553367));
#61224=CARTESIAN_POINT('',(46.1388218999039,93.,-85.2873711438316));
#61225=CARTESIAN_POINT('',(43.9449049906817,93.,-70.8309085949006));
#61226=CARTESIAN_POINT('',(43.8836903545926,93.,-87.0895129381072));
#61227=CARTESIAN_POINT('',(21.779297126192,93.,-104.753782216246));
#61228=CARTESIAN_POINT('',(41.1954240068725,93.,-86.0375826281298));
#61229=CARTESIAN_POINT('',(2.57303236153103,93.,-70.9244728538654));
#61230=CARTESIAN_POINT('',(40.7622892044638,93.,-83.1835105238767));
#61231=CARTESIAN_POINT('',(39.0015070976502,93.,-71.5811200791985));
#61232=CARTESIAN_POINT('',(18.6578959760632,93.,-100.847779802016));
#61233=CARTESIAN_POINT('',(50.0017415975683,93.,-84.1143638439549));
#61234=CARTESIAN_POINT('',(52.6900079452883,93.,-85.1662941539323));
#61235=CARTESIAN_POINT('',(4.39502910443357,93.,-66.2682589553367));
#61236=CARTESIAN_POINT('',(53.123142747697,93.,-88.0203662581854));
#61237=CARTESIAN_POINT('',(50.3665672252512,93.,-69.856355289481));
#61238=CARTESIAN_POINT('',(50.8680112023857,93.,-89.8225080524611));
#61239=CARTESIAN_POINT('',(25.8341161633122,93.,-109.827828193197));
#61240=CARTESIAN_POINT('',(48.1797448546657,93.,-88.7705777424837));
#61241=CARTESIAN_POINT('',(2.57303236153103,93.,-70.9244728538654));
#61242=CARTESIAN_POINT('',(47.7466100522569,93.,-85.9165056382306));
#61243=CARTESIAN_POINT('',(45.4231693322196,93.,-70.6065667737789));
#61244=CARTESIAN_POINT('',(22.7127150131835,93.,-105.921825778966));
#61245=CARTESIAN_POINT('',(-41.9197466501898,93.,-41.1703305178073));
#61246=CARTESIAN_POINT('',(-39.2314803024698,93.,-42.2222608277847));
#61247=CARTESIAN_POINT('',(6.76187230188284,93.,-60.2196596729665));
#61248=CARTESIAN_POINT('',(-38.798345500061,93.,-45.0763329320378));
#61249=CARTESIAN_POINT('',(-33.1150418241522,93.,-82.525548259936));
#61250=CARTESIAN_POINT('',(-41.0534770453724,93.,-46.8784747263135));
#61251=CARTESIAN_POINT('',(-30.9333503563712,93.,-38.7911845158899));
#61252=CARTESIAN_POINT('',(-43.7417433930924,93.,-45.8265444163361));
#61253=CARTESIAN_POINT('',(4.93987555898024,93.,-64.8758735714953));
#61254=CARTESIAN_POINT('',(-44.1748781955011,93.,-42.972472312083));
#61255=CARTESIAN_POINT('',(-38.0584397171832,93.,-83.2757597442344));
#61256=CARTESIAN_POINT('',(-34.0547515065,93.,-34.8851821016595));
#61257=CARTESIAN_POINT('',(29.0487790541889,93.,-75.9153785008933));
#61258=CARTESIAN_POINT('',(31.7370454019089,93.,-76.9673088108707));
#61259=CARTESIAN_POINT('',(4.39502910443359,93.,-66.2682589553367));
#61260=CARTESIAN_POINT('',(32.1701802043176,93.,-79.8213809151238));
#61261=CARTESIAN_POINT('',(31.1015805215427,93.,-72.7800152057398));
#61262=CARTESIAN_POINT('',(29.9150486590063,93.,-81.6235227093995));
#61263=CARTESIAN_POINT('',(13.6696590519515,93.,-94.6056902623452));
#61264=CARTESIAN_POINT('',(27.2267823112863,93.,-80.571592399422));
#61265=CARTESIAN_POINT('',(2.57303236153103,93.,-70.9244728538654));
#61266=CARTESIAN_POINT('',(26.7936475088776,93.,-77.717520295169));
#61267=CARTESIAN_POINT('',(26.1581826285113,93.,-73.5302266900378));
#61268=CARTESIAN_POINT('',(10.5482579018228,93.,-90.6996878481147));
#61269=CARTESIAN_POINT('',(22.0644582063958,93.,-73.1823833865394));
#61270=CARTESIAN_POINT('',(24.7527245541158,93.,-74.2343136965168));
#61271=CARTESIAN_POINT('',(4.39502910443359,93.,-66.2682589553367));
#61272=CARTESIAN_POINT('',(25.1858593565245,93.,-77.0883858007699));
#61273=CARTESIAN_POINT('',(24.6799182869733,93.,-73.7545685111594));
#61274=CARTESIAN_POINT('',(22.9307278112132,93.,-78.8905275950456));
#61275=CARTESIAN_POINT('',(9.61484001483124,93.,-89.5316442853947));
#61276=CARTESIAN_POINT('',(20.2424614634932,93.,-77.8385972850681));
#61277=CARTESIAN_POINT('',(2.57303236153103,93.,-70.9244728538654));
#61278=CARTESIAN_POINT('',(19.8093266610844,93.,-74.9845251808151));
#61279=CARTESIAN_POINT('',(19.7365203939419,93.,-74.5047799954575));
#61280=CARTESIAN_POINT('',(6.4934388647025,93.,-85.6256418711642));
#61281=CARTESIAN_POINT('',(15.0801373586026,93.,-70.4493882721855));
#61282=CARTESIAN_POINT('',(17.7684037063227,93.,-71.5013185821629));
#61283=CARTESIAN_POINT('',(4.3950291044336,93.,-66.2682589553367));
#61284=CARTESIAN_POINT('',(18.2015385087314,93.,-74.355390686416));
#61285=CARTESIAN_POINT('',(18.2582560524038,93.,-74.729121816579));
#61286=CARTESIAN_POINT('',(15.94640696342,93.,-76.1575324806917));
#61287=CARTESIAN_POINT('',(5.560020977711,93.,-84.4575983084442));
#61288=CARTESIAN_POINT('',(13.2581406157,93.,-75.1056021707142));
#61289=CARTESIAN_POINT('',(2.57303236153103,93.,-70.9244728538654));
#61290=CARTESIAN_POINT('',(12.8250058132913,93.,-72.2515300664612));
#61291=CARTESIAN_POINT('',(13.3148581593724,93.,-75.4793333008771));
#61292=CARTESIAN_POINT('',(2.43861982758225,93.,-80.5515958942137));
#61293=CARTESIAN_POINT('',(8.09581651080951,93.,-67.7163931578316));
#61294=CARTESIAN_POINT('',(10.7840828585295,93.,-68.768323467809));
#61295=CARTESIAN_POINT('',(4.3950291044336,93.,-66.2682589553366));
#61296=CARTESIAN_POINT('',(11.2172176609382,93.,-71.6223955720621));
#61297=CARTESIAN_POINT('',(11.8365938178343,93.,-75.7036751219986));
#61298=CARTESIAN_POINT('',(8.96208611562692,93.,-73.4245373663378));
#61299=CARTESIAN_POINT('',(1.50520194059076,93.,-79.3835523314937));
#61300=CARTESIAN_POINT('',(6.27381976790689,93.,-72.3726070563604));
#61301=CARTESIAN_POINT('',(2.57303236153103,93.,-70.9244728538654));
#61302=CARTESIAN_POINT('',(5.84068496549816,93.,-69.5185349521073));
#61303=CARTESIAN_POINT('',(6.89319592480295,93.,-76.4538866062968));
#61304=CARTESIAN_POINT('',(-1.616199209538,93.,-75.4775499172633));
#61305=CARTESIAN_POINT('',(-34.9354258023966,93.,-43.9033256321612));
#61306=CARTESIAN_POINT('',(-32.2471594546766,93.,-44.9552559421386));
#61307=CARTESIAN_POINT('',(6.76187230188284,93.,-60.2196596729665));
#61308=CARTESIAN_POINT('',(-31.8140246522679,93.,-47.8093280463917));
#61309=CARTESIAN_POINT('',(-26.6933795895827,93.,-81.5509949545163));
#61310=CARTESIAN_POINT('',(-34.0691561975792,93.,-49.6114698406674));
#61311=CARTESIAN_POINT('',(-26.878531319251,93.,-43.8652304928404));
#61312=CARTESIAN_POINT('',(-36.7574225452993,93.,-48.55953953069));
#61313=CARTESIAN_POINT('',(4.93987555898024,93.,-64.8758735714953));
#61314=CARTESIAN_POINT('',(-37.190557347708,93.,-45.7054674264369));
#61315=CARTESIAN_POINT('',(-31.6367774826138,93.,-82.3012064388147));
#61316=CARTESIAN_POINT('',(-29.9999324693798,93.,-39.95922807861));
#61317=CARTESIAN_POINT('',(-27.9511049546035,93.,-46.6363207465151));
#61318=CARTESIAN_POINT('',(-25.2628386068835,93.,-47.6882510564925));
#61319=CARTESIAN_POINT('',(6.76187230188283,93.,-60.2196596729665));
#61320=CARTESIAN_POINT('',(-24.8297038044748,93.,-50.5423231607456));
#61321=CARTESIAN_POINT('',(-20.2717173550132,93.,-80.5764416490967));
#61322=CARTESIAN_POINT('',(-27.0848353497861,93.,-52.3444649550213));
#61323=CARTESIAN_POINT('',(-22.8237122821307,93.,-48.9392764697909));
#61324=CARTESIAN_POINT('',(-29.7731016975061,93.,-51.2925346450439));
#61325=CARTESIAN_POINT('',(4.93987555898024,93.,-64.8758735714953));
#61326=CARTESIAN_POINT('',(-30.2062364999149,93.,-48.4384625407908));
#61327=CARTESIAN_POINT('',(-25.2151152480443,93.,-81.3266531333951));
#61328=CARTESIAN_POINT('',(-25.9451134322595,93.,-45.0332740555604));
#61329=CARTESIAN_POINT('',(-20.9667841068104,93.,-49.369315860869));
#61330=CARTESIAN_POINT('',(-18.2785177590904,93.,-50.4212461708464));
#61331=CARTESIAN_POINT('',(6.76187230188283,93.,-60.2196596729665));
#61332=CARTESIAN_POINT('',(-17.8453829566817,93.,-53.2753182750995));
#61333=CARTESIAN_POINT('',(-13.8500551204437,93.,-79.6018883436771));
#61334=CARTESIAN_POINT('',(-20.100514501993,93.,-55.0774600693752));
#61335=CARTESIAN_POINT('',(-18.7688932450105,93.,-54.0133224467414));
#61336=CARTESIAN_POINT('',(-22.788780849713,93.,-54.0255297593977));
#61337=CARTESIAN_POINT('',(4.93987555898024,93.,-64.8758735714953));
#61338=CARTESIAN_POINT('',(-23.2219156521217,93.,-51.1714576551447));
#61339=CARTESIAN_POINT('',(-18.7934530134749,93.,-80.3520998279754));
#61340=CARTESIAN_POINT('',(-21.8902943951393,93.,-50.1073200325109));
#61341=CARTESIAN_POINT('',(-13.9824632590173,93.,-52.1023109752229));
#61342=CARTESIAN_POINT('',(-11.2941969112972,93.,-53.1542412852003));
#61343=CARTESIAN_POINT('',(6.76187230188282,93.,-60.2196596729665));
#61344=CARTESIAN_POINT('',(-10.8610621088885,93.,-56.0083133894534));
#61345=CARTESIAN_POINT('',(-7.42839288587424,93.,-78.6273350382575));
#61346=CARTESIAN_POINT('',(-13.1161936541999,93.,-57.8104551837291));
#61347=CARTESIAN_POINT('',(-14.7140742078902,93.,-59.0873684236919));
#61348=CARTESIAN_POINT('',(-15.8044600019199,93.,-56.7585248737516));
#61349=CARTESIAN_POINT('',(4.93987555898024,93.,-64.8758735714953));
#61350=CARTESIAN_POINT('',(-16.2375948043286,93.,-53.9044527694986));
#61351=CARTESIAN_POINT('',(-12.3717907789054,93.,-79.3775465225558));
#61352=CARTESIAN_POINT('',(-17.835475358019,93.,-55.1813660094614));
#61353=CARTESIAN_POINT('',(-6.99814241122413,93.,-54.8353060895768));
#61354=CARTESIAN_POINT('',(-4.30987606350412,93.,-55.8872363995542));
#61355=CARTESIAN_POINT('',(6.76187230188282,93.,-60.2196596729665));
#61356=CARTESIAN_POINT('',(-3.8767412610954,93.,-58.7413085038073));
#61357=CARTESIAN_POINT('',(-1.00673065130475,93.,-77.6527817328379));
#61358=CARTESIAN_POINT('',(-6.13187280640672,93.,-60.5434502980829));
#61359=CARTESIAN_POINT('',(-10.65925517077,93.,-64.1614144006423));
#61360=CARTESIAN_POINT('',(-8.82013915412675,93.,-59.4915199881055));
#61361=CARTESIAN_POINT('',(4.93987555898024,93.,-64.8758735714953));
#61362=CARTESIAN_POINT('',(-9.25327395653548,93.,-56.6374478838525));
#61363=CARTESIAN_POINT('',(-5.95012854433598,93.,-78.4029932171361));
#61364=CARTESIAN_POINT('',(-13.7806563208988,93.,-60.2554119864119));
#61365=CARTESIAN_POINT('',(-0.0138215634309935,93.,-57.5683012039307));
#61366=CARTESIAN_POINT('',(2.67444478428902,93.,-58.6202315139081));
#61367=CARTESIAN_POINT('',(6.76187230188281,93.,-60.2196596729665));
#61368=CARTESIAN_POINT('',(3.10757958669774,93.,-61.4743036181612));
#61369=CARTESIAN_POINT('',(5.41493158326473,93.,-76.6782284274183));
#61370=CARTESIAN_POINT('',(0.852448041386411,93.,-63.2764454124368));
#61371=CARTESIAN_POINT('',(-6.60443613364974,93.,-69.2354603775928));
#61372=CARTESIAN_POINT('',(-1.83581830633362,93.,-62.2245151024594));
#61373=CARTESIAN_POINT('',(4.93987555898025,93.,-64.8758735714953));
#61374=CARTESIAN_POINT('',(-2.26895310874235,93.,-59.3704429982063));
#61375=CARTESIAN_POINT('',(0.471533690233477,93.,-77.4284399117164));
#61376=CARTESIAN_POINT('',(-9.7258372837785,93.,-65.3294579633623));
#61377=CARTESIAN_POINT('',(6.97049928436214,93.,-60.3012963182845));
#61378=CARTESIAN_POINT('',(9.65876563208215,93.,-61.353226628262));
#61379=CARTESIAN_POINT('',(6.76187230188281,93.,-60.2196596729665));
#61380=CARTESIAN_POINT('',(10.0919004344909,93.,-64.2072987325151));
#61381=CARTESIAN_POINT('',(11.8365938178342,93.,-75.7036751219986));
#61382=CARTESIAN_POINT('',(7.83676888917954,93.,-66.0094405267907));
#61383=CARTESIAN_POINT('',(-2.54961709652949,93.,-74.3095063545433));
#61384=CARTESIAN_POINT('',(5.14850254145952,93.,-64.9575102168133));
#61385=CARTESIAN_POINT('',(4.93987555898025,93.,-64.8758735714953));
#61386=CARTESIAN_POINT('',(4.71536773905078,93.,-62.1034381125602));
#61387=CARTESIAN_POINT('',(6.89319592480293,93.,-76.4538866062968));
#61388=CARTESIAN_POINT('',(-5.67101824665825,93.,-70.4035039403128));
#61389=CARTESIAN_POINT('',(13.9548201321553,93.,-63.0342914326384));
#61390=CARTESIAN_POINT('',(16.6430864798753,93.,-64.0862217426158));
#61391=CARTESIAN_POINT('',(6.7618723018828,93.,-60.2196596729666));
#61392=CARTESIAN_POINT('',(17.076221282284,93.,-66.940293846869));
#61393=CARTESIAN_POINT('',(18.2582560524037,93.,-74.729121816579));
#61394=CARTESIAN_POINT('',(14.8210897369727,93.,-68.7424356411446));
#61395=CARTESIAN_POINT('',(1.50520194059075,93.,-79.3835523314937));
#61396=CARTESIAN_POINT('',(12.1328233892526,93.,-67.6905053311672));
#61397=CARTESIAN_POINT('',(4.93987555898025,93.,-64.8758735714953));
#61398=CARTESIAN_POINT('',(11.6996885868439,93.,-64.8364332269141));
#61399=CARTESIAN_POINT('',(13.3148581593724,93.,-75.4793333008771));
#61400=CARTESIAN_POINT('',(-1.616199209538,93.,-75.4775499172633));
#61401=CARTESIAN_POINT('',(-11.7318288061225,93.,-66.932504654317));
#61402=CARTESIAN_POINT('',(-9.04356245840249,93.,-67.9844349642944));
#61403=CARTESIAN_POINT('',(2.02818590698441,93.,-72.3168582377067));
#61404=CARTESIAN_POINT('',(-8.61042765599378,93.,-70.8385070685475));
#61405=CARTESIAN_POINT('',(-7.42839288587409,93.,-78.6273350382575));
#61406=CARTESIAN_POINT('',(-10.8655592013051,93.,-72.6406488628232));
#61407=CARTESIAN_POINT('',(-6.60443613364973,93.,-69.2354603775928));
#61408=CARTESIAN_POINT('',(-13.5538255490251,93.,-71.5887185528457));
#61409=CARTESIAN_POINT('',(0.206189164081805,93.,-76.9730721362355));
#61410=CARTESIAN_POINT('',(-13.9869603514339,93.,-68.7346464485927));
#61411=CARTESIAN_POINT('',(-12.3717907789054,93.,-79.3775465225557));
#61412=CARTESIAN_POINT('',(-9.72583728377851,93.,-65.3294579633623));
#61413=CARTESIAN_POINT('',(-4.74750795832937,93.,-69.6654997686709));
#61414=CARTESIAN_POINT('',(-2.05924161060936,93.,-70.7174300786483));
#61415=CARTESIAN_POINT('',(2.0281859069844,93.,-72.3168582377067));
#61416=CARTESIAN_POINT('',(-1.62610680820064,93.,-73.5715021829014));
#61417=CARTESIAN_POINT('',(-1.00673065130461,93.,-77.6527817328379));
#61418=CARTESIAN_POINT('',(-3.88123835351197,93.,-75.3736439771771));
#61419=CARTESIAN_POINT('',(-2.54961709652949,93.,-74.3095063545433));
#61420=CARTESIAN_POINT('',(-6.569504701232,93.,-74.3217136671996));
#61421=CARTESIAN_POINT('',(0.206189164081806,93.,-76.9730721362355));
#61422=CARTESIAN_POINT('',(-7.00263950364073,93.,-71.4676415629466));
#61423=CARTESIAN_POINT('',(-5.95012854433593,93.,-78.4029932171361));
#61424=CARTESIAN_POINT('',(-5.67101824665825,93.,-70.4035039403128));
#61425=CARTESIAN_POINT('',(2.23681288946376,93.,-72.3984948830248));
#61426=CARTESIAN_POINT('',(4.92507923718377,93.,-73.4504251930022));
#61427=CARTESIAN_POINT('',(2.0281859069844,93.,-72.3168582377067));
#61428=CARTESIAN_POINT('',(5.35821403959249,93.,-76.3044972972553));
#61429=CARTESIAN_POINT('',(5.41493158326488,93.,-76.6782284274182));
#61430=CARTESIAN_POINT('',(3.10308249428116,93.,-78.1066390915309));
#61431=CARTESIAN_POINT('',(1.50520194059076,93.,-79.3835523314937));
#61432=CARTESIAN_POINT('',(0.414816146561137,93.,-77.0547087815535));
#61433=CARTESIAN_POINT('',(0.206189164081808,93.,-76.9730721362355));
#61434=CARTESIAN_POINT('',(-0.0183186558475948,93.,-74.2006366773005));
#61435=CARTESIAN_POINT('',(0.471533690233522,93.,-77.4284399117164));
#61436=CARTESIAN_POINT('',(-1.616199209538,93.,-75.4775499172633));
#61437=CARTESIAN_POINT('',(9.22113373725689,93.,-75.1314899973787));
#61438=CARTESIAN_POINT('',(11.9094000849769,93.,-76.1834203073561));
#61439=CARTESIAN_POINT('',(2.02818590698439,93.,-72.3168582377068));
#61440=CARTESIAN_POINT('',(12.3425348873856,93.,-79.0374924116092));
#61441=CARTESIAN_POINT('',(11.8365938178344,93.,-75.7036751219986));
#61442=CARTESIAN_POINT('',(10.0874033420743,93.,-80.8396342058848));
#61443=CARTESIAN_POINT('',(5.560020977711,93.,-84.4575983084442));
#61444=CARTESIAN_POINT('',(7.39913699435427,93.,-79.7877038959074));
#61445=CARTESIAN_POINT('',(0.206189164081809,93.,-76.9730721362355));
#61446=CARTESIAN_POINT('',(6.96600219194553,93.,-76.9336317916543));
#61447=CARTESIAN_POINT('',(6.89319592480297,93.,-76.4538866062968));
#61448=CARTESIAN_POINT('',(2.43861982758225,93.,-80.5515958942137));
#61449=CARTESIAN_POINT('',(16.20545458505,93.,-77.8644851117325));
#61450=CARTESIAN_POINT('',(18.89372093277,93.,-78.9164154217099));
#61451=CARTESIAN_POINT('',(2.02818590698439,93.,-72.3168582377068));
#61452=CARTESIAN_POINT('',(19.3268557351787,93.,-81.770487525963));
#61453=CARTESIAN_POINT('',(18.2582560524038,93.,-74.729121816579));
#61454=CARTESIAN_POINT('',(17.0717241898674,93.,-83.5726293202387));
#61455=CARTESIAN_POINT('',(9.61484001483125,93.,-89.5316442853947));
#61456=CARTESIAN_POINT('',(14.3834578421474,93.,-82.5206990102613));
#61457=CARTESIAN_POINT('',(0.20618916408181,93.,-76.9730721362355));
#61458=CARTESIAN_POINT('',(13.9503230397387,93.,-79.6666269060082));
#61459=CARTESIAN_POINT('',(13.3148581593724,93.,-75.4793333008771));
#61460=CARTESIAN_POINT('',(6.4934388647025,93.,-85.6256418711642));
#61461=CARTESIAN_POINT('',(23.1897754328432,93.,-80.5974802260864));
#61462=CARTESIAN_POINT('',(25.8780417805632,93.,-81.6494105360638));
#61463=CARTESIAN_POINT('',(2.02818590698438,93.,-72.3168582377068));
#61464=CARTESIAN_POINT('',(26.3111765829719,93.,-84.5034826403169));
#61465=CARTESIAN_POINT('',(24.6799182869733,93.,-73.7545685111594));
#61466=CARTESIAN_POINT('',(24.0560450376606,93.,-86.3056244345926));
#61467=CARTESIAN_POINT('',(13.6696590519515,93.,-94.6056902623452));
#61468=CARTESIAN_POINT('',(21.3677786899405,93.,-85.2536941246152));
#61469=CARTESIAN_POINT('',(0.206189164081811,93.,-76.9730721362355));
#61470=CARTESIAN_POINT('',(20.9346438875318,93.,-82.3996220203621));
#61471=CARTESIAN_POINT('',(19.7365203939419,93.,-74.5047799954575));
#61472=CARTESIAN_POINT('',(10.5482579018228,93.,-90.6996878481147));
#61473=CARTESIAN_POINT('',(30.1740962806363,93.,-83.3304753404403));
#61474=CARTESIAN_POINT('',(32.8623626283563,93.,-84.3824056504177));
#61475=CARTESIAN_POINT('',(2.02818590698438,93.,-72.3168582377068));
#61476=CARTESIAN_POINT('',(33.295497430765,93.,-87.2364777546708));
#61477=CARTESIAN_POINT('',(31.1015805215428,93.,-72.7800152057398));
#61478=CARTESIAN_POINT('',(31.0403658854537,93.,-89.0386195489465));
#61479=CARTESIAN_POINT('',(17.7244780890717,93.,-99.6797362392957));
#61480=CARTESIAN_POINT('',(28.3520995377337,93.,-87.9866892389691));
#61481=CARTESIAN_POINT('',(0.206189164081812,93.,-76.9730721362355));
#61482=CARTESIAN_POINT('',(27.9189647353249,93.,-85.132617134716));
#61483=CARTESIAN_POINT('',(26.1581826285113,93.,-73.5302266900378));
#61484=CARTESIAN_POINT('',(14.603076938943,93.,-95.7737338250652));
#61485=CARTESIAN_POINT('',(37.1584171284294,93.,-86.0634704547942));
#61486=CARTESIAN_POINT('',(39.8466834761494,93.,-87.1154007647716));
#61487=CARTESIAN_POINT('',(2.02818590698437,93.,-72.3168582377068));
#61488=CARTESIAN_POINT('',(40.2798182785581,93.,-89.9694728690247));
#61489=CARTESIAN_POINT('',(37.5232427561123,93.,-71.8054619003202));
#61490=CARTESIAN_POINT('',(38.0246867332468,93.,-91.7716146633004));
#61491=CARTESIAN_POINT('',(21.779297126192,93.,-104.753782216246));
#61492=CARTESIAN_POINT('',(35.3364203855268,93.,-90.719684353323));
#61493=CARTESIAN_POINT('',(0.206189164081812,93.,-76.9730721362355));
#61494=CARTESIAN_POINT('',(34.903285583118,93.,-87.8656122490699));
#61495=CARTESIAN_POINT('',(32.5798448630808,93.,-72.5556733846182));
#61496=CARTESIAN_POINT('',(18.6578959760632,93.,-100.847779802016));
#61497=CARTESIAN_POINT('',(1.11149566301639,93.,-64.9833980434777));
#61498=CARTESIAN_POINT('',(3.7997620107364,93.,-66.0353283534551));
#61499=CARTESIAN_POINT('',(4.39502910443361,93.,-66.2682589553366));
#61500=CARTESIAN_POINT('',(4.23289681314511,93.,-68.8894004577082));
#61501=CARTESIAN_POINT('',(5.41493158326481,93.,-76.6782284274183));
#61502=CARTESIAN_POINT('',(1.97776526783379,93.,-70.6915422519839));
#61503=CARTESIAN_POINT('',(-2.54961709652949,93.,-74.3095063545433));
#61504=CARTESIAN_POINT('',(-0.710501079886239,93.,-69.6396119420065));
#61505=CARTESIAN_POINT('',(2.57303236153103,93.,-70.9244728538654));
#61506=CARTESIAN_POINT('',(-1.14363588229497,93.,-66.7855398377534));
#61507=CARTESIAN_POINT('',(0.471533690233501,93.,-77.4284399117164));
#61508=CARTESIAN_POINT('',(-5.67101824665825,93.,-70.4035039403128));
#61509=CARTESIAN_POINT('',(-5.87282518477675,93.,-62.2504029291238));
#61510=CARTESIAN_POINT('',(-3.18455883705674,93.,-63.3023332391012));
#61511=CARTESIAN_POINT('',(4.39502910443361,93.,-66.2682589553366));
#61512=CARTESIAN_POINT('',(-2.75142403464802,93.,-66.1564053433543));
#61513=CARTESIAN_POINT('',(-1.00673065130468,93.,-77.6527817328379));
#61514=CARTESIAN_POINT('',(-5.00655557995934,93.,-67.95854713763));
#61515=CARTESIAN_POINT('',(-6.60443613364974,93.,-69.2354603775928));
#61516=CARTESIAN_POINT('',(-7.69482192767937,93.,-66.9066168276526));
#61517=CARTESIAN_POINT('',(2.57303236153103,93.,-70.9244728538654));
#61518=CARTESIAN_POINT('',(-8.1279567300881,93.,-64.0525447233995));
#61519=CARTESIAN_POINT('',(-5.95012854433595,93.,-78.4029932171361));
#61520=CARTESIAN_POINT('',(-9.7258372837785,93.,-65.3294579633623));
#61521=CARTESIAN_POINT('',(-12.8571460325699,93.,-59.5174078147699));
#61522=CARTESIAN_POINT('',(-10.1688796848499,93.,-60.5693381247473));
#61523=CARTESIAN_POINT('',(4.39502910443361,93.,-66.2682589553366));
#61524=CARTESIAN_POINT('',(-9.73574488244115,93.,-63.4234102290004));
#61525=CARTESIAN_POINT('',(-7.42839288587416,93.,-78.6273350382575));
#61526=CARTESIAN_POINT('',(-11.9908764277525,93.,-65.2255520232761));
#61527=CARTESIAN_POINT('',(-10.65925517077,93.,-64.1614144006423));
#61528=CARTESIAN_POINT('',(-14.6791427754725,93.,-64.1736217132987));
#61529=CARTESIAN_POINT('',(2.57303236153102,93.,-70.9244728538654));
#61530=CARTESIAN_POINT('',(-15.1122775778812,93.,-61.3195496090456));
#61531=CARTESIAN_POINT('',(-12.3717907789054,93.,-79.3775465225558));
#61532=CARTESIAN_POINT('',(-13.7806563208988,93.,-60.2554119864119));
#61533=CARTESIAN_POINT('',(-19.841466880363,93.,-56.784412700416));
#61534=CARTESIAN_POINT('',(-17.153200532643,93.,-57.8363430103935));
#61535=CARTESIAN_POINT('',(4.39502910443362,93.,-66.2682589553366));
#61536=CARTESIAN_POINT('',(-16.7200657302343,93.,-60.6904151146466));
#61537=CARTESIAN_POINT('',(-13.8500551204436,93.,-79.6018883436771));
#61538=CARTESIAN_POINT('',(-18.9751972755456,93.,-62.4925569089222));
#61539=CARTESIAN_POINT('',(-14.7140742078902,93.,-59.0873684236919));
#61540=CARTESIAN_POINT('',(-21.6634636232656,93.,-61.4406265989448));
#61541=CARTESIAN_POINT('',(2.57303236153102,93.,-70.9244728538654));
#61542=CARTESIAN_POINT('',(-22.0965984256744,93.,-58.5865544946917));
#61543=CARTESIAN_POINT('',(-18.7934530134749,93.,-80.3520998279754));
#61544=CARTESIAN_POINT('',(-17.835475358019,93.,-55.1813660094614));
#61545=CARTESIAN_POINT('',(44.1427379762225,93.,-88.7964655691481));
#61546=CARTESIAN_POINT('',(46.8310043239425,93.,-89.8483958791255));
#61547=CARTESIAN_POINT('',(2.02818590698437,93.,-72.3168582377068));
#61548=CARTESIAN_POINT('',(47.2641391263513,93.,-92.7024679833786));
#61549=CARTESIAN_POINT('',(43.9449049906818,93.,-70.8309085949006));
#61550=CARTESIAN_POINT('',(45.0090075810399,93.,-94.5046097776543));
#61551=CARTESIAN_POINT('',(25.8341161633122,93.,-109.827828193197));
#61552=CARTESIAN_POINT('',(42.3207412333199,93.,-93.4526794676769));
#61553=CARTESIAN_POINT('',(0.206189164081814,93.,-76.9730721362355));
#61554=CARTESIAN_POINT('',(41.8876064309112,93.,-90.5986073634238));
#61555=CARTESIAN_POINT('',(39.0015070976502,93.,-71.5811200791985));
#61556=CARTESIAN_POINT('',(22.7127150131835,93.,-105.921825778966));
#61557=CARTESIAN_POINT('',(-40.7944294237424,93.,-48.5854273573544));
#61558=CARTESIAN_POINT('',(-38.1061630760224,93.,-49.6373576673318));
#61559=CARTESIAN_POINT('',(4.39502910443363,93.,-66.2682589553366));
#61560=CARTESIAN_POINT('',(-37.6730282736137,93.,-52.4914297715849));
#61561=CARTESIAN_POINT('',(-33.1150418241521,93.,-82.5255482599359));
#61562=CARTESIAN_POINT('',(-39.928159818925,93.,-54.2935715658606));
#61563=CARTESIAN_POINT('',(-26.878531319251,93.,-43.8652304928404));
#61564=CARTESIAN_POINT('',(-42.616426166645,93.,-53.2416412558831));
#61565=CARTESIAN_POINT('',(2.57303236153102,93.,-70.9244728538654));
#61566=CARTESIAN_POINT('',(-43.0495609690538,93.,-50.3875691516301));
#61567=CARTESIAN_POINT('',(-38.0584397171832,93.,-83.2757597442344));
#61568=CARTESIAN_POINT('',(-29.9999324693798,93.,-39.95922807861));
#61569=CARTESIAN_POINT('',(-33.8101085759493,93.,-51.3184224717083));
#61570=CARTESIAN_POINT('',(-31.1218422282293,93.,-52.3703527816857));
#61571=CARTESIAN_POINT('',(4.39502910443363,93.,-66.2682589553366));
#61572=CARTESIAN_POINT('',(-30.6887074258205,93.,-55.2244248859388));
#61573=CARTESIAN_POINT('',(-26.6933795895826,93.,-81.5509949545163));
#61574=CARTESIAN_POINT('',(-32.9438389711319,93.,-57.0265666802144));
#61575=CARTESIAN_POINT('',(-22.8237122821307,93.,-48.9392764697909));
#61576=CARTESIAN_POINT('',(-35.6321053188519,93.,-55.974636370237));
#61577=CARTESIAN_POINT('',(2.57303236153102,93.,-70.9244728538654));
#61578=CARTESIAN_POINT('',(-36.0652401212606,93.,-53.120564265984));
#61579=CARTESIAN_POINT('',(-31.6367774826138,93.,-82.3012064388147));
#61580=CARTESIAN_POINT('',(-25.9451134322595,93.,-45.0332740555604));
#61581=CARTESIAN_POINT('',(-26.8257877281561,93.,-54.0514175860622));
#61582=CARTESIAN_POINT('',(-24.1375213804361,93.,-55.1033478960396));
#61583=CARTESIAN_POINT('',(4.39502910443362,93.,-66.2682589553366));
#61584=CARTESIAN_POINT('',(-23.7043865780274,93.,-57.9574200002927));
#61585=CARTESIAN_POINT('',(-20.2717173550131,93.,-80.5764416490967));
#61586=CARTESIAN_POINT('',(-25.9595181233387,93.,-59.7595617945683));
#61587=CARTESIAN_POINT('',(-18.7688932450105,93.,-54.0133224467414));
#61588=CARTESIAN_POINT('',(-28.6477844710588,93.,-58.7076314845909));
#61589=CARTESIAN_POINT('',(2.57303236153102,93.,-70.9244728538654));
#61590=CARTESIAN_POINT('',(-29.0809192734675,93.,-55.8535593803378));
#61591=CARTESIAN_POINT('',(-25.2151152480443,93.,-81.3266531333951));
#61592=CARTESIAN_POINT('',(-21.8902943951393,93.,-50.1073200325109));
#61593=CARTESIAN_POINT('',(-25.9328879908176,93.,-103.224100348538));
#61594=CARTESIAN_POINT('',(-23.2446216430976,93.,-104.276030658515));
#61595=CARTESIAN_POINT('',(-12.1728732777108,93.,-108.608453931927));
#61596=CARTESIAN_POINT('',(-22.8114868406889,93.,-107.130102762768));
#61597=CARTESIAN_POINT('',(-26.6933795895821,93.,-81.5509949545162));
#61598=CARTESIAN_POINT('',(-25.0666183860002,93.,-108.932244557044));
#61599=CARTESIAN_POINT('',(5.56002097771103,93.,-84.4575983084443));
#61600=CARTESIAN_POINT('',(-27.7548847337203,93.,-107.880314247066));
#61601=CARTESIAN_POINT('',(-13.9948700206135,93.,-113.264667830456));
#61602=CARTESIAN_POINT('',(-28.188019536129,93.,-105.026242142813));
#61603=CARTESIAN_POINT('',(-31.6367774826136,93.,-82.3012064388147));
#61604=CARTESIAN_POINT('',(2.43861982758225,93.,-80.5515958942138));
#61605=CARTESIAN_POINT('',(-18.9485671430245,93.,-105.957095462892));
#61606=CARTESIAN_POINT('',(-16.2603007953045,93.,-107.009025772869));
#61607=CARTESIAN_POINT('',(-12.1728732777108,93.,-108.608453931927));
#61608=CARTESIAN_POINT('',(-15.8271659928958,93.,-109.863097877122));
#61609=CARTESIAN_POINT('',(-20.2717173550126,93.,-80.5764416490966));
#61610=CARTESIAN_POINT('',(-18.0822975382071,93.,-111.665239671398));
#61611=CARTESIAN_POINT('',(9.61484001483127,93.,-89.5316442853947));
#61612=CARTESIAN_POINT('',(-20.7705638859271,93.,-110.61330936142));
#61613=CARTESIAN_POINT('',(-13.9948700206135,93.,-113.264667830456));
#61614=CARTESIAN_POINT('',(-21.2036986883359,93.,-107.759237257167));
#61615=CARTESIAN_POINT('',(-25.2151152480442,93.,-81.326653133395));
#61616=CARTESIAN_POINT('',(6.4934388647025,93.,-85.6256418711642));
#61617=CARTESIAN_POINT('',(-11.9642462952314,93.,-108.690090577245));
#61618=CARTESIAN_POINT('',(-9.27597994751136,93.,-109.742020887223));
#61619=CARTESIAN_POINT('',(-12.1728732777108,93.,-108.608453931927));
#61620=CARTESIAN_POINT('',(-8.84284514510264,93.,-112.596092991476));
#61621=CARTESIAN_POINT('',(-13.8500551204431,93.,-79.601888343677));
#61622=CARTESIAN_POINT('',(-11.097976690414,93.,-114.398234785752));
#61623=CARTESIAN_POINT('',(13.6696590519515,93.,-94.6056902623452));
#61624=CARTESIAN_POINT('',(-13.786243038134,93.,-113.346304475774));
#61625=CARTESIAN_POINT('',(-13.9948700206135,93.,-113.264667830456));
#61626=CARTESIAN_POINT('',(-14.2193778405427,93.,-110.492232371521));
#61627=CARTESIAN_POINT('',(-18.7934530134747,93.,-80.3520998279754));
#61628=CARTESIAN_POINT('',(10.5482579018228,93.,-90.6996878481147));
#61629=CARTESIAN_POINT('',(-4.97992544743824,93.,-111.423085691599));
#61630=CARTESIAN_POINT('',(-2.29165909971822,93.,-112.475016001577));
#61631=CARTESIAN_POINT('',(-12.1728732777108,93.,-108.608453931927));
#61632=CARTESIAN_POINT('',(-1.85852429730951,93.,-115.32908810583));
#61633=CARTESIAN_POINT('',(-7.42839288587365,93.,-78.6273350382574));
#61634=CARTESIAN_POINT('',(-4.11365584262083,93.,-117.131229900105));
#61635=CARTESIAN_POINT('',(17.7244780890718,93.,-99.6797362392957));
#61636=CARTESIAN_POINT('',(-6.80192219034086,93.,-116.079299590128));
#61637=CARTESIAN_POINT('',(-13.9948700206135,93.,-113.264667830456));
#61638=CARTESIAN_POINT('',(-7.23505699274959,93.,-113.225227485875));
#61639=CARTESIAN_POINT('',(-12.3717907789052,93.,-79.3775465225557));
#61640=CARTESIAN_POINT('',(14.603076938943,93.,-95.7737338250652));
#61641=CARTESIAN_POINT('',(2.0043954003549,93.,-114.156080805953));
#61642=CARTESIAN_POINT('',(4.69266174807491,93.,-115.208011115931));
#61643=CARTESIAN_POINT('',(-12.1728732777109,93.,-108.608453931927));
#61644=CARTESIAN_POINT('',(5.12579655048363,93.,-118.062083220184));
#61645=CARTESIAN_POINT('',(-1.00673065130416,93.,-77.6527817328378));
#61646=CARTESIAN_POINT('',(2.8706650051723,93.,-119.864225014459));
#61647=CARTESIAN_POINT('',(21.779297126192,93.,-104.753782216246));
#61648=CARTESIAN_POINT('',(0.182398657452273,93.,-118.812294704482));
#61649=CARTESIAN_POINT('',(-13.9948700206135,93.,-113.264667830456));
#61650=CARTESIAN_POINT('',(-0.250736144956458,93.,-115.958222600229));
#61651=CARTESIAN_POINT('',(-5.95012854433579,93.,-78.4029932171361));
#61652=CARTESIAN_POINT('',(18.6578959760633,93.,-100.847779802016));
#61653=CARTESIAN_POINT('',(8.98871624814803,93.,-116.889075920307));
#61654=CARTESIAN_POINT('',(11.676982595868,93.,-117.941006230285));
#61655=CARTESIAN_POINT('',(-12.1728732777109,93.,-108.608453931927));
#61656=CARTESIAN_POINT('',(12.1101173982768,93.,-120.795078334538));
#61657=CARTESIAN_POINT('',(5.41493158326532,93.,-76.6782284274182));
#61658=CARTESIAN_POINT('',(9.85498585296543,93.,-122.597220128813));
#61659=CARTESIAN_POINT('',(25.8341161633123,93.,-109.827828193197));
#61660=CARTESIAN_POINT('',(7.1667195052454,93.,-121.545289818836));
#61661=CARTESIAN_POINT('',(-13.9948700206135,93.,-113.264667830456));
#61662=CARTESIAN_POINT('',(6.73358470283667,93.,-118.691217714583));
#61663=CARTESIAN_POINT('',(0.471533690233657,93.,-77.4284399117164));
#61664=CARTESIAN_POINT('',(22.7127150131835,93.,-105.921825778966));
#61665=CARTESIAN_POINT('',(15.9730370959412,93.,-119.622071034661));
#61666=CARTESIAN_POINT('',(18.6613034436612,93.,-120.674001344638));
#61667=CARTESIAN_POINT('',(-12.1728732777109,93.,-108.608453931927));
#61668=CARTESIAN_POINT('',(19.0944382460699,93.,-123.528073448892));
#61669=CARTESIAN_POINT('',(11.8365938178348,93.,-75.7036751219986));
#61670=CARTESIAN_POINT('',(16.8393067007586,93.,-125.330215243167));
#61671=CARTESIAN_POINT('',(29.8889352004325,93.,-114.901874170147));
#61672=CARTESIAN_POINT('',(14.1510403530385,93.,-124.27828493319));
#61673=CARTESIAN_POINT('',(-13.9948700206135,93.,-113.264667830456));
#61674=CARTESIAN_POINT('',(13.7179055506298,93.,-121.424212828937));
#61675=CARTESIAN_POINT('',(6.89319592480311,93.,-76.4538866062968));
#61676=CARTESIAN_POINT('',(26.7675340503038,93.,-110.995871755917));
#61677=CARTESIAN_POINT('',(22.9573579437343,93.,-122.355066149015));
#61678=CARTESIAN_POINT('',(25.6456242914543,93.,-123.406996458992));
#61679=CARTESIAN_POINT('',(-12.1728732777109,93.,-108.608453931927));
#61680=CARTESIAN_POINT('',(26.078759093863,93.,-126.261068563245));
#61681=CARTESIAN_POINT('',(18.2582560524043,93.,-74.729121816579));
#61682=CARTESIAN_POINT('',(23.8236275485517,93.,-128.063210357521));
#61683=CARTESIAN_POINT('',(33.9437542375528,93.,-119.975920147098));
#61684=CARTESIAN_POINT('',(21.1353612008317,93.,-127.011280047544));
#61685=CARTESIAN_POINT('',(-13.9948700206135,93.,-113.264667830456));
#61686=CARTESIAN_POINT('',(20.7022263984229,93.,-124.157207943291));
#61687=CARTESIAN_POINT('',(13.3148581593726,93.,-75.4793333008771));
#61688=CARTESIAN_POINT('',(30.822353087424,93.,-116.069917732867));
#61689=CARTESIAN_POINT('',(-48.0111677606444,93.,-87.6100181659289));
#61690=CARTESIAN_POINT('',(-45.3229014129244,93.,-88.6619484759063));
#61691=CARTESIAN_POINT('',(-9.80603008026161,93.,-102.559854649557));
#61692=CARTESIAN_POINT('',(-44.8897666105157,93.,-91.5160205801594));
#61693=CARTESIAN_POINT('',(-45.9583662932906,93.,-84.4746548707751));
#61694=CARTESIAN_POINT('',(-47.144898155827,93.,-93.3181623744351));
#61695=CARTESIAN_POINT('',(-10.65925517077,93.,-64.1614144006424));
#61696=CARTESIAN_POINT('',(-49.833164503547,93.,-92.2662320644577));
#61697=CARTESIAN_POINT('',(-11.6280268231643,93.,-107.216068548086));
#61698=CARTESIAN_POINT('',(-50.2662993059558,93.,-89.4121599602046));
#61699=CARTESIAN_POINT('',(-50.901764186322,93.,-85.2248663550737));
#61700=CARTESIAN_POINT('',(-13.7806563208988,93.,-60.2554119864119));
#61701=CARTESIAN_POINT('',(-41.0268469128513,93.,-90.3430132802828));
#61702=CARTESIAN_POINT('',(-38.3385805651313,93.,-91.3949435902602));
#61703=CARTESIAN_POINT('',(-9.80603008026162,93.,-102.559854649557));
#61704=CARTESIAN_POINT('',(-37.9054457627226,93.,-94.2490156945133));
#61705=CARTESIAN_POINT('',(-39.5367040587211,93.,-83.5001015653555));
#61706=CARTESIAN_POINT('',(-40.1605773080339,93.,-96.051157488789));
#61707=CARTESIAN_POINT('',(-6.60443613364971,93.,-69.2354603775928));
#61708=CARTESIAN_POINT('',(-42.8488436557539,93.,-94.9992271788116));
#61709=CARTESIAN_POINT('',(-11.6280268231643,93.,-107.216068548086));
#61710=CARTESIAN_POINT('',(-43.2819784581626,93.,-92.1451550745585));
#61711=CARTESIAN_POINT('',(-44.4801019517525,93.,-84.250313049654));
#61712=CARTESIAN_POINT('',(-9.7258372837785,93.,-65.3294579633623));
#61713=CARTESIAN_POINT('',(-34.0425260650581,93.,-93.0760083946367));
#61714=CARTESIAN_POINT('',(-31.3542597173381,93.,-94.1279387046141));
#61715=CARTESIAN_POINT('',(-9.80603008026162,93.,-102.559854649557));
#61716=CARTESIAN_POINT('',(-30.9211249149294,93.,-96.9820108088672));
#61717=CARTESIAN_POINT('',(-33.1150418241517,93.,-82.5255482599359));
#61718=CARTESIAN_POINT('',(-33.1762564602408,93.,-98.7841526031429));
#61719=CARTESIAN_POINT('',(-2.54961709652947,93.,-74.3095063545433));
#61720=CARTESIAN_POINT('',(-35.8645228079608,93.,-97.7322222931655));
#61721=CARTESIAN_POINT('',(-11.6280268231643,93.,-107.216068548086));
#61722=CARTESIAN_POINT('',(-36.2976576103695,93.,-94.8781501889124));
#61723=CARTESIAN_POINT('',(-38.0584397171831,93.,-83.2757597442344));
#61724=CARTESIAN_POINT('',(-5.67101824665825,93.,-70.4035039403128));
#61725=CARTESIAN_POINT('',(-27.058205217265,93.,-95.8090035089906));
#61726=CARTESIAN_POINT('',(-24.369938869545,93.,-96.860933818968));
#61727=CARTESIAN_POINT('',(-9.80603008026163,93.,-102.559854649557));
#61728=CARTESIAN_POINT('',(-23.9368040671363,93.,-99.7150059232211));
#61729=CARTESIAN_POINT('',(-26.6933795895822,93.,-81.5509949545163));
#61730=CARTESIAN_POINT('',(-26.1919356124476,93.,-101.517147717497));
#61731=CARTESIAN_POINT('',(1.50520194059078,93.,-79.3835523314938));
#61732=CARTESIAN_POINT('',(-28.8802019601676,93.,-100.465217407519));
#61733=CARTESIAN_POINT('',(-11.6280268231643,93.,-107.216068548086));
#61734=CARTESIAN_POINT('',(-29.3133367625764,93.,-97.6111453032663));
#61735=CARTESIAN_POINT('',(-31.6367774826136,93.,-82.3012064388147));
#61736=CARTESIAN_POINT('',(-1.616199209538,93.,-75.4775499172633));
#61737=CARTESIAN_POINT('',(-20.0738843694719,93.,-98.5419986233445));
#61738=CARTESIAN_POINT('',(-17.3856180217519,93.,-99.5939289333219));
#61739=CARTESIAN_POINT('',(-9.80603008026163,93.,-102.559854649557));
#61740=CARTESIAN_POINT('',(-16.9524832193432,93.,-102.448001037575));
#61741=CARTESIAN_POINT('',(-20.2717173550127,93.,-80.5764416490967));
#61742=CARTESIAN_POINT('',(-19.2076147646545,93.,-104.250142831851));
#61743=CARTESIAN_POINT('',(5.56002097771102,93.,-84.4575983084442));
#61744=CARTESIAN_POINT('',(-21.8958811123745,93.,-103.198212521873));
#61745=CARTESIAN_POINT('',(-11.6280268231643,93.,-107.216068548086));
#61746=CARTESIAN_POINT('',(-22.3290159147832,93.,-100.34414041762));
#61747=CARTESIAN_POINT('',(-25.2151152480442,93.,-81.326653133395));
#61748=CARTESIAN_POINT('',(2.43861982758225,93.,-80.5515958942137));
#61749=CARTESIAN_POINT('',(-13.0895635216788,93.,-101.274993737698));
#61750=CARTESIAN_POINT('',(-10.4012971739587,93.,-102.326924047676));
#61751=CARTESIAN_POINT('',(-9.80603008026164,93.,-102.559854649557));
#61752=CARTESIAN_POINT('',(-9.96816237155003,93.,-105.180996151929));
#61753=CARTESIAN_POINT('',(-13.8500551204432,93.,-79.601888343677));
#61754=CARTESIAN_POINT('',(-12.2232939168614,93.,-106.983137946205));
#61755=CARTESIAN_POINT('',(9.61484001483127,93.,-89.5316442853947));
#61756=CARTESIAN_POINT('',(-14.9115602645814,93.,-105.931207636227));
#61757=CARTESIAN_POINT('',(-11.6280268231643,93.,-107.216068548086));
#61758=CARTESIAN_POINT('',(-15.3446950669901,93.,-103.077135531974));
#61759=CARTESIAN_POINT('',(-18.7934530134747,93.,-80.3520998279754));
#61760=CARTESIAN_POINT('',(6.4934388647025,93.,-85.6256418711642));
#61761=CARTESIAN_POINT('',(-6.10524267388563,93.,-104.007988852052));
#61762=CARTESIAN_POINT('',(-3.41697632616561,93.,-105.05991916203));
#61763=CARTESIAN_POINT('',(-9.80603008026164,93.,-102.559854649557));
#61764=CARTESIAN_POINT('',(-2.9838415237569,93.,-107.913991266283));
#61765=CARTESIAN_POINT('',(-7.42839288587373,93.,-78.6273350382574));
#61766=CARTESIAN_POINT('',(-5.23897306906822,93.,-109.716133060558));
#61767=CARTESIAN_POINT('',(13.6696590519515,93.,-94.6056902623452));
#61768=CARTESIAN_POINT('',(-7.92723941678825,93.,-108.664202750581));
#61769=CARTESIAN_POINT('',(-11.6280268231643,93.,-107.216068548086));
#61770=CARTESIAN_POINT('',(-8.36037421919698,93.,-105.810130646328));
#61771=CARTESIAN_POINT('',(-12.3717907789053,93.,-79.3775465225557));
#61772=CARTESIAN_POINT('',(10.5482579018228,93.,-90.6996878481147));
#61773=CARTESIAN_POINT('',(0.879078173907508,93.,-106.740983966406));
#61774=CARTESIAN_POINT('',(3.56734452162752,93.,-107.792914276384));
#61775=CARTESIAN_POINT('',(-9.80603008026165,93.,-102.559854649557));
#61776=CARTESIAN_POINT('',(4.00047932403624,93.,-110.646986380637));
#61777=CARTESIAN_POINT('',(-1.00673065130425,93.,-77.6527817328378));
#61778=CARTESIAN_POINT('',(1.74534777872491,93.,-112.449128174912));
#61779=CARTESIAN_POINT('',(17.7244780890718,93.,-99.6797362392957));
#61780=CARTESIAN_POINT('',(-0.942918568995116,93.,-111.397197864935));
#61781=CARTESIAN_POINT('',(-11.6280268231643,93.,-107.216068548086));
#61782=CARTESIAN_POINT('',(-1.37605337140385,93.,-108.543125760682));
#61783=CARTESIAN_POINT('',(-5.95012854433583,93.,-78.4029932171361));
#61784=CARTESIAN_POINT('',(14.603076938943,93.,-95.7737338250652));
#61785=CARTESIAN_POINT('',(-23.6822535379229,93.,-118.054294027632));
#61786=CARTESIAN_POINT('',(-20.9939871902029,93.,-119.106224337609));
#61787=CARTESIAN_POINT('',(-16.9065596726093,93.,-120.705652496668));
#61788=CARTESIAN_POINT('',(-20.5608523877941,93.,-121.960296441862));
#61789=CARTESIAN_POINT('',(-26.693379589582,93.,-81.5509949545162));
#61790=CARTESIAN_POINT('',(-22.8159839331055,93.,-123.762438236138));
#61791=CARTESIAN_POINT('',(13.6696590519515,93.,-94.6056902623452));
#61792=CARTESIAN_POINT('',(-25.5042502808255,93.,-122.710507926161));
#61793=CARTESIAN_POINT('',(-18.728556415512,93.,-125.361866395196));
#61794=CARTESIAN_POINT('',(-25.9373850832342,93.,-119.856435821907));
#61795=CARTESIAN_POINT('',(-31.6367774826136,93.,-82.3012064388147));
#61796=CARTESIAN_POINT('',(10.5482579018228,93.,-90.6996878481147));
#61797=CARTESIAN_POINT('',(-16.6979326901297,93.,-120.787289141986));
#61798=CARTESIAN_POINT('',(-14.0096663424097,93.,-121.839219451963));
#61799=CARTESIAN_POINT('',(-16.9065596726093,93.,-120.705652496668));
#61800=CARTESIAN_POINT('',(-13.576531540001,93.,-124.693291556216));
#61801=CARTESIAN_POINT('',(-20.2717173550125,93.,-80.5764416490966));
#61802=CARTESIAN_POINT('',(-15.8316630853124,93.,-126.495433350492));
#61803=CARTESIAN_POINT('',(17.7244780890718,93.,-99.6797362392957));
#61804=CARTESIAN_POINT('',(-18.5199294330324,93.,-125.443503040514));
#61805=CARTESIAN_POINT('',(-18.728556415512,93.,-125.361866395196));
#61806=CARTESIAN_POINT('',(-18.9530642354411,93.,-122.589430936261));
#61807=CARTESIAN_POINT('',(-25.2151152480441,93.,-81.326653133395));
#61808=CARTESIAN_POINT('',(14.603076938943,93.,-95.7737338250652));
#61809=CARTESIAN_POINT('',(-9.71361184233662,93.,-123.52028425634));
#61810=CARTESIAN_POINT('',(-7.02534549461661,93.,-124.572214566317));
#61811=CARTESIAN_POINT('',(-16.9065596726093,93.,-120.705652496668));
#61812=CARTESIAN_POINT('',(-6.59221069220789,93.,-127.42628667057));
#61813=CARTESIAN_POINT('',(-13.850055120443,93.,-79.601888343677));
#61814=CARTESIAN_POINT('',(-8.84734223751921,93.,-129.228428464846));
#61815=CARTESIAN_POINT('',(21.779297126192,93.,-104.753782216246));
#61816=CARTESIAN_POINT('',(-11.5356085852392,93.,-128.176498154868));
#61817=CARTESIAN_POINT('',(-18.728556415512,93.,-125.361866395196));
#61818=CARTESIAN_POINT('',(-11.968743387648,93.,-125.322426050615));
#61819=CARTESIAN_POINT('',(-18.7934530134747,93.,-80.3520998279754));
#61820=CARTESIAN_POINT('',(18.6578959760633,93.,-100.847779802016));
#61821=CARTESIAN_POINT('',(-2.72929099454348,93.,-126.253279370693));
#61822=CARTESIAN_POINT('',(-0.0410246468234739,93.,-127.305209680671));
#61823=CARTESIAN_POINT('',(-16.9065596726093,93.,-120.705652496668));
#61824=CARTESIAN_POINT('',(0.392110155585244,93.,-130.159281784924));
#61825=CARTESIAN_POINT('',(-7.42839288587351,93.,-78.6273350382574));
#61826=CARTESIAN_POINT('',(-1.86302138972608,93.,-131.9614235792));
#61827=CARTESIAN_POINT('',(25.8341161633123,93.,-109.827828193197));
#61828=CARTESIAN_POINT('',(-4.55128773744611,93.,-130.909493269222));
#61829=CARTESIAN_POINT('',(-18.728556415512,93.,-125.361866395196));
#61830=CARTESIAN_POINT('',(-4.98442253985484,93.,-128.055421164969));
#61831=CARTESIAN_POINT('',(-12.3717907789052,93.,-79.3775465225557));
#61832=CARTESIAN_POINT('',(22.7127150131835,93.,-105.921825778966));
#61833=CARTESIAN_POINT('',(-45.7605333077496,93.,-102.440211845023));
#61834=CARTESIAN_POINT('',(-43.0722669600296,93.,-103.492142155));
#61835=CARTESIAN_POINT('',(-14.53971647516,93.,-114.657053214297));
#61836=CARTESIAN_POINT('',(-42.6391321576209,93.,-106.346214259254));
#61837=CARTESIAN_POINT('',(-45.9583662932905,93.,-84.4746548707751));
#61838=CARTESIAN_POINT('',(-44.8942637029322,93.,-108.148356053529));
#61839=CARTESIAN_POINT('',(-2.54961709652946,93.,-74.3095063545433));
#61840=CARTESIAN_POINT('',(-47.5825300506523,93.,-107.096425743552));
#61841=CARTESIAN_POINT('',(-16.3617132180627,93.,-119.313267112826));
#61842=CARTESIAN_POINT('',(-48.015664853061,93.,-104.242353639299));
#61843=CARTESIAN_POINT('',(-50.9017641863219,93.,-85.2248663550736));
#61844=CARTESIAN_POINT('',(-5.67101824665825,93.,-70.4035039403128));
#61845=CARTESIAN_POINT('',(-38.7762124599565,93.,-105.173206959377));
#61846=CARTESIAN_POINT('',(-36.0879461122365,93.,-106.225137269354));
#61847=CARTESIAN_POINT('',(-14.53971647516,93.,-114.657053214297));
#61848=CARTESIAN_POINT('',(-35.6548113098278,93.,-109.079209373607));
#61849=CARTESIAN_POINT('',(-39.536704058721,93.,-83.5001015653555));
#61850=CARTESIAN_POINT('',(-37.9099428551391,93.,-110.881351167883));
#61851=CARTESIAN_POINT('',(1.50520194059079,93.,-79.3835523314938));
#61852=CARTESIAN_POINT('',(-40.5982092028591,93.,-109.829420857906));
#61853=CARTESIAN_POINT('',(-16.3617132180627,93.,-119.313267112826));
#61854=CARTESIAN_POINT('',(-41.0313440052679,93.,-106.975348753653));
#61855=CARTESIAN_POINT('',(-44.4801019517525,93.,-84.250313049654));
#61856=CARTESIAN_POINT('',(-1.616199209538,93.,-75.4775499172633));
#61857=CARTESIAN_POINT('',(-31.7918916121634,93.,-107.906202073731));
#61858=CARTESIAN_POINT('',(-29.1036252644434,93.,-108.958132383708));
#61859=CARTESIAN_POINT('',(-14.53971647516,93.,-114.657053214297));
#61860=CARTESIAN_POINT('',(-28.6704904620347,93.,-111.812204487961));
#61861=CARTESIAN_POINT('',(-33.1150418241515,93.,-82.5255482599358));
#61862=CARTESIAN_POINT('',(-30.925622007346,93.,-113.614346282237));
#61863=CARTESIAN_POINT('',(5.56002097771103,93.,-84.4575983084443));
#61864=CARTESIAN_POINT('',(-33.613888355066,93.,-112.56241597226));
#61865=CARTESIAN_POINT('',(-16.3617132180627,93.,-119.313267112826));
#61866=CARTESIAN_POINT('',(-34.0470231574747,93.,-109.708343868006));
#61867=CARTESIAN_POINT('',(-38.058439717183,93.,-83.2757597442344));
#61868=CARTESIAN_POINT('',(2.43861982758225,93.,-80.5515958942138));
#61869=CARTESIAN_POINT('',(-24.8075707643703,93.,-110.639197188085));
#61870=CARTESIAN_POINT('',(-22.1193044166502,93.,-111.691127498062));
#61871=CARTESIAN_POINT('',(-14.53971647516,93.,-114.657053214297));
#61872=CARTESIAN_POINT('',(-21.6861696142415,93.,-114.545199602315));
#61873=CARTESIAN_POINT('',(-26.693379589582,93.,-81.5509949545162));
#61874=CARTESIAN_POINT('',(-23.9413011595529,93.,-116.347341396591));
#61875=CARTESIAN_POINT('',(9.61484001483128,93.,-89.5316442853947));
#61876=CARTESIAN_POINT('',(-26.6295675072729,93.,-115.295411086613));
#61877=CARTESIAN_POINT('',(-16.3617132180627,93.,-119.313267112826));
#61878=CARTESIAN_POINT('',(-27.0627023096816,93.,-112.44133898236));
#61879=CARTESIAN_POINT('',(-31.6367774826136,93.,-82.3012064388147));
#61880=CARTESIAN_POINT('',(6.4934388647025,93.,-85.6256418711642));
#61881=CARTESIAN_POINT('',(10.1140334745954,93.,-124.304172759854));
#61882=CARTESIAN_POINT('',(12.8022998223154,93.,-125.356103069832));
#61883=CARTESIAN_POINT('',(-14.5397164751601,93.,-114.657053214298));
#61884=CARTESIAN_POINT('',(13.2354346247241,93.,-128.210175174085));
#61885=CARTESIAN_POINT('',(5.41493158326539,93.,-76.6782284274182));
#61886=CARTESIAN_POINT('',(10.9803030794128,93.,-130.01231696836));
#61887=CARTESIAN_POINT('',(29.8889352004325,93.,-114.901874170147));
#61888=CARTESIAN_POINT('',(8.29203673169278,93.,-128.960386658383));
#61889=CARTESIAN_POINT('',(-16.3617132180627,93.,-119.313267112826));
#61890=CARTESIAN_POINT('',(7.85890192928405,93.,-126.10631455413));
#61891=CARTESIAN_POINT('',(0.47153369023368,93.,-77.4284399117164));
#61892=CARTESIAN_POINT('',(26.7675340503038,93.,-110.995871755917));
#61893=CARTESIAN_POINT('',(-46.885850534197,93.,-95.025115005476));
#61894=CARTESIAN_POINT('',(-44.197584186477,93.,-96.0770453154534));
#61895=CARTESIAN_POINT('',(-12.1728732777108,93.,-108.608453931927));
#61896=CARTESIAN_POINT('',(-43.7644493840683,93.,-98.9311174197065));
#61897=CARTESIAN_POINT('',(-45.9583662932906,93.,-84.4746548707751));
#61898=CARTESIAN_POINT('',(-46.0195809293796,93.,-100.733259213982));
#61899=CARTESIAN_POINT('',(-6.6044361336497,93.,-69.2354603775928));
#61900=CARTESIAN_POINT('',(-48.7078472770996,93.,-99.6813289040047));
#61901=CARTESIAN_POINT('',(-13.9948700206135,93.,-113.264667830456));
#61902=CARTESIAN_POINT('',(-49.1409820795084,93.,-96.8272567997517));
#61903=CARTESIAN_POINT('',(-50.901764186322,93.,-85.2248663550736));
#61904=CARTESIAN_POINT('',(-9.7258372837785,93.,-65.3294579633623));
#61905=CARTESIAN_POINT('',(-39.9015296864039,93.,-97.7581101198299));
#61906=CARTESIAN_POINT('',(-37.2132633386839,93.,-98.8100404298073));
#61907=CARTESIAN_POINT('',(-12.1728732777108,93.,-108.608453931927));
#61908=CARTESIAN_POINT('',(-36.7801285362752,93.,-101.66411253406));
#61909=CARTESIAN_POINT('',(-39.5367040587211,93.,-83.5001015653555));
#61910=CARTESIAN_POINT('',(-39.0352600815865,93.,-103.466254328336));
#61911=CARTESIAN_POINT('',(-2.54961709652946,93.,-74.3095063545433));
#61912=CARTESIAN_POINT('',(-41.7235264293065,93.,-102.414324018359));
#61913=CARTESIAN_POINT('',(-13.9948700206135,93.,-113.264667830456));
#61914=CARTESIAN_POINT('',(-42.1566612317152,93.,-99.5602519141056));
#61915=CARTESIAN_POINT('',(-44.4801019517525,93.,-84.250313049654));
#61916=CARTESIAN_POINT('',(-5.67101824665825,93.,-70.4035039403128));
#61917=CARTESIAN_POINT('',(-32.9172088386108,93.,-100.491105234184));
#61918=CARTESIAN_POINT('',(-30.2289424908907,93.,-101.543035544161));
#61919=CARTESIAN_POINT('',(-12.1728732777108,93.,-108.608453931927));
#61920=CARTESIAN_POINT('',(-29.795807688482,93.,-104.397107648414));
#61921=CARTESIAN_POINT('',(-33.1150418241516,93.,-82.5255482599359));
#61922=CARTESIAN_POINT('',(-32.0509392337934,93.,-106.19924944269));
#61923=CARTESIAN_POINT('',(1.50520194059079,93.,-79.3835523314938));
#61924=CARTESIAN_POINT('',(-34.7392055815134,93.,-105.147319132713));
#61925=CARTESIAN_POINT('',(-13.9948700206135,93.,-113.264667830456));
#61926=CARTESIAN_POINT('',(-35.1723403839221,93.,-102.293247028459));
#61927=CARTESIAN_POINT('',(-38.058439717183,93.,-83.2757597442344));
#61928=CARTESIAN_POINT('',(-1.616199209538,93.,-75.4775499172633));
#61929=CARTESIAN_POINT('',(3.12971262680227,93.,-121.5711776455));
#61930=CARTESIAN_POINT('',(5.81797897452228,93.,-122.623107955478));
#61931=CARTESIAN_POINT('',(-14.5397164751601,93.,-114.657053214297));
#61932=CARTESIAN_POINT('',(6.251113776931,93.,-125.477180059731));
#61933=CARTESIAN_POINT('',(-1.00673065130409,93.,-77.6527817328378));
#61934=CARTESIAN_POINT('',(3.99598223161968,93.,-127.279321854006));
#61935=CARTESIAN_POINT('',(25.8341161633122,93.,-109.827828193197));
#61936=CARTESIAN_POINT('',(1.30771588389965,93.,-126.227391544029));
#61937=CARTESIAN_POINT('',(-16.3617132180627,93.,-119.313267112826));
#61938=CARTESIAN_POINT('',(0.874581081490917,93.,-123.373319439776));
#61939=CARTESIAN_POINT('',(-5.95012854433577,93.,-78.4029932171361));
#61940=CARTESIAN_POINT('',(22.7127150131835,93.,-105.921825778966));
#61941=CARTESIAN_POINT('',(-3.85460822099086,93.,-118.838182531146));
#61942=CARTESIAN_POINT('',(-1.16634187327085,93.,-119.890112841124));
#61943=CARTESIAN_POINT('',(-14.5397164751601,93.,-114.657053214298));
#61944=CARTESIAN_POINT('',(-0.733207070862132,93.,-122.744184945377));
#61945=CARTESIAN_POINT('',(-7.42839288587358,93.,-78.6273350382574));
#61946=CARTESIAN_POINT('',(-2.98833861617346,93.,-124.546326739653));
#61947=CARTESIAN_POINT('',(21.779297126192,93.,-104.753782216246));
#61948=CARTESIAN_POINT('',(-5.67660496389348,93.,-123.494396429675));
#61949=CARTESIAN_POINT('',(-16.3617132180627,93.,-119.313267112826));
#61950=CARTESIAN_POINT('',(-6.10973976630222,93.,-120.640324325422));
#61951=CARTESIAN_POINT('',(-12.3717907789052,93.,-79.3775465225557));
#61952=CARTESIAN_POINT('',(18.6578959760633,93.,-100.847779802016));
#61953=CARTESIAN_POINT('',(-10.838929068784,93.,-116.105187416792));
#61954=CARTESIAN_POINT('',(-8.15066272106398,93.,-117.15711772677));
#61955=CARTESIAN_POINT('',(-14.5397164751601,93.,-114.657053214297));
#61956=CARTESIAN_POINT('',(-7.71752791865526,93.,-120.011189831023));
#61957=CARTESIAN_POINT('',(-13.8500551204431,93.,-79.601888343677));
#61958=CARTESIAN_POINT('',(-9.97265946396659,93.,-121.813331625299));
#61959=CARTESIAN_POINT('',(17.7244780890718,93.,-99.6797362392957));
#61960=CARTESIAN_POINT('',(-12.6609258116866,93.,-120.761401315321));
#61961=CARTESIAN_POINT('',(-16.3617132180627,93.,-119.313267112826));
#61962=CARTESIAN_POINT('',(-13.0940606140953,93.,-117.907329211068));
#61963=CARTESIAN_POINT('',(-18.7934530134747,93.,-80.3520998279754));
#61964=CARTESIAN_POINT('',(14.603076938943,93.,-95.7737338250652));
#61965=CARTESIAN_POINT('',(-17.8232499165771,93.,-113.372192302439));
#61966=CARTESIAN_POINT('',(-15.1349835688571,93.,-114.424122612416));
#61967=CARTESIAN_POINT('',(-14.53971647516,93.,-114.657053214297));
#61968=CARTESIAN_POINT('',(-14.7018487664484,93.,-117.278194716669));
#61969=CARTESIAN_POINT('',(-20.2717173550125,93.,-80.5764416490966));
#61970=CARTESIAN_POINT('',(-16.9569803117597,93.,-119.080336510945));
#61971=CARTESIAN_POINT('',(13.6696590519515,93.,-94.6056902623452));
#61972=CARTESIAN_POINT('',(-19.6452466594797,93.,-118.028406200967));
#61973=CARTESIAN_POINT('',(-16.3617132180627,93.,-119.313267112826));
#61974=CARTESIAN_POINT('',(-20.0783814618885,93.,-115.174334096714));
#61975=CARTESIAN_POINT('',(-25.2151152480441,93.,-81.326653133395));
#61976=CARTESIAN_POINT('',(10.5482579018228,93.,-90.6996878481147));
#61977=CARTESIAN_POINT('',(-8.35587712678037,93.,-89.1777951729581));
#61978=CARTESIAN_POINT('',(-5.66761077906036,93.,-90.2297254829355));
#61979=CARTESIAN_POINT('',(-5.07234368536322,93.,-90.462656084817));
#61980=CARTESIAN_POINT('',(-5.23447597665164,93.,-93.0837975871887));
#61981=CARTESIAN_POINT('',(-7.42839288587387,93.,-78.6273350382574));
#61982=CARTESIAN_POINT('',(-7.48960752196297,93.,-94.8859393814643));
#61983=CARTESIAN_POINT('',(5.56002097771101,93.,-84.4575983084442));
#61984=CARTESIAN_POINT('',(-10.177873869683,93.,-93.8340090714869));
#61985=CARTESIAN_POINT('',(-6.89434042826585,93.,-95.1188699833458));
#61986=CARTESIAN_POINT('',(-10.6110086720917,93.,-90.9799369672338));
#61987=CARTESIAN_POINT('',(-12.3717907789053,93.,-79.3775465225557));
#61988=CARTESIAN_POINT('',(2.43861982758225,93.,-80.5515958942137));
#61989=CARTESIAN_POINT('',(-15.3401979745735,93.,-86.4448000586042));
#61990=CARTESIAN_POINT('',(-12.6519316268535,93.,-87.4967303685817));
#61991=CARTESIAN_POINT('',(-5.07234368536321,93.,-90.462656084817));
#61992=CARTESIAN_POINT('',(-12.2187968244448,93.,-90.3508024728348));
#61993=CARTESIAN_POINT('',(-13.8500551204434,93.,-79.6018883436771));
#61994=CARTESIAN_POINT('',(-14.4739283697561,93.,-92.1529442671104));
#61995=CARTESIAN_POINT('',(1.50520194059077,93.,-79.3835523314938));
#61996=CARTESIAN_POINT('',(-17.1621947174761,93.,-91.101013957133));
#61997=CARTESIAN_POINT('',(-6.89434042826585,93.,-95.1188699833458));
#61998=CARTESIAN_POINT('',(-17.5953295198849,93.,-88.2469418528799));
#61999=CARTESIAN_POINT('',(-18.7934530134748,93.,-80.3520998279754));
#62000=CARTESIAN_POINT('',(-1.616199209538,93.,-75.4775499172633));
#62001=CARTESIAN_POINT('',(-22.3245188223666,93.,-83.7118049442504));
#62002=CARTESIAN_POINT('',(-19.6362524746466,93.,-84.7637352542278));
#62003=CARTESIAN_POINT('',(-5.07234368536321,93.,-90.462656084817));
#62004=CARTESIAN_POINT('',(-19.2031176722379,93.,-87.6178073584809));
#62005=CARTESIAN_POINT('',(-20.2717173550128,93.,-80.5764416490967));
#62006=CARTESIAN_POINT('',(-21.4582492175492,93.,-89.4199491527566));
#62007=CARTESIAN_POINT('',(-2.54961709652948,93.,-74.3095063545433));
#62008=CARTESIAN_POINT('',(-24.1465155652693,93.,-88.3680188427791));
#62009=CARTESIAN_POINT('',(-6.89434042826585,93.,-95.1188699833458));
#62010=CARTESIAN_POINT('',(-24.579650367678,93.,-85.5139467385261));
#62011=CARTESIAN_POINT('',(-25.2151152480442,93.,-81.326653133395));
#62012=CARTESIAN_POINT('',(-5.67101824665826,93.,-70.4035039403128));
#62013=CARTESIAN_POINT('',(-29.3088396701598,93.,-80.9788098298965));
#62014=CARTESIAN_POINT('',(-26.6205733224398,93.,-82.0307401398739));
#62015=CARTESIAN_POINT('',(-5.0723436853632,93.,-90.462656084817));
#62016=CARTESIAN_POINT('',(-26.187438520031,93.,-84.884812244127));
#62017=CARTESIAN_POINT('',(-26.6933795895823,93.,-81.5509949545163));
#62018=CARTESIAN_POINT('',(-28.4425700653424,93.,-86.6869540384027));
#62019=CARTESIAN_POINT('',(-6.60443613364972,93.,-69.2354603775928));
#62020=CARTESIAN_POINT('',(-31.1308364130624,93.,-85.6350237284252));
#62021=CARTESIAN_POINT('',(-6.89434042826586,93.,-95.1188699833458));
#62022=CARTESIAN_POINT('',(-31.5639712154711,93.,-82.7809516241722));
#62023=CARTESIAN_POINT('',(-31.6367774826137,93.,-82.3012064388147));
#62024=CARTESIAN_POINT('',(-9.72583728377851,93.,-65.3294579633623));
#62025=CARTESIAN_POINT('',(34.6753651864258,93.,-112.990862698629));
#62026=CARTESIAN_POINT('',(37.3636315341458,93.,-114.042793008606));
#62027=CARTESIAN_POINT('',(-7.43918688281246,93.,-96.5112553671872));
#62028=CARTESIAN_POINT('',(37.7967663365545,93.,-116.896865112859));
#62029=CARTESIAN_POINT('',(31.1015805215431,93.,-72.7800152057397));
#62030=CARTESIAN_POINT('',(35.5416347912432,93.,-118.699006907135));
#62031=CARTESIAN_POINT('',(33.9437542375527,93.,-119.975920147098));
#62032=CARTESIAN_POINT('',(32.8533684435232,93.,-117.647076597157));
#62033=CARTESIAN_POINT('',(-9.26118362571507,93.,-101.167469265716));
#62034=CARTESIAN_POINT('',(32.4202336411144,93.,-114.793004492904));
#62035=CARTESIAN_POINT('',(26.1581826285114,93.,-73.5302266900378));
#62036=CARTESIAN_POINT('',(30.822353087424,93.,-116.069917732867));
#62037=CARTESIAN_POINT('',(-50.2618022135392,93.,-72.7798244868348));
#62038=CARTESIAN_POINT('',(-47.5735358658191,93.,-73.8317547968122));
#62039=CARTESIAN_POINT('',(-5.07234368536319,93.,-90.462656084817));
#62040=CARTESIAN_POINT('',(-47.1404010634104,93.,-76.6858269010653));
#62041=CARTESIAN_POINT('',(-45.9583662932908,93.,-84.4746548707751));
#62042=CARTESIAN_POINT('',(-49.3955326087217,93.,-78.487968695341));
#62043=CARTESIAN_POINT('',(-18.7688932450105,93.,-54.0133224467414));
#62044=CARTESIAN_POINT('',(-52.0837989564418,93.,-77.4360383853636));
#62045=CARTESIAN_POINT('',(-6.89434042826586,93.,-95.1188699833458));
#62046=CARTESIAN_POINT('',(-52.5169337588505,93.,-74.5819662811105));
#62047=CARTESIAN_POINT('',(-50.901764186322,93.,-85.2248663550737));
#62048=CARTESIAN_POINT('',(-21.8902943951393,93.,-50.1073200325109));
#62049=CARTESIAN_POINT('',(-43.277481365746,93.,-75.5128196011887));
#62050=CARTESIAN_POINT('',(-40.589215018026,93.,-76.5647499111661));
#62051=CARTESIAN_POINT('',(-5.07234368536319,93.,-90.462656084817));
#62052=CARTESIAN_POINT('',(-40.1560802156173,93.,-79.4188220154192));
#62053=CARTESIAN_POINT('',(-39.5367040587213,93.,-83.5001015653555));
#62054=CARTESIAN_POINT('',(-42.4112117609286,93.,-81.2209638096949));
#62055=CARTESIAN_POINT('',(-14.7140742078902,93.,-59.0873684236919));
#62056=CARTESIAN_POINT('',(-45.0994781086486,93.,-80.1690334997174));
#62057=CARTESIAN_POINT('',(-6.89434042826586,93.,-95.1188699833458));
#62058=CARTESIAN_POINT('',(-45.5326129110574,93.,-77.3149613954644));
#62059=CARTESIAN_POINT('',(-44.4801019517526,93.,-84.250313049654));
#62060=CARTESIAN_POINT('',(-17.835475358019,93.,-55.1813660094614));
#62061=CARTESIAN_POINT('',(-36.2931605179529,93.,-78.2458147155426));
#62062=CARTESIAN_POINT('',(-33.6048941702329,93.,-79.29774502552));
#62063=CARTESIAN_POINT('',(-5.0723436853632,93.,-90.462656084817));
#62064=CARTESIAN_POINT('',(-33.1717593678242,93.,-82.1518171297731));
#62065=CARTESIAN_POINT('',(-33.1150418241518,93.,-82.5255482599359));
#62066=CARTESIAN_POINT('',(-35.4268909131355,93.,-83.9539589240488));
#62067=CARTESIAN_POINT('',(-10.65925517077,93.,-64.1614144006423));
#62068=CARTESIAN_POINT('',(-38.1151572608555,93.,-82.9020286140714));
#62069=CARTESIAN_POINT('',(-6.89434042826586,93.,-95.1188699833458));
#62070=CARTESIAN_POINT('',(-38.5482920632642,93.,-80.0479565098183));
#62071=CARTESIAN_POINT('',(-38.0584397171831,93.,-83.2757597442344));
#62072=CARTESIAN_POINT('',(-13.7806563208988,93.,-60.2554119864119));
#62073=CARTESIAN_POINT('',(26.5657271121853,93.,-102.842770744728));
#62074=CARTESIAN_POINT('',(29.2539934599053,93.,-103.894701054705));
#62075=CARTESIAN_POINT('',(-5.07234368536324,93.,-90.4626560848171));
#62076=CARTESIAN_POINT('',(29.687128262314,93.,-106.748773158958));
#62077=CARTESIAN_POINT('',(24.6799182869735,93.,-73.7545685111594));
#62078=CARTESIAN_POINT('',(27.4319967170027,93.,-108.550914953234));
#62079=CARTESIAN_POINT('',(25.8341161633122,93.,-109.827828193197));
#62080=CARTESIAN_POINT('',(24.7437303692827,93.,-107.498984643256));
#62081=CARTESIAN_POINT('',(-6.89434042826585,93.,-95.1188699833458));
#62082=CARTESIAN_POINT('',(24.3105955668739,93.,-104.644912539003));
#62083=CARTESIAN_POINT('',(19.7365203939419,93.,-74.5047799954575));
#62084=CARTESIAN_POINT('',(22.7127150131835,93.,-105.921825778966));
#62085=CARTESIAN_POINT('',(33.5500479599784,93.,-105.575765859081));
#62086=CARTESIAN_POINT('',(36.2383143076984,93.,-106.627696169059));
#62087=CARTESIAN_POINT('',(-5.07234368536325,93.,-90.4626560848171));
#62088=CARTESIAN_POINT('',(36.6714491101071,93.,-109.481768273312));
#62089=CARTESIAN_POINT('',(31.101580521543,93.,-72.7800152057397));
#62090=CARTESIAN_POINT('',(34.4163175647958,93.,-111.283910067588));
#62091=CARTESIAN_POINT('',(29.8889352004325,93.,-114.901874170147));
#62092=CARTESIAN_POINT('',(31.7280512170758,93.,-110.23197975761));
#62093=CARTESIAN_POINT('',(-6.89434042826585,93.,-95.1188699833458));
#62094=CARTESIAN_POINT('',(31.2949164146671,93.,-107.377907653357));
#62095=CARTESIAN_POINT('',(26.1581826285114,93.,-73.5302266900378));
#62096=CARTESIAN_POINT('',(26.7675340503038,93.,-110.995871755917));
#62097=CARTESIAN_POINT('',(40.5343688077715,93.,-108.308760973435));
#62098=CARTESIAN_POINT('',(43.2226351554916,93.,-109.360691283413));
#62099=CARTESIAN_POINT('',(-5.07234368536325,93.,-90.4626560848171));
#62100=CARTESIAN_POINT('',(43.6557699579003,93.,-112.214763387666));
#62101=CARTESIAN_POINT('',(37.5232427561125,93.,-71.8054619003202));
#62102=CARTESIAN_POINT('',(41.4006384125889,93.,-114.016905181942));
#62103=CARTESIAN_POINT('',(33.9437542375527,93.,-119.975920147098));
#62104=CARTESIAN_POINT('',(38.7123720648689,93.,-112.964974871964));
#62105=CARTESIAN_POINT('',(-6.89434042826584,93.,-95.1188699833458));
#62106=CARTESIAN_POINT('',(38.2792372624602,93.,-110.110902767711));
#62107=CARTESIAN_POINT('',(32.5798448630808,93.,-72.5556733846182));
#62108=CARTESIAN_POINT('',(30.822353087424,93.,-116.069917732867));
#62109=CARTESIAN_POINT('',(-51.3871194399865,93.,-65.3647276472878));
#62110=CARTESIAN_POINT('',(-48.6988530922665,93.,-66.4166579572652));
#62111=CARTESIAN_POINT('',(-2.70550048791398,93.,-84.4140568024469));
#62112=CARTESIAN_POINT('',(-48.2657182898578,93.,-69.2707300615183));
#62113=CARTESIAN_POINT('',(-45.9583662932909,93.,-84.4746548707751));
#62114=CARTESIAN_POINT('',(-50.5208498351691,93.,-71.0728718557939));
#62115=CARTESIAN_POINT('',(-22.8237122821307,93.,-48.9392764697909));
#62116=CARTESIAN_POINT('',(-53.2091161828892,93.,-70.0209415458165));
#62117=CARTESIAN_POINT('',(-4.52749723081664,93.,-89.0702707009757));
#62118=CARTESIAN_POINT('',(-53.6422509852979,93.,-67.1668694415634));
#62119=CARTESIAN_POINT('',(-50.901764186322,93.,-85.2248663550737));
#62120=CARTESIAN_POINT('',(-25.9451134322595,93.,-45.0332740555604));
#62121=CARTESIAN_POINT('',(19.5814062643922,93.,-100.109775630374));
#62122=CARTESIAN_POINT('',(22.2696726121122,93.,-101.161705940351));
#62123=CARTESIAN_POINT('',(-5.07234368536324,93.,-90.4626560848171));
#62124=CARTESIAN_POINT('',(22.7028074145209,93.,-104.015778044604));
#62125=CARTESIAN_POINT('',(18.2582560524041,93.,-74.729121816579));
#62126=CARTESIAN_POINT('',(20.4476758692096,93.,-105.81791983888));
#62127=CARTESIAN_POINT('',(21.779297126192,93.,-104.753782216246));
#62128=CARTESIAN_POINT('',(17.7594095214895,93.,-104.765989528902));
#62129=CARTESIAN_POINT('',(-6.89434042826585,93.,-95.1188699833458));
#62130=CARTESIAN_POINT('',(17.3262747190808,93.,-101.911917424649));
#62131=CARTESIAN_POINT('',(13.3148581593725,93.,-75.4793333008771));
#62132=CARTESIAN_POINT('',(18.6578959760632,93.,-100.847779802016));
#62133=CARTESIAN_POINT('',(12.597085416599,93.,-97.3767805160198));
#62134=CARTESIAN_POINT('',(15.285351764319,93.,-98.4287108259972));
#62135=CARTESIAN_POINT('',(-5.07234368536323,93.,-90.4626560848171));
#62136=CARTESIAN_POINT('',(15.7184865667278,93.,-101.28278293025));
#62137=CARTESIAN_POINT('',(11.8365938178346,93.,-75.7036751219986));
#62138=CARTESIAN_POINT('',(13.4633550214164,93.,-103.084924724526));
#62139=CARTESIAN_POINT('',(17.7244780890717,93.,-99.6797362392957));
#62140=CARTESIAN_POINT('',(10.7750886736964,93.,-102.032994414549));
#62141=CARTESIAN_POINT('',(-6.89434042826585,93.,-95.1188699833458));
#62142=CARTESIAN_POINT('',(10.3419538712877,93.,-99.1789223102955));
#62143=CARTESIAN_POINT('',(6.89319592480304,93.,-76.4538866062968));
#62144=CARTESIAN_POINT('',(14.603076938943,93.,-95.7737338250652));
#62145=CARTESIAN_POINT('',(5.6127645688059,93.,-94.6437854016659));
#62146=CARTESIAN_POINT('',(8.3010309165259,93.,-95.6957157116433));
#62147=CARTESIAN_POINT('',(-5.07234368536323,93.,-90.4626560848171));
#62148=CARTESIAN_POINT('',(8.73416571893462,93.,-98.5497878158964));
#62149=CARTESIAN_POINT('',(5.4149315832651,93.,-76.6782284274182));
#62150=CARTESIAN_POINT('',(6.4790341736233,93.,-100.351929610172));
#62151=CARTESIAN_POINT('',(13.6696590519515,93.,-94.6056902623452));
#62152=CARTESIAN_POINT('',(3.79076782590327,93.,-99.2999993001947));
#62153=CARTESIAN_POINT('',(-6.89434042826585,93.,-95.1188699833458));
#62154=CARTESIAN_POINT('',(3.35763302349454,93.,-96.4459271959416));
#62155=CARTESIAN_POINT('',(0.471533690233591,93.,-77.4284399117164));
#62156=CARTESIAN_POINT('',(10.5482579018228,93.,-90.6996878481147));
#62157=CARTESIAN_POINT('',(-1.37155627898724,93.,-91.910790287312));
#62158=CARTESIAN_POINT('',(1.31671006873277,93.,-92.9627205972894));
#62159=CARTESIAN_POINT('',(-5.07234368536322,93.,-90.4626560848171));
#62160=CARTESIAN_POINT('',(1.74984487114149,93.,-95.8167927015425));
#62161=CARTESIAN_POINT('',(-1.00673065130438,93.,-77.6527817328378));
#62162=CARTESIAN_POINT('',(-0.505286674169835,93.,-97.6189344958182));
#62163=CARTESIAN_POINT('',(9.61484001483126,93.,-89.5316442853947));
#62164=CARTESIAN_POINT('',(-3.19355302188986,93.,-96.5670041858408));
#62165=CARTESIAN_POINT('',(-6.89434042826585,93.,-95.1188699833458));
#62166=CARTESIAN_POINT('',(-3.6266878242986,93.,-93.7129320815877));
#62167=CARTESIAN_POINT('',(-5.95012854433586,93.,-78.4029932171361));
#62168=CARTESIAN_POINT('',(6.4934388647025,93.,-85.6256418711642));
#62169=CARTESIAN_POINT('',(7.86339902170064,93.,-109.47397908076));
#62170=CARTESIAN_POINT('',(10.5516653694206,93.,-110.525909390737));
#62171=CARTESIAN_POINT('',(-9.80603008026165,93.,-102.559854649557));
#62172=CARTESIAN_POINT('',(10.9848001718294,93.,-113.379981494991));
#62173=CARTESIAN_POINT('',(5.41493158326524,93.,-76.6782284274182));
#62174=CARTESIAN_POINT('',(8.72966862651804,93.,-115.182123289266));
#62175=CARTESIAN_POINT('',(21.779297126192,93.,-104.753782216246));
#62176=CARTESIAN_POINT('',(6.04140227879801,93.,-114.130192979289));
#62177=CARTESIAN_POINT('',(-11.6280268231643,93.,-107.216068548086));
#62178=CARTESIAN_POINT('',(5.60826747638928,93.,-111.276120875036));
#62179=CARTESIAN_POINT('',(0.471533690233623,93.,-77.4284399117164));
#62180=CARTESIAN_POINT('',(18.6578959760633,93.,-100.847779802016));
#62181=CARTESIAN_POINT('',(14.8477198694938,93.,-112.206974195114));
#62182=CARTESIAN_POINT('',(17.5359862172138,93.,-113.258904505091));
#62183=CARTESIAN_POINT('',(-9.80603008026165,93.,-102.559854649557));
#62184=CARTESIAN_POINT('',(17.9691210196225,93.,-116.112976609344));
#62185=CARTESIAN_POINT('',(11.8365938178347,93.,-75.7036751219986));
#62186=CARTESIAN_POINT('',(15.7139894743112,93.,-117.91511840362));
#62187=CARTESIAN_POINT('',(25.8341161633122,93.,-109.827828193197));
#62188=CARTESIAN_POINT('',(13.0257231265911,93.,-116.863188093643));
#62189=CARTESIAN_POINT('',(-11.6280268231643,93.,-107.216068548086));
#62190=CARTESIAN_POINT('',(12.5925883241824,93.,-114.00911598939));
#62191=CARTESIAN_POINT('',(6.89319592480307,93.,-76.4538866062968));
#62192=CARTESIAN_POINT('',(22.7127150131835,93.,-105.921825778966));
#62193=CARTESIAN_POINT('',(21.8320407172869,93.,-114.939969309468));
#62194=CARTESIAN_POINT('',(24.5203070650069,93.,-115.991899619445));
#62195=CARTESIAN_POINT('',(-9.80603008026166,93.,-102.559854649557));
#62196=CARTESIAN_POINT('',(24.9534418674156,93.,-118.845971723698));
#62197=CARTESIAN_POINT('',(18.2582560524042,93.,-74.729121816579));
#62198=CARTESIAN_POINT('',(22.6983103221043,93.,-120.648113517974));
#62199=CARTESIAN_POINT('',(29.8889352004325,93.,-114.901874170147));
#62200=CARTESIAN_POINT('',(20.0100439743843,93.,-119.596183207997));
#62201=CARTESIAN_POINT('',(-11.6280268231643,93.,-107.216068548086));
#62202=CARTESIAN_POINT('',(19.5769091719755,93.,-116.742111103744));
#62203=CARTESIAN_POINT('',(13.3148581593725,93.,-75.4793333008771));
#62204=CARTESIAN_POINT('',(26.7675340503038,93.,-110.995871755917));
#62205=CARTESIAN_POINT('',(28.81636156508,93.,-117.672964423822));
#62206=CARTESIAN_POINT('',(31.5046279128,93.,-118.724894733799));
#62207=CARTESIAN_POINT('',(-9.80603008026167,93.,-102.559854649557));
#62208=CARTESIAN_POINT('',(31.9377627152088,93.,-121.578966838052));
#62209=CARTESIAN_POINT('',(24.6799182869737,93.,-73.7545685111593));
#62210=CARTESIAN_POINT('',(29.6826311698974,93.,-123.381108632328));
#62211=CARTESIAN_POINT('',(33.9437542375527,93.,-119.975920147098));
#62212=CARTESIAN_POINT('',(26.9943648221774,93.,-122.32917832235));
#62213=CARTESIAN_POINT('',(-11.6280268231643,93.,-107.216068548086));
#62214=CARTESIAN_POINT('',(26.5612300197687,93.,-119.475106218097));
#62215=CARTESIAN_POINT('',(19.736520393942,93.,-74.5047799954575));
#62216=CARTESIAN_POINT('',(30.822353087424,93.,-116.069917732867));
#62217=CARTESIAN_POINT('',(-49.1364849870918,93.,-80.1949213263819));
#62218=CARTESIAN_POINT('',(-46.4482186393718,93.,-81.2468516363593));
#62219=CARTESIAN_POINT('',(-7.4391868828124,93.,-96.5112553671871));
#62220=CARTESIAN_POINT('',(-46.0150838369631,93.,-84.1009237406124));
#62221=CARTESIAN_POINT('',(-45.9583662932907,93.,-84.4746548707751));
#62222=CARTESIAN_POINT('',(-48.2702153822744,93.,-85.9030655348881));
#62223=CARTESIAN_POINT('',(-14.7140742078902,93.,-59.0873684236919));
#62224=CARTESIAN_POINT('',(-50.9584817299944,93.,-84.8511352249106));
#62225=CARTESIAN_POINT('',(-9.26118362571508,93.,-101.167469265716));
#62226=CARTESIAN_POINT('',(-51.3916165324031,93.,-81.9970631206576));
#62227=CARTESIAN_POINT('',(-50.901764186322,93.,-85.2248663550737));
#62228=CARTESIAN_POINT('',(-17.835475358019,93.,-55.1813660094614));
#62229=CARTESIAN_POINT('',(-42.1521641392987,93.,-82.9279164407358));
#62230=CARTESIAN_POINT('',(-39.4638977915786,93.,-83.9798467507132));
#62231=CARTESIAN_POINT('',(-7.43918688281241,93.,-96.5112553671871));
#62232=CARTESIAN_POINT('',(-39.0307629891699,93.,-86.8339188549663));
#62233=CARTESIAN_POINT('',(-39.5367040587212,93.,-83.5001015653555));
#62234=CARTESIAN_POINT('',(-41.2858945344813,93.,-88.636060649242));
#62235=CARTESIAN_POINT('',(-10.65925517077,93.,-64.1614144006424));
#62236=CARTESIAN_POINT('',(-43.9741608822013,93.,-87.5841303392645));
#62237=CARTESIAN_POINT('',(-9.26118362571508,93.,-101.167469265716));
#62238=CARTESIAN_POINT('',(-44.40729568461,93.,-84.7300582350115));
#62239=CARTESIAN_POINT('',(-44.4801019517526,93.,-84.250313049654));
#62240=CARTESIAN_POINT('',(-13.7806563208988,93.,-60.2554119864119));
#62241=CARTESIAN_POINT('',(-35.1678432915055,93.,-85.6609115550896));
#62242=CARTESIAN_POINT('',(-32.4795769437855,93.,-86.7128418650671));
#62243=CARTESIAN_POINT('',(-7.43918688281241,93.,-96.5112553671871));
#62244=CARTESIAN_POINT('',(-32.0464421413768,93.,-89.5669139693202));
#62245=CARTESIAN_POINT('',(-33.1150418241517,93.,-82.5255482599359));
#62246=CARTESIAN_POINT('',(-34.3015736866881,93.,-91.3690557635958));
#62247=CARTESIAN_POINT('',(-6.60443613364972,93.,-69.2354603775928));
#62248=CARTESIAN_POINT('',(-36.9898400344081,93.,-90.3171254536184));
#62249=CARTESIAN_POINT('',(-9.26118362571508,93.,-101.167469265716));
#62250=CARTESIAN_POINT('',(-37.4229748368169,93.,-87.4630533493654));
#62251=CARTESIAN_POINT('',(-38.0584397171831,93.,-83.2757597442344));
#62252=CARTESIAN_POINT('',(-9.7258372837785,93.,-65.3294579633623));
#62253=CARTESIAN_POINT('',(-28.1835224437124,93.,-88.3939066694435));
#62254=CARTESIAN_POINT('',(-25.4952560959924,93.,-89.4458369794209));
#62255=CARTESIAN_POINT('',(-7.43918688281242,93.,-96.5112553671871));
#62256=CARTESIAN_POINT('',(-25.0621212935837,93.,-92.2999090836741));
#62257=CARTESIAN_POINT('',(-26.6933795895823,93.,-81.5509949545163));
#62258=CARTESIAN_POINT('',(-27.317252838895,93.,-94.1020508779497));
#62259=CARTESIAN_POINT('',(-2.54961709652947,93.,-74.3095063545433));
#62260=CARTESIAN_POINT('',(-30.005519186615,93.,-93.0501205679723));
#62261=CARTESIAN_POINT('',(-9.26118362571508,93.,-101.167469265716));
#62262=CARTESIAN_POINT('',(-30.4386539890237,93.,-90.1960484637193));
#62263=CARTESIAN_POINT('',(-31.6367774826137,93.,-82.3012064388147));
#62264=CARTESIAN_POINT('',(-5.67101824665825,93.,-70.4035039403128));
#62265=CARTESIAN_POINT('',(-21.1992015959193,93.,-91.1269017837974));
#62266=CARTESIAN_POINT('',(-18.5109352481993,93.,-92.1788320937748));
#62267=CARTESIAN_POINT('',(-7.43918688281242,93.,-96.5112553671871));
#62268=CARTESIAN_POINT('',(-18.0778004457905,93.,-95.0329041980279));
#62269=CARTESIAN_POINT('',(-20.2717173550128,93.,-80.5764416490967));
#62270=CARTESIAN_POINT('',(-20.3329319911019,93.,-96.8350459923036));
#62271=CARTESIAN_POINT('',(1.50520194059077,93.,-79.3835523314938));
#62272=CARTESIAN_POINT('',(-23.0211983388219,93.,-95.7831156823262));
#62273=CARTESIAN_POINT('',(-9.26118362571508,93.,-101.167469265716));
#62274=CARTESIAN_POINT('',(-23.4543331412306,93.,-92.9290435780731));
#62275=CARTESIAN_POINT('',(-25.2151152480442,93.,-81.326653133395));
#62276=CARTESIAN_POINT('',(-1.616199209538,93.,-75.4775499172633));
#62277=CARTESIAN_POINT('',(-14.2148807481261,93.,-93.8598968981513));
#62278=CARTESIAN_POINT('',(-11.5266144004061,93.,-94.9118272081287));
#62279=CARTESIAN_POINT('',(-7.43918688281243,93.,-96.5112553671872));
#62280=CARTESIAN_POINT('',(-11.0934795979974,93.,-97.7658993123818));
#62281=CARTESIAN_POINT('',(-13.8500551204433,93.,-79.601888343677));
#62282=CARTESIAN_POINT('',(-13.3486111433087,93.,-99.5680411066575));
#62283=CARTESIAN_POINT('',(5.56002097771102,93.,-84.4575983084442));
#62284=CARTESIAN_POINT('',(-16.0368774910288,93.,-98.5161107966801));
#62285=CARTESIAN_POINT('',(-9.26118362571508,93.,-101.167469265716));
#62286=CARTESIAN_POINT('',(-16.4700122934375,93.,-95.662038692427));
#62287=CARTESIAN_POINT('',(-18.7934530134748,93.,-80.3520998279754));
#62288=CARTESIAN_POINT('',(2.43861982758225,93.,-80.5515958942138));
#62289=CARTESIAN_POINT('',(-7.230559900333,93.,-96.5928920125052));
#62290=CARTESIAN_POINT('',(-4.54229355261299,93.,-97.6448223224826));
#62291=CARTESIAN_POINT('',(-7.43918688281243,93.,-96.5112553671872));
#62292=CARTESIAN_POINT('',(-4.10915875020428,93.,-100.498894426736));
#62293=CARTESIAN_POINT('',(-7.42839288587381,93.,-78.6273350382574));
#62294=CARTESIAN_POINT('',(-6.3642902955156,93.,-102.301036221011));
#62295=CARTESIAN_POINT('',(9.61484001483127,93.,-89.5316442853947));
#62296=CARTESIAN_POINT('',(-9.05255664323563,93.,-101.249105911034));
#62297=CARTESIAN_POINT('',(-9.26118362571508,93.,-101.167469265716));
#62298=CARTESIAN_POINT('',(-9.48569144564436,93.,-98.3950338067809));
#62299=CARTESIAN_POINT('',(-12.3717907789053,93.,-79.3775465225557));
#62300=CARTESIAN_POINT('',(6.4934388647025,93.,-85.6256418711642));
#62301=CARTESIAN_POINT('',(-0.246239052539871,93.,-99.3258871268591));
#62302=CARTESIAN_POINT('',(2.44202729518014,93.,-100.377817436837));
#62303=CARTESIAN_POINT('',(-7.43918688281244,93.,-96.5112553671872));
#62304=CARTESIAN_POINT('',(2.87516209758886,93.,-103.23188954109));
#62305=CARTESIAN_POINT('',(-1.00673065130432,93.,-77.6527817328378));
#62306=CARTESIAN_POINT('',(0.620030552277533,93.,-105.034031335365));
#62307=CARTESIAN_POINT('',(13.6696590519515,93.,-94.6056902623452));
#62308=CARTESIAN_POINT('',(-2.06823579544249,93.,-103.982101025388));
#62309=CARTESIAN_POINT('',(-9.26118362571508,93.,-101.167469265716));
#62310=CARTESIAN_POINT('',(-2.50137059785123,93.,-101.128028921135));
#62311=CARTESIAN_POINT('',(-5.95012854433585,93.,-78.4029932171361));
#62312=CARTESIAN_POINT('',(10.5482579018228,93.,-90.6996878481147));
#62313=CARTESIAN_POINT('',(6.73808179525326,93.,-102.058882241213));
#62314=CARTESIAN_POINT('',(9.42634814297327,93.,-103.11081255119));
#62315=CARTESIAN_POINT('',(-7.43918688281244,93.,-96.5112553671872));
#62316=CARTESIAN_POINT('',(9.85948294538199,93.,-105.964884655444));
#62317=CARTESIAN_POINT('',(5.41493158326516,93.,-76.6782284274182));
#62318=CARTESIAN_POINT('',(7.60435140007067,93.,-107.767026449719));
#62319=CARTESIAN_POINT('',(17.7244780890718,93.,-99.6797362392957));
#62320=CARTESIAN_POINT('',(4.91608505235064,93.,-106.715096139742));
#62321=CARTESIAN_POINT('',(-9.26118362571508,93.,-101.167469265716));
#62322=CARTESIAN_POINT('',(4.48295024994191,93.,-103.861024035489));
#62323=CARTESIAN_POINT('',(0.471533690233602,93.,-77.4284399117164));
#62324=CARTESIAN_POINT('',(14.603076938943,93.,-95.7737338250652));
#62325=CARTESIAN_POINT('',(13.7224026430464,93.,-104.791877355567));
#62326=CARTESIAN_POINT('',(16.4106689907664,93.,-105.843807665544));
#62327=CARTESIAN_POINT('',(-7.43918688281245,93.,-96.5112553671872));
#62328=CARTESIAN_POINT('',(16.8438037931751,93.,-108.697879769797));
#62329=CARTESIAN_POINT('',(11.8365938178346,93.,-75.7036751219986));
#62330=CARTESIAN_POINT('',(14.5886722478638,93.,-110.500021564073));
#62331=CARTESIAN_POINT('',(21.779297126192,93.,-104.753782216246));
#62332=CARTESIAN_POINT('',(11.9004059001438,93.,-109.448091254096));
#62333=CARTESIAN_POINT('',(-9.26118362571507,93.,-101.167469265716));
#62334=CARTESIAN_POINT('',(11.467271097735,93.,-106.594019149843));
#62335=CARTESIAN_POINT('',(6.89319592480305,93.,-76.4538866062968));
#62336=CARTESIAN_POINT('',(18.6578959760633,93.,-100.847779802016));
#62337=CARTESIAN_POINT('',(20.7067234908395,93.,-107.524872469921));
#62338=CARTESIAN_POINT('',(23.3949898385595,93.,-108.576802779898));
#62339=CARTESIAN_POINT('',(-7.43918688281245,93.,-96.5112553671872));
#62340=CARTESIAN_POINT('',(23.8281246409682,93.,-111.430874884151));
#62341=CARTESIAN_POINT('',(18.2582560524041,93.,-74.729121816579));
#62342=CARTESIAN_POINT('',(21.5729930956569,93.,-113.233016678427));
#62343=CARTESIAN_POINT('',(25.8341161633122,93.,-109.827828193197));
#62344=CARTESIAN_POINT('',(18.8847267479369,93.,-112.18108636845));
#62345=CARTESIAN_POINT('',(-9.26118362571507,93.,-101.167469265716));
#62346=CARTESIAN_POINT('',(18.4515919455282,93.,-109.327014264196));
#62347=CARTESIAN_POINT('',(13.3148581593725,93.,-75.4793333008771));
#62348=CARTESIAN_POINT('',(22.7127150131835,93.,-105.921825778966));
#62349=CARTESIAN_POINT('',(27.6910443386327,93.,-110.257867584275));
#62350=CARTESIAN_POINT('',(30.3793106863527,93.,-111.309797894252));
#62351=CARTESIAN_POINT('',(-7.43918688281246,93.,-96.5112553671872));
#62352=CARTESIAN_POINT('',(30.8124454887614,93.,-114.163869998505));
#62353=CARTESIAN_POINT('',(24.6799182869736,93.,-73.7545685111594));
#62354=CARTESIAN_POINT('',(28.5573139434501,93.,-115.966011792781));
#62355=CARTESIAN_POINT('',(29.8889352004325,93.,-114.901874170147));
#62356=CARTESIAN_POINT('',(25.86904759573,93.,-114.914081482803));
#62357=CARTESIAN_POINT('',(-9.26118362571507,93.,-101.167469265716));
#62358=CARTESIAN_POINT('',(25.4359127933213,93.,-112.06000937855));
#62359=CARTESIAN_POINT('',(19.736520393942,93.,-74.5047799954575));
#62360=CARTESIAN_POINT('',(26.7675340503038,93.,-110.995871755917));
#62361=CARTESIAN_POINT('',(2.46923037857264,93.,-30.6409089600963));
#62362=CARTESIAN_POINT('',(5.15749672629266,93.,-31.6928392700737));
#62363=CARTESIAN_POINT('',(16.2292450916797,93.,-36.0252625434861));
#62364=CARTESIAN_POINT('',(5.59063152870137,93.,-34.5469113743268));
#62365=CARTESIAN_POINT('',(11.8365938178339,93.,-75.7036751219987));
#62366=CARTESIAN_POINT('',(3.33549998339005,93.,-36.3490531686025));
#62367=CARTESIAN_POINT('',(-18.7688932450105,93.,-54.0133224467414));
#62368=CARTESIAN_POINT('',(0.647233635670021,93.,-35.2971228586251));
#62369=CARTESIAN_POINT('',(14.4072483487771,93.,-40.6814764420149));
#62370=CARTESIAN_POINT('',(0.214098833261289,93.,-32.443050754372));
#62371=CARTESIAN_POINT('',(6.89319592480286,93.,-76.4538866062968));
#62372=CARTESIAN_POINT('',(-21.8902943951393,93.,-50.1073200325109));
#62373=CARTESIAN_POINT('',(-4.51509046922049,93.,-27.9079138457424));
#62374=CARTESIAN_POINT('',(-1.82682412150048,93.,-28.9598441557198));
#62375=CARTESIAN_POINT('',(16.2292450916797,93.,-36.0252625434861));
#62376=CARTESIAN_POINT('',(-1.39368931909176,93.,-31.8139162599729));
#62377=CARTESIAN_POINT('',(5.41493158326445,93.,-76.6782284274183));
#62378=CARTESIAN_POINT('',(-3.64882086440308,93.,-33.6160580542486));
#62379=CARTESIAN_POINT('',(-22.8237122821307,93.,-48.9392764697909));
#62380=CARTESIAN_POINT('',(-6.33708721212311,93.,-32.5641277442712));
#62381=CARTESIAN_POINT('',(14.4072483487771,93.,-40.6814764420149));
#62382=CARTESIAN_POINT('',(-6.77022201453184,93.,-29.7100556400181));
#62383=CARTESIAN_POINT('',(0.471533690233403,93.,-77.4284399117165));
#62384=CARTESIAN_POINT('',(-25.9451134322595,93.,-45.0332740555604));
#62385=CARTESIAN_POINT('',(-11.4994113170136,93.,-25.1749187313885));
#62386=CARTESIAN_POINT('',(-8.81114496929361,93.,-26.2268490413659));
#62387=CARTESIAN_POINT('',(16.2292450916797,93.,-36.0252625434861));
#62388=CARTESIAN_POINT('',(-8.37801016688489,93.,-29.080921145619));
#62389=CARTESIAN_POINT('',(-1.00673065130503,93.,-77.6527817328379));
#62390=CARTESIAN_POINT('',(-10.6331417121962,93.,-30.8830629398947));
#62391=CARTESIAN_POINT('',(-26.878531319251,93.,-43.8652304928404));
#62392=CARTESIAN_POINT('',(-13.3214080599162,93.,-29.8311326299173));
#62393=CARTESIAN_POINT('',(14.4072483487771,93.,-40.6814764420149));
#62394=CARTESIAN_POINT('',(-13.754542862325,93.,-26.9770605256642));
#62395=CARTESIAN_POINT('',(-5.95012854433605,93.,-78.4029932171361));
#62396=CARTESIAN_POINT('',(-29.9999324693798,93.,-39.9592280786099));
#62397=CARTESIAN_POINT('',(45.5004726917788,93.,-54.4539764857667));
#62398=CARTESIAN_POINT('',(48.1887390394988,93.,-55.5059067957441));
#62399=CARTESIAN_POINT('',(13.8624018942304,93.,-42.0738618258563));
#62400=CARTESIAN_POINT('',(48.6218738419075,93.,-58.3599788999972));
#62401=CARTESIAN_POINT('',(50.3665672252509,93.,-69.856355289481));
#62402=CARTESIAN_POINT('',(46.3667422965962,93.,-60.1621206942729));
#62403=CARTESIAN_POINT('',(9.61484001483123,93.,-89.5316442853947));
#62404=CARTESIAN_POINT('',(43.6784759488762,93.,-59.1101903842955));
#62405=CARTESIAN_POINT('',(12.0404051513279,93.,-46.730075724385));
#62406=CARTESIAN_POINT('',(43.2453411464674,93.,-56.2561182800424));
#62407=CARTESIAN_POINT('',(45.4231693322196,93.,-70.6065667737789));
#62408=CARTESIAN_POINT('',(6.4934388647025,93.,-85.6256418711642));
#62409=CARTESIAN_POINT('',(9.45355122636578,93.,-33.3739040744502));
#62410=CARTESIAN_POINT('',(12.1418175740858,93.,-34.4258343844276));
#62411=CARTESIAN_POINT('',(16.2292450916796,93.,-36.0252625434861));
#62412=CARTESIAN_POINT('',(12.5749523764945,93.,-37.2799064886807));
#62413=CARTESIAN_POINT('',(18.2582560524034,93.,-74.7291218165791));
#62414=CARTESIAN_POINT('',(10.3198208311832,93.,-39.0820482829564));
#62415=CARTESIAN_POINT('',(-14.7140742078902,93.,-59.0873684236918));
#62416=CARTESIAN_POINT('',(7.63155448346315,93.,-38.030117972979));
#62417=CARTESIAN_POINT('',(14.4072483487771,93.,-40.6814764420149));
#62418=CARTESIAN_POINT('',(7.19841968105442,93.,-35.1760458687259));
#62419=CARTESIAN_POINT('',(13.3148581593723,93.,-75.4793333008772));
#62420=CARTESIAN_POINT('',(-17.835475358019,93.,-55.1813660094614));
#62421=CARTESIAN_POINT('',(16.4378720741589,93.,-36.1068991888041));
#62422=CARTESIAN_POINT('',(19.1261384218789,93.,-37.1588294987815));
#62423=CARTESIAN_POINT('',(16.2292450916796,93.,-36.0252625434861));
#62424=CARTESIAN_POINT('',(19.5592732242876,93.,-40.0129016030346));
#62425=CARTESIAN_POINT('',(24.6799182869729,93.,-73.7545685111595));
#62426=CARTESIAN_POINT('',(17.3041416789763,93.,-41.8150433973103));
#62427=CARTESIAN_POINT('',(-10.65925517077,93.,-64.1614144006423));
#62428=CARTESIAN_POINT('',(14.6158753312563,93.,-40.7631130873329));
#62429=CARTESIAN_POINT('',(14.4072483487771,93.,-40.6814764420149));
#62430=CARTESIAN_POINT('',(14.1827405288475,93.,-37.9090409830798));
#62431=CARTESIAN_POINT('',(19.7365203939418,93.,-74.5047799954575));
#62432=CARTESIAN_POINT('',(-13.7806563208988,93.,-60.2554119864119));
#62433=CARTESIAN_POINT('',(23.422192921952,93.,-38.839894303158));
#62434=CARTESIAN_POINT('',(26.110459269672,93.,-39.8918246131354));
#62435=CARTESIAN_POINT('',(16.2292450916796,93.,-36.0252625434861));
#62436=CARTESIAN_POINT('',(26.5435940720808,93.,-42.7458967173885));
#62437=CARTESIAN_POINT('',(31.1015805215424,93.,-72.7800152057398));
#62438=CARTESIAN_POINT('',(24.2884625267694,93.,-44.5480385116642));
#62439=CARTESIAN_POINT('',(-6.60443613364976,93.,-69.2354603775928));
#62440=CARTESIAN_POINT('',(21.6001961790494,93.,-43.4961082016867));
#62441=CARTESIAN_POINT('',(14.4072483487771,93.,-40.6814764420149));
#62442=CARTESIAN_POINT('',(21.1670613766407,93.,-40.6420360974337));
#62443=CARTESIAN_POINT('',(26.1581826285112,93.,-73.5302266900378));
#62444=CARTESIAN_POINT('',(-9.7258372837785,93.,-65.3294579633623));
#62445=CARTESIAN_POINT('',(30.4065137697452,93.,-41.5728894175119));
#62446=CARTESIAN_POINT('',(33.0947801174652,93.,-42.6248197274893));
#62447=CARTESIAN_POINT('',(16.2292450916796,93.,-36.0252625434861));
#62448=CARTESIAN_POINT('',(33.5279149198739,93.,-45.4788918317424));
#62449=CARTESIAN_POINT('',(37.5232427561119,93.,-71.8054619003202));
#62450=CARTESIAN_POINT('',(31.2727833745626,93.,-47.2810336260181));
#62451=CARTESIAN_POINT('',(-2.54961709652951,93.,-74.3095063545433));
#62452=CARTESIAN_POINT('',(28.5845170268425,93.,-46.2291033160406));
#62453=CARTESIAN_POINT('',(14.4072483487771,93.,-40.6814764420149));
#62454=CARTESIAN_POINT('',(28.1513822244338,93.,-43.3750312117876));
#62455=CARTESIAN_POINT('',(32.5798448630807,93.,-72.5556733846182));
#62456=CARTESIAN_POINT('',(-5.67101824665825,93.,-70.4035039403128));
#62457=CARTESIAN_POINT('',(38.5161518439857,93.,-51.7209813714128));
#62458=CARTESIAN_POINT('',(41.2044181917057,93.,-52.7729116813902));
#62459=CARTESIAN_POINT('',(13.8624018942304,93.,-42.0738618258563));
#62460=CARTESIAN_POINT('',(41.6375529941144,93.,-55.6269837856433));
#62461=CARTESIAN_POINT('',(43.9449049906814,93.,-70.8309085949006));
#62462=CARTESIAN_POINT('',(39.3824214488031,93.,-57.429125579919));
#62463=CARTESIAN_POINT('',(5.56002097771098,93.,-84.4575983084442));
#62464=CARTESIAN_POINT('',(36.694155101083,93.,-56.3771952699416));
#62465=CARTESIAN_POINT('',(12.0404051513279,93.,-46.730075724385));
#62466=CARTESIAN_POINT('',(36.2610202986743,93.,-53.5231231656885));
#62467=CARTESIAN_POINT('',(39.0015070976501,93.,-71.5811200791985));
#62468=CARTESIAN_POINT('',(2.43861982758225,93.,-80.5515958942137));
#62469=CARTESIAN_POINT('',(31.5318309961925,93.,-48.9879862570589));
#62470=CARTESIAN_POINT('',(34.2200973439125,93.,-50.0399165670363));
#62471=CARTESIAN_POINT('',(13.8624018942304,93.,-42.0738618258563));
#62472=CARTESIAN_POINT('',(34.6532321463213,93.,-52.8939886712894));
#62473=CARTESIAN_POINT('',(37.5232427561119,93.,-71.8054619003202));
#62474=CARTESIAN_POINT('',(32.3981006010099,93.,-54.6961304655651));
#62475=CARTESIAN_POINT('',(1.50520194059074,93.,-79.3835523314937));
#62476=CARTESIAN_POINT('',(29.7098342532899,93.,-53.6442001555877));
#62477=CARTESIAN_POINT('',(12.0404051513279,93.,-46.730075724385));
#62478=CARTESIAN_POINT('',(29.2766994508812,93.,-50.7901280513346));
#62479=CARTESIAN_POINT('',(32.5798448630807,93.,-72.5556733846182));
#62480=CARTESIAN_POINT('',(-1.616199209538,93.,-75.4775499172633));
#62481=CARTESIAN_POINT('',(24.5475101483994,93.,-46.254991142705));
#62482=CARTESIAN_POINT('',(27.2357764961194,93.,-47.3069214526824));
#62483=CARTESIAN_POINT('',(13.8624018942304,93.,-42.0738618258562));
#62484=CARTESIAN_POINT('',(27.6689112985281,93.,-50.1609935569356));
#62485=CARTESIAN_POINT('',(31.1015805215425,93.,-72.7800152057398));
#62486=CARTESIAN_POINT('',(25.4137797532168,93.,-51.9631353512112));
#62487=CARTESIAN_POINT('',(-2.5496170965295,93.,-74.3095063545433));
#62488=CARTESIAN_POINT('',(22.7255134054968,93.,-50.9112050412338));
#62489=CARTESIAN_POINT('',(12.0404051513279,93.,-46.730075724385));
#62490=CARTESIAN_POINT('',(22.2923786030881,93.,-48.0571329369807));
#62491=CARTESIAN_POINT('',(26.1581826285112,93.,-73.5302266900378));
#62492=CARTESIAN_POINT('',(-5.67101824665825,93.,-70.4035039403128));
#62493=CARTESIAN_POINT('',(17.5631893006063,93.,-43.5219960283511));
#62494=CARTESIAN_POINT('',(20.2514556483263,93.,-44.5739263383286));
#62495=CARTESIAN_POINT('',(13.8624018942304,93.,-42.0738618258562));
#62496=CARTESIAN_POINT('',(20.684590450735,93.,-47.4279984425817));
#62497=CARTESIAN_POINT('',(24.679918286973,93.,-73.7545685111594));
#62498=CARTESIAN_POINT('',(18.4294589054237,93.,-49.2301402368573));
#62499=CARTESIAN_POINT('',(-6.60443613364975,93.,-69.2354603775928));
#62500=CARTESIAN_POINT('',(15.7411925577037,93.,-48.1782099268799));
#62501=CARTESIAN_POINT('',(12.0404051513279,93.,-46.730075724385));
#62502=CARTESIAN_POINT('',(15.3080577552949,93.,-45.3241378226269));
#62503=CARTESIAN_POINT('',(19.7365203939418,93.,-74.5047799954575));
#62504=CARTESIAN_POINT('',(-9.7258372837785,93.,-65.3294579633623));
#62505=CARTESIAN_POINT('',(10.5788684528132,93.,-40.7890009139973));
#62506=CARTESIAN_POINT('',(13.2671348005332,93.,-41.8409312239747));
#62507=CARTESIAN_POINT('',(13.8624018942304,93.,-42.0738618258562));
#62508=CARTESIAN_POINT('',(13.7002696029419,93.,-44.6950033282278));
#62509=CARTESIAN_POINT('',(18.2582560524035,93.,-74.7291218165791));
#62510=CARTESIAN_POINT('',(11.4451380576306,93.,-46.4971451225034));
#62511=CARTESIAN_POINT('',(-10.65925517077,93.,-64.1614144006423));
#62512=CARTESIAN_POINT('',(8.75687170991053,93.,-45.445214812526));
#62513=CARTESIAN_POINT('',(12.0404051513279,93.,-46.730075724385));
#62514=CARTESIAN_POINT('',(8.32373690750179,93.,-42.591142708273));
#62515=CARTESIAN_POINT('',(13.3148581593723,93.,-75.4793333008771));
#62516=CARTESIAN_POINT('',(-13.7806563208988,93.,-60.2554119864119));
#62517=CARTESIAN_POINT('',(3.59454760502002,93.,-38.0560057996434));
#62518=CARTESIAN_POINT('',(6.28281395274003,93.,-39.1079361096208));
#62519=CARTESIAN_POINT('',(13.8624018942304,93.,-42.0738618258562));
#62520=CARTESIAN_POINT('',(6.71594875514875,93.,-41.9620082138739));
#62521=CARTESIAN_POINT('',(11.836593817834,93.,-75.7036751219987));
#62522=CARTESIAN_POINT('',(4.46081720983743,93.,-43.7641500081495));
#62523=CARTESIAN_POINT('',(-14.7140742078902,93.,-59.0873684236918));
#62524=CARTESIAN_POINT('',(1.7725508621174,93.,-42.7122196981721));
#62525=CARTESIAN_POINT('',(12.0404051513279,93.,-46.730075724385));
#62526=CARTESIAN_POINT('',(1.33941605970866,93.,-39.8581475939191));
#62527=CARTESIAN_POINT('',(6.89319592480288,93.,-76.4538866062968));
#62528=CARTESIAN_POINT('',(-17.835475358019,93.,-55.1813660094614));
#62529=CARTESIAN_POINT('',(-3.38977324277311,93.,-35.3230106852895));
#62530=CARTESIAN_POINT('',(-0.701506895053102,93.,-36.3749409952669));
#62531=CARTESIAN_POINT('',(13.8624018942304,93.,-42.0738618258562));
#62532=CARTESIAN_POINT('',(-0.268372092644385,93.,-39.22901309952));
#62533=CARTESIAN_POINT('',(5.41493158326452,93.,-76.6782284274183));
#62534=CARTESIAN_POINT('',(-2.52350363795571,93.,-41.0311548937957));
#62535=CARTESIAN_POINT('',(-18.7688932450105,93.,-54.0133224467414));
#62536=CARTESIAN_POINT('',(-5.21176998567574,93.,-39.9792245838182));
#62537=CARTESIAN_POINT('',(12.0404051513279,93.,-46.730075724385));
#62538=CARTESIAN_POINT('',(-5.64490478808447,93.,-37.1251524795652));
#62539=CARTESIAN_POINT('',(0.471533690233424,93.,-77.4284399117165));
#62540=CARTESIAN_POINT('',(-21.8902943951393,93.,-50.1073200325109));
#62541=CARTESIAN_POINT('',(-10.3740940905662,93.,-32.5900155709356));
#62542=CARTESIAN_POINT('',(-7.68582774284623,93.,-33.641945880913));
#62543=CARTESIAN_POINT('',(13.8624018942304,93.,-42.0738618258562));
#62544=CARTESIAN_POINT('',(-7.25269294043752,93.,-36.4960179851661));
#62545=CARTESIAN_POINT('',(-1.00673065130496,93.,-77.6527817328379));
#62546=CARTESIAN_POINT('',(-9.50782448574884,93.,-38.2981597794418));
#62547=CARTESIAN_POINT('',(-22.8237122821307,93.,-48.9392764697909));
#62548=CARTESIAN_POINT('',(-12.1960908334689,93.,-37.2462294694643));
#62549=CARTESIAN_POINT('',(12.0404051513279,93.,-46.730075724385));
#62550=CARTESIAN_POINT('',(-12.6292256358776,93.,-34.3921573652113));
#62551=CARTESIAN_POINT('',(-5.95012854433603,93.,-78.4029932171361));
#62552=CARTESIAN_POINT('',(-25.9451134322595,93.,-45.0332740555604));
#62553=CARTESIAN_POINT('',(36.2655173910909,93.,-36.8907876923187));
#62554=CARTESIAN_POINT('',(38.9537837388109,93.,-37.9427180022961));
#62555=CARTESIAN_POINT('',(18.5960882891288,93.,-29.976663261116));
#62556=CARTESIAN_POINT('',(39.3869185412196,93.,-40.7967901065492));
#62557=CARTESIAN_POINT('',(43.9449049906813,93.,-70.8309085949006));
#62558=CARTESIAN_POINT('',(37.1317869959083,93.,-42.5989319008249));
#62559=CARTESIAN_POINT('',(-2.54961709652952,93.,-74.3095063545432));
#62560=CARTESIAN_POINT('',(34.4435206481883,93.,-41.5470015908475));
#62561=CARTESIAN_POINT('',(16.7740915462264,93.,-34.6328771596448));
#62562=CARTESIAN_POINT('',(34.0103858457796,93.,-38.6929294865944));
#62563=CARTESIAN_POINT('',(39.0015070976501,93.,-71.5811200791985));
#62564=CARTESIAN_POINT('',(-5.67101824665826,93.,-70.4035039403128));
#62565=CARTESIAN_POINT('',(29.2811965432978,93.,-34.1577925779648));
#62566=CARTESIAN_POINT('',(31.9694628910178,93.,-35.2097228879422));
#62567=CARTESIAN_POINT('',(18.5960882891288,93.,-29.976663261116));
#62568=CARTESIAN_POINT('',(32.4025976934265,93.,-38.0637949921953));
#62569=CARTESIAN_POINT('',(37.5232427561118,93.,-71.8054619003203));
#62570=CARTESIAN_POINT('',(30.1474661481152,93.,-39.865936786471));
#62571=CARTESIAN_POINT('',(-6.60443613364976,93.,-69.2354603775928));
#62572=CARTESIAN_POINT('',(27.4591998003952,93.,-38.8140064764936));
#62573=CARTESIAN_POINT('',(16.7740915462264,93.,-34.6328771596448));
#62574=CARTESIAN_POINT('',(27.0260649979864,93.,-35.9599343722405));
#62575=CARTESIAN_POINT('',(32.5798448630806,93.,-72.5556733846182));
#62576=CARTESIAN_POINT('',(-9.72583728377851,93.,-65.3294579633623));
#62577=CARTESIAN_POINT('',(22.2968756955047,93.,-31.4247974636109));
#62578=CARTESIAN_POINT('',(24.9851420432247,93.,-32.4767277735883));
#62579=CARTESIAN_POINT('',(18.5960882891288,93.,-29.976663261116));
#62580=CARTESIAN_POINT('',(25.4182768456334,93.,-35.3307998778414));
#62581=CARTESIAN_POINT('',(31.1015805215423,93.,-72.7800152057399));
#62582=CARTESIAN_POINT('',(23.1631453003221,93.,-37.1329416721171));
#62583=CARTESIAN_POINT('',(-10.65925517077,93.,-64.1614144006423));
#62584=CARTESIAN_POINT('',(20.474878952602,93.,-36.0810113621397));
#62585=CARTESIAN_POINT('',(16.7740915462264,93.,-34.6328771596448));
#62586=CARTESIAN_POINT('',(20.0417441501933,93.,-33.2269392578866));
#62587=CARTESIAN_POINT('',(26.1581826285112,93.,-73.5302266900378));
#62588=CARTESIAN_POINT('',(-13.7806563208988,93.,-60.2554119864118));
#62589=CARTESIAN_POINT('',(15.3125548477115,93.,-28.691802349257));
#62590=CARTESIAN_POINT('',(18.0008211954315,93.,-29.7437326592344));
#62591=CARTESIAN_POINT('',(18.5960882891289,93.,-29.976663261116));
#62592=CARTESIAN_POINT('',(18.4339559978403,93.,-32.5978047634875));
#62593=CARTESIAN_POINT('',(24.6799182869728,93.,-73.7545685111595));
#62594=CARTESIAN_POINT('',(16.1788244525289,93.,-34.3999465577632));
#62595=CARTESIAN_POINT('',(-14.7140742078902,93.,-59.0873684236918));
#62596=CARTESIAN_POINT('',(13.4905581048089,93.,-33.3480162477858));
#62597=CARTESIAN_POINT('',(16.7740915462264,93.,-34.6328771596448));
#62598=CARTESIAN_POINT('',(13.0574233024002,93.,-30.4939441435327));
#62599=CARTESIAN_POINT('',(19.7365203939417,93.,-74.5047799954575));
#62600=CARTESIAN_POINT('',(-17.835475358019,93.,-55.1813660094614));
#62601=CARTESIAN_POINT('',(8.3282339999184,93.,-25.9588072349031));
#62602=CARTESIAN_POINT('',(11.0165003476384,93.,-27.0107375448806));
#62603=CARTESIAN_POINT('',(18.5960882891289,93.,-29.976663261116));
#62604=CARTESIAN_POINT('',(11.4496351500471,93.,-29.8648096491337));
#62605=CARTESIAN_POINT('',(18.2582560524034,93.,-74.7291218165791));
#62606=CARTESIAN_POINT('',(9.1945036047358,93.,-31.6669514434093));
#62607=CARTESIAN_POINT('',(-18.7688932450105,93.,-54.0133224467413));
#62608=CARTESIAN_POINT('',(6.50623725701577,93.,-30.6150211334319));
#62609=CARTESIAN_POINT('',(16.7740915462264,93.,-34.6328771596448));
#62610=CARTESIAN_POINT('',(6.07310245460704,93.,-27.7609490291788));
#62611=CARTESIAN_POINT('',(13.3148581593723,93.,-75.4793333008772));
#62612=CARTESIAN_POINT('',(-21.8902943951393,93.,-50.1073200325109));
#62613=CARTESIAN_POINT('',(1.34391315212527,93.,-23.2258121205493));
#62614=CARTESIAN_POINT('',(4.03217949984528,93.,-24.2777424305267));
#62615=CARTESIAN_POINT('',(18.5960882891289,93.,-29.976663261116));
#62616=CARTESIAN_POINT('',(4.465314302254,93.,-27.1318145347798));
#62617=CARTESIAN_POINT('',(11.8365938178339,93.,-75.7036751219987));
#62618=CARTESIAN_POINT('',(2.21018275694267,93.,-28.9339563290554));
#62619=CARTESIAN_POINT('',(-22.8237122821307,93.,-48.9392764697909));
#62620=CARTESIAN_POINT('',(-0.478083590777355,93.,-27.882026019078));
#62621=CARTESIAN_POINT('',(16.7740915462264,93.,-34.6328771596448));
#62622=CARTESIAN_POINT('',(-0.911218393186086,93.,-25.0279539148249));
#62623=CARTESIAN_POINT('',(6.89319592480284,93.,-76.4538866062968));
#62624=CARTESIAN_POINT('',(-25.9451134322595,93.,-45.0332740555604));
#62625=CARTESIAN_POINT('',(44.3751554653314,93.,-47.0388796462197));
#62626=CARTESIAN_POINT('',(47.0634218130514,93.,-48.0908099561971));
#62627=CARTESIAN_POINT('',(16.2292450916796,93.,-36.0252625434862));
#62628=CARTESIAN_POINT('',(47.4965566154602,93.,-50.9448820604502));
#62629=CARTESIAN_POINT('',(50.3665672252508,93.,-69.856355289481));
#62630=CARTESIAN_POINT('',(45.2414250701488,93.,-52.7470238547258));
#62631=CARTESIAN_POINT('',(5.56002097771098,93.,-84.4575983084442));
#62632=CARTESIAN_POINT('',(42.5531587224288,93.,-51.6950935447484));
#62633=CARTESIAN_POINT('',(14.4072483487771,93.,-40.6814764420149));
#62634=CARTESIAN_POINT('',(42.1200239200201,93.,-48.8410214404954));
#62635=CARTESIAN_POINT('',(45.4231693322196,93.,-70.6065667737789));
#62636=CARTESIAN_POINT('',(2.43861982758225,93.,-80.5515958942138));
#62637=CARTESIAN_POINT('',(37.3908346175383,93.,-44.3058845318658));
#62638=CARTESIAN_POINT('',(40.0791009652583,93.,-45.3578148418432));
#62639=CARTESIAN_POINT('',(16.2292450916796,93.,-36.0252625434862));
#62640=CARTESIAN_POINT('',(40.512235767667,93.,-48.2118869460963));
#62641=CARTESIAN_POINT('',(43.9449049906814,93.,-70.8309085949006));
#62642=CARTESIAN_POINT('',(38.2571042223557,93.,-50.014028740372));
#62643=CARTESIAN_POINT('',(1.50520194059074,93.,-79.3835523314937));
#62644=CARTESIAN_POINT('',(35.5688378746357,93.,-48.9620984303945));
#62645=CARTESIAN_POINT('',(14.4072483487771,93.,-40.6814764420149));
#62646=CARTESIAN_POINT('',(35.1357030722269,93.,-46.1080263261415));
#62647=CARTESIAN_POINT('',(39.0015070976501,93.,-71.5811200791985));
#62648=CARTESIAN_POINT('',(-1.616199209538,93.,-75.4775499172633));
#62649=CARTESIAN_POINT('',(33.7824654490873,93.,-63.818179936153));
#62650=CARTESIAN_POINT('',(36.4707317968073,93.,-64.8701102461305));
#62651=CARTESIAN_POINT('',(9.128715499332,93.,-54.1710603905965));
#62652=CARTESIAN_POINT('',(36.903866599216,93.,-67.7241823503836));
#62653=CARTESIAN_POINT('',(37.5232427561121,93.,-71.8054619003202));
#62654=CARTESIAN_POINT('',(34.6487350539047,93.,-69.5263241446592));
#62655=CARTESIAN_POINT('',(9.61484001483124,93.,-89.5316442853947));
#62656=CARTESIAN_POINT('',(31.9604687061847,93.,-68.4743938346818));
#62657=CARTESIAN_POINT('',(7.30671875642947,93.,-58.8272742891252));
#62658=CARTESIAN_POINT('',(31.5273339037759,93.,-65.6203217304287));
#62659=CARTESIAN_POINT('',(32.5798448630807,93.,-72.5556733846182));
#62660=CARTESIAN_POINT('',(6.4934388647025,93.,-85.6256418711642));
#62661=CARTESIAN_POINT('',(26.7981446012942,93.,-61.0851848217992));
#62662=CARTESIAN_POINT('',(29.4864109490142,93.,-62.1371151317766));
#62663=CARTESIAN_POINT('',(9.128715499332,93.,-54.1710603905965));
#62664=CARTESIAN_POINT('',(29.9195457514229,93.,-64.9911872360297));
#62665=CARTESIAN_POINT('',(31.1015805215426,93.,-72.7800152057398));
#62666=CARTESIAN_POINT('',(27.6644142061116,93.,-66.7933290303053));
#62667=CARTESIAN_POINT('',(5.560020977711,93.,-84.4575983084442));
#62668=CARTESIAN_POINT('',(24.9761478583915,93.,-65.7413987203279));
#62669=CARTESIAN_POINT('',(7.30671875642947,93.,-58.8272742891252));
#62670=CARTESIAN_POINT('',(24.5430130559828,93.,-62.8873266160749));
#62671=CARTESIAN_POINT('',(26.1581826285113,93.,-73.5302266900378));
#62672=CARTESIAN_POINT('',(2.43861982758225,93.,-80.5515958942138));
#62673=CARTESIAN_POINT('',(19.813823753501,93.,-58.3521897074453));
#62674=CARTESIAN_POINT('',(22.502090101221,93.,-59.4041200174227));
#62675=CARTESIAN_POINT('',(9.12871549933201,93.,-54.1710603905965));
#62676=CARTESIAN_POINT('',(22.9352249036298,93.,-62.2581921216758));
#62677=CARTESIAN_POINT('',(24.6799182869731,93.,-73.7545685111594));
#62678=CARTESIAN_POINT('',(20.6800933583184,93.,-64.0603339159514));
#62679=CARTESIAN_POINT('',(1.50520194059075,93.,-79.3835523314937));
#62680=CARTESIAN_POINT('',(17.9918270105984,93.,-63.008403605974));
#62681=CARTESIAN_POINT('',(7.30671875642947,93.,-58.8272742891252));
#62682=CARTESIAN_POINT('',(17.5586922081897,93.,-60.154331501721));
#62683=CARTESIAN_POINT('',(19.7365203939418,93.,-74.5047799954575));
#62684=CARTESIAN_POINT('',(-1.616199209538,93.,-75.4775499172633));
#62685=CARTESIAN_POINT('',(12.8295029057079,93.,-55.6191945930914));
#62686=CARTESIAN_POINT('',(15.5177692534279,93.,-56.6711249030688));
#62687=CARTESIAN_POINT('',(9.12871549933201,93.,-54.1710603905965));
#62688=CARTESIAN_POINT('',(15.9509040558366,93.,-59.5251970073219));
#62689=CARTESIAN_POINT('',(18.2582560524036,93.,-74.7291218165791));
#62690=CARTESIAN_POINT('',(13.6957725105253,93.,-61.3273388015976));
#62691=CARTESIAN_POINT('',(-2.54961709652949,93.,-74.3095063545433));
#62692=CARTESIAN_POINT('',(11.0075061628053,93.,-60.2754084916201));
#62693=CARTESIAN_POINT('',(7.30671875642947,93.,-58.8272742891252));
#62694=CARTESIAN_POINT('',(10.5743713603965,93.,-57.4213363873671));
#62695=CARTESIAN_POINT('',(13.3148581593724,93.,-75.4793333008771));
#62696=CARTESIAN_POINT('',(-5.67101824665825,93.,-70.4035039403128));
#62697=CARTESIAN_POINT('',(5.84518205791477,93.,-52.8861994787375));
#62698=CARTESIAN_POINT('',(8.53344840563478,93.,-53.9381297887149));
#62699=CARTESIAN_POINT('',(9.12871549933202,93.,-54.1710603905964));
#62700=CARTESIAN_POINT('',(8.9665832080435,93.,-56.792201892968));
#62701=CARTESIAN_POINT('',(11.8365938178341,93.,-75.7036751219987));
#62702=CARTESIAN_POINT('',(6.71145166273218,93.,-58.5943436872437));
#62703=CARTESIAN_POINT('',(-6.60443613364974,93.,-69.2354603775928));
#62704=CARTESIAN_POINT('',(4.02318531501215,93.,-57.5424133772663));
#62705=CARTESIAN_POINT('',(7.30671875642947,93.,-58.8272742891252));
#62706=CARTESIAN_POINT('',(3.59005051260342,93.,-54.6883412730132));
#62707=CARTESIAN_POINT('',(6.89319592480292,93.,-76.4538866062968));
#62708=CARTESIAN_POINT('',(-9.7258372837785,93.,-65.3294579633623));
#62709=CARTESIAN_POINT('',(-1.13913878987836,93.,-50.1532043643836));
#62710=CARTESIAN_POINT('',(1.54912755784165,93.,-51.205134674361));
#62711=CARTESIAN_POINT('',(9.12871549933202,93.,-54.1710603905964));
#62712=CARTESIAN_POINT('',(1.98226236025037,93.,-54.0592067786141));
#62713=CARTESIAN_POINT('',(5.41493158326467,93.,-76.6782284274183));
#62714=CARTESIAN_POINT('',(-0.272869185060958,93.,-55.8613485728898));
#62715=CARTESIAN_POINT('',(-10.65925517077,93.,-64.1614144006423));
#62716=CARTESIAN_POINT('',(-2.96113553278099,93.,-54.8094182629124));
#62717=CARTESIAN_POINT('',(7.30671875642947,93.,-58.8272742891252));
#62718=CARTESIAN_POINT('',(-3.39427033518972,93.,-51.9553461586593));
#62719=CARTESIAN_POINT('',(0.471533690233463,93.,-77.4284399117164));
#62720=CARTESIAN_POINT('',(-13.7806563208987,93.,-60.2554119864119));
#62721=CARTESIAN_POINT('',(-8.12345963767149,93.,-47.4202092500297));
#62722=CARTESIAN_POINT('',(-5.43519328995148,93.,-48.4721395600071));
#62723=CARTESIAN_POINT('',(9.12871549933203,93.,-54.1710603905964));
#62724=CARTESIAN_POINT('',(-5.00205848754277,93.,-51.3262116642602));
#62725=CARTESIAN_POINT('',(-1.00673065130482,93.,-77.6527817328379));
#62726=CARTESIAN_POINT('',(-7.25719003285409,93.,-53.1283534585359));
#62727=CARTESIAN_POINT('',(-14.7140742078902,93.,-59.0873684236919));
#62728=CARTESIAN_POINT('',(-9.94545638057412,93.,-52.0764231485585));
#62729=CARTESIAN_POINT('',(7.30671875642947,93.,-58.8272742891252));
#62730=CARTESIAN_POINT('',(-10.3785911829829,93.,-49.2223510443054));
#62731=CARTESIAN_POINT('',(-5.95012854433599,93.,-78.4029932171361));
#62732=CARTESIAN_POINT('',(-17.835475358019,93.,-55.1813660094614));
#62733=CARTESIAN_POINT('',(-15.1077804854646,93.,-44.6872141356758));
#62734=CARTESIAN_POINT('',(-12.4195141377446,93.,-45.7391444456532));
#62735=CARTESIAN_POINT('',(9.12871549933203,93.,-54.1710603905964));
#62736=CARTESIAN_POINT('',(-11.9863793353359,93.,-48.5932165499063));
#62737=CARTESIAN_POINT('',(-7.4283928858743,93.,-78.6273350382575));
#62738=CARTESIAN_POINT('',(-14.2415108806472,93.,-50.395358344182));
#62739=CARTESIAN_POINT('',(-18.7688932450105,93.,-54.0133224467414));
#62740=CARTESIAN_POINT('',(-16.9297772283673,93.,-49.3434280342046));
#62741=CARTESIAN_POINT('',(7.30671875642947,93.,-58.8272742891252));
#62742=CARTESIAN_POINT('',(-17.362912030776,93.,-46.4893559299515));
#62743=CARTESIAN_POINT('',(-12.3717907789054,93.,-79.3775465225558));
#62744=CARTESIAN_POINT('',(-21.8902943951393,93.,-50.1073200325109));
#62745=CARTESIAN_POINT('',(20.9391409799484,93.,-65.7672865469923));
#62746=CARTESIAN_POINT('',(23.6274073276684,93.,-66.8192168569697));
#62747=CARTESIAN_POINT('',(6.7618723018828,93.,-60.2196596729666));
#62748=CARTESIAN_POINT('',(24.0605421300771,93.,-69.6732889612228));
#62749=CARTESIAN_POINT('',(24.6799182869732,93.,-73.7545685111594));
#62750=CARTESIAN_POINT('',(21.8054105847658,93.,-71.4754307554985));
#62751=CARTESIAN_POINT('',(5.560020977711,93.,-84.4575983084442));
#62752=CARTESIAN_POINT('',(19.1171442370458,93.,-70.4235004455211));
#62753=CARTESIAN_POINT('',(4.93987555898025,93.,-64.8758735714953));
#62754=CARTESIAN_POINT('',(18.684009434637,93.,-67.569428341268));
#62755=CARTESIAN_POINT('',(19.7365203939418,93.,-74.5047799954575));
#62756=CARTESIAN_POINT('',(2.43861982758225,93.,-80.5515958942137));
#62757=CARTESIAN_POINT('',(27.9234618277415,93.,-68.5002816613462));
#62758=CARTESIAN_POINT('',(30.6117281754615,93.,-69.5522119713236));
#62759=CARTESIAN_POINT('',(6.76187230188279,93.,-60.2196596729666));
#62760=CARTESIAN_POINT('',(31.0448629778703,93.,-72.4062840755767));
#62761=CARTESIAN_POINT('',(31.1015805215427,93.,-72.7800152057398));
#62762=CARTESIAN_POINT('',(28.7897314325589,93.,-74.2084258698524));
#62763=CARTESIAN_POINT('',(9.61484001483124,93.,-89.5316442853947));
#62764=CARTESIAN_POINT('',(26.1014650848389,93.,-73.156495559875));
#62765=CARTESIAN_POINT('',(4.93987555898025,93.,-64.8758735714953));
#62766=CARTESIAN_POINT('',(25.6683302824302,93.,-70.3024234556219));
#62767=CARTESIAN_POINT('',(26.1581826285113,93.,-73.5302266900378));
#62768=CARTESIAN_POINT('',(6.4934388647025,93.,-85.6256418711642));
#62769=CARTESIAN_POINT('',(34.9077826755347,93.,-71.2332767757001));
#62770=CARTESIAN_POINT('',(37.5960490232547,93.,-72.2852070856775));
#62771=CARTESIAN_POINT('',(6.76187230188279,93.,-60.2196596729666));
#62772=CARTESIAN_POINT('',(38.0291838256634,93.,-75.1392791899306));
#62773=CARTESIAN_POINT('',(37.5232427561121,93.,-71.8054619003202));
#62774=CARTESIAN_POINT('',(35.7740522803521,93.,-76.9414209842063));
#62775=CARTESIAN_POINT('',(13.6696590519515,93.,-94.6056902623452));
#62776=CARTESIAN_POINT('',(33.085785932632,93.,-75.8894906742289));
#62777=CARTESIAN_POINT('',(4.93987555898025,93.,-64.8758735714953));
#62778=CARTESIAN_POINT('',(32.6526511302233,93.,-73.0354185699758));
#62779=CARTESIAN_POINT('',(32.5798448630807,93.,-72.5556733846182));
#62780=CARTESIAN_POINT('',(10.5482579018227,93.,-90.6996878481147));
#62781=CARTESIAN_POINT('',(41.8921035233278,93.,-73.966271890054));
#62782=CARTESIAN_POINT('',(44.5803698710478,93.,-75.0182022000314));
#62783=CARTESIAN_POINT('',(6.76187230188278,93.,-60.2196596729666));
#62784=CARTESIAN_POINT('',(45.0135046734565,93.,-77.8722743042845));
#62785=CARTESIAN_POINT('',(43.9449049906816,93.,-70.8309085949006));
#62786=CARTESIAN_POINT('',(42.7583731281452,93.,-79.6744160985602));
#62787=CARTESIAN_POINT('',(17.7244780890717,93.,-99.6797362392957));
#62788=CARTESIAN_POINT('',(40.0701067804252,93.,-78.6224857885828));
#62789=CARTESIAN_POINT('',(4.93987555898025,93.,-64.8758735714953));
#62790=CARTESIAN_POINT('',(39.6369719780164,93.,-75.7684136843297));
#62791=CARTESIAN_POINT('',(39.0015070976502,93.,-71.5811200791985));
#62792=CARTESIAN_POINT('',(14.603076938943,93.,-95.7737338250652));
#62793=CARTESIAN_POINT('',(-22.0921013332578,93.,-41.9542190213219));
#62794=CARTESIAN_POINT('',(-19.4038349855377,93.,-43.0061493312993));
#62795=CARTESIAN_POINT('',(9.12871549933204,93.,-54.1710603905964));
#62796=CARTESIAN_POINT('',(-18.970700183129,93.,-45.8602214355524));
#62797=CARTESIAN_POINT('',(-13.8500551204438,93.,-79.6018883436771));
#62798=CARTESIAN_POINT('',(-21.2258317284404,93.,-47.6623632298281));
#62799=CARTESIAN_POINT('',(-22.8237122821307,93.,-48.9392764697909));
#62800=CARTESIAN_POINT('',(-23.9140980761604,93.,-46.6104329198507));
#62801=CARTESIAN_POINT('',(7.30671875642946,93.,-58.8272742891252));
#62802=CARTESIAN_POINT('',(-24.3472328785691,93.,-43.7563608155976));
#62803=CARTESIAN_POINT('',(-18.7934530134749,93.,-80.3520998279754));
#62804=CARTESIAN_POINT('',(-25.9451134322595,93.,-45.0332740555604));
#62805=CARTESIAN_POINT('',(-29.0764221810509,93.,-39.221223906968));
#62806=CARTESIAN_POINT('',(-26.3881558333309,93.,-40.2731542169454));
#62807=CARTESIAN_POINT('',(9.12871549933204,93.,-54.1710603905964));
#62808=CARTESIAN_POINT('',(-25.9550210309222,93.,-43.1272263211986));
#62809=CARTESIAN_POINT('',(-20.2717173550133,93.,-80.5764416490967));
#62810=CARTESIAN_POINT('',(-28.2101525762335,93.,-44.9293681154742));
#62811=CARTESIAN_POINT('',(-26.878531319251,93.,-43.8652304928404));
#62812=CARTESIAN_POINT('',(-30.8984189239535,93.,-43.8774378054968));
#62813=CARTESIAN_POINT('',(7.30671875642946,93.,-58.8272742891252));
#62814=CARTESIAN_POINT('',(-31.3315537263622,93.,-41.0233657012437));
#62815=CARTESIAN_POINT('',(-25.2151152480443,93.,-81.3266531333951));
#62816=CARTESIAN_POINT('',(-29.9999324693798,93.,-39.95922807861));
#62817=CARTESIAN_POINT('',(-36.060743028844,93.,-36.4882287926142));
#62818=CARTESIAN_POINT('',(-33.372476681124,93.,-37.5401591025916));
#62819=CARTESIAN_POINT('',(9.12871549933205,93.,-54.1710603905964));
#62820=CARTESIAN_POINT('',(-32.9393418787153,93.,-40.3942312068447));
#62821=CARTESIAN_POINT('',(-26.6933795895828,93.,-81.5509949545164));
#62822=CARTESIAN_POINT('',(-35.1944734240266,93.,-42.1963730011203));
#62823=CARTESIAN_POINT('',(-30.9333503563712,93.,-38.7911845158899));
#62824=CARTESIAN_POINT('',(-37.8827397717466,93.,-41.1444426911429));
#62825=CARTESIAN_POINT('',(7.30671875642946,93.,-58.8272742891252));
#62826=CARTESIAN_POINT('',(-38.3158745741554,93.,-38.2903705868898));
#62827=CARTESIAN_POINT('',(-31.6367774826138,93.,-82.3012064388147));
#62828=CARTESIAN_POINT('',(-34.0547515065,93.,-34.8851821016595));
#62829=CARTESIAN_POINT('',(48.8764243711209,93.,-76.6992670044079));
#62830=CARTESIAN_POINT('',(51.5646907188409,93.,-77.7511973143853));
#62831=CARTESIAN_POINT('',(6.76187230188278,93.,-60.2196596729666));
#62832=CARTESIAN_POINT('',(51.9978255212496,93.,-80.6052694186384));
#62833=CARTESIAN_POINT('',(50.3665672252511,93.,-69.856355289481));
#62834=CARTESIAN_POINT('',(49.7426939759383,93.,-82.4074112129141));
#62835=CARTESIAN_POINT('',(21.779297126192,93.,-104.753782216246));
#62836=CARTESIAN_POINT('',(47.0544276282183,93.,-81.3554809029366));
#62837=CARTESIAN_POINT('',(4.93987555898025,93.,-64.8758735714953));
#62838=CARTESIAN_POINT('',(46.6212928258096,93.,-78.5014087986836));
#62839=CARTESIAN_POINT('',(45.4231693322196,93.,-70.6065667737789));
#62840=CARTESIAN_POINT('',(18.6578959760632,93.,-100.847779802016));
#62841=CARTESIAN_POINT('',(11.7041856792605,93.,-48.2040977535443));
#62842=CARTESIAN_POINT('',(14.3924520269805,93.,-49.2560280635217));
#62843=CARTESIAN_POINT('',(11.4955586967812,93.,-48.1224611082263));
#62844=CARTESIAN_POINT('',(14.8255868293893,93.,-52.1101001677748));
#62845=CARTESIAN_POINT('',(18.2582560524036,93.,-74.7291218165791));
#62846=CARTESIAN_POINT('',(12.5704552840779,93.,-53.9122419620505));
#62847=CARTESIAN_POINT('',(-6.60443613364975,93.,-69.2354603775928));
#62848=CARTESIAN_POINT('',(9.8821889363579,93.,-52.8603116520731));
#62849=CARTESIAN_POINT('',(9.67356195387869,93.,-52.7786750067551));
#62850=CARTESIAN_POINT('',(9.44905413394917,93.,-50.00623954782));
#62851=CARTESIAN_POINT('',(13.3148581593723,93.,-75.4793333008771));
#62852=CARTESIAN_POINT('',(-9.7258372837785,93.,-65.3294579633623));
#62853=CARTESIAN_POINT('',(18.6885065270537,93.,-50.9370928678982));
#62854=CARTESIAN_POINT('',(21.3767728747737,93.,-51.9890231778756));
#62855=CARTESIAN_POINT('',(11.4955586967812,93.,-48.1224611082263));
#62856=CARTESIAN_POINT('',(21.8099076771824,93.,-54.8430952821287));
#62857=CARTESIAN_POINT('',(24.679918286973,93.,-73.7545685111594));
#62858=CARTESIAN_POINT('',(19.5547761318711,93.,-56.6452370764044));
#62859=CARTESIAN_POINT('',(-2.5496170965295,93.,-74.3095063545433));
#62860=CARTESIAN_POINT('',(16.866509784151,93.,-55.593306766427));
#62861=CARTESIAN_POINT('',(9.6735619538787,93.,-52.7786750067551));
#62862=CARTESIAN_POINT('',(16.4333749817423,93.,-52.7392346621739));
#62863=CARTESIAN_POINT('',(19.7365203939418,93.,-74.5047799954575));
#62864=CARTESIAN_POINT('',(-5.67101824665825,93.,-70.4035039403128));
#62865=CARTESIAN_POINT('',(25.6728273748468,93.,-53.6700879822521));
#62866=CARTESIAN_POINT('',(28.3610937225668,93.,-54.7220182922295));
#62867=CARTESIAN_POINT('',(11.4955586967812,93.,-48.1224611082263));
#62868=CARTESIAN_POINT('',(28.7942285249755,93.,-57.5760903964826));
#62869=CARTESIAN_POINT('',(31.1015805215425,93.,-72.7800152057398));
#62870=CARTESIAN_POINT('',(26.5390969796642,93.,-59.3782321907583));
#62871=CARTESIAN_POINT('',(1.50520194059074,93.,-79.3835523314937));
#62872=CARTESIAN_POINT('',(23.8508306319442,93.,-58.3263018807808));
#62873=CARTESIAN_POINT('',(9.6735619538787,93.,-52.7786750067551));
#62874=CARTESIAN_POINT('',(23.4176958295354,93.,-55.4722297765278));
#62875=CARTESIAN_POINT('',(26.1581826285112,93.,-73.5302266900378));
#62876=CARTESIAN_POINT('',(-1.616199209538,93.,-75.4775499172633));
#62877=CARTESIAN_POINT('',(32.6571482226399,93.,-56.403083096606));
#62878=CARTESIAN_POINT('',(35.3454145703599,93.,-57.4550134065834));
#62879=CARTESIAN_POINT('',(11.4955586967812,93.,-48.1224611082264));
#62880=CARTESIAN_POINT('',(35.7785493727686,93.,-60.3090855108365));
#62881=CARTESIAN_POINT('',(37.523242756112,93.,-71.8054619003202));
#62882=CARTESIAN_POINT('',(33.5234178274573,93.,-62.1112273051122));
#62883=CARTESIAN_POINT('',(5.56002097771099,93.,-84.4575983084442));
#62884=CARTESIAN_POINT('',(30.8351514797373,93.,-61.0592969951347));
#62885=CARTESIAN_POINT('',(9.6735619538787,93.,-52.7786750067551));
#62886=CARTESIAN_POINT('',(30.4020166773286,93.,-58.2052248908817));
#62887=CARTESIAN_POINT('',(32.5798448630807,93.,-72.5556733846182));
#62888=CARTESIAN_POINT('',(2.43861982758225,93.,-80.5515958942137));
#62889=CARTESIAN_POINT('',(39.641469070433,93.,-59.1360782109599));
#62890=CARTESIAN_POINT('',(42.3297354181531,93.,-60.1880085209373));
#62891=CARTESIAN_POINT('',(11.4955586967812,93.,-48.1224611082264));
#62892=CARTESIAN_POINT('',(42.7628702205618,93.,-63.0420806251904));
#62893=CARTESIAN_POINT('',(43.9449049906815,93.,-70.8309085949006));
#62894=CARTESIAN_POINT('',(40.5077386752504,93.,-64.8442224194661));
#62895=CARTESIAN_POINT('',(9.61484001483123,93.,-89.5316442853947));
#62896=CARTESIAN_POINT('',(37.8194723275304,93.,-63.7922921094886));
#62897=CARTESIAN_POINT('',(9.6735619538787,93.,-52.7786750067551));
#62898=CARTESIAN_POINT('',(37.3863375251217,93.,-60.9382200052356));
#62899=CARTESIAN_POINT('',(39.0015070976501,93.,-71.5811200791985));
#62900=CARTESIAN_POINT('',(6.4934388647025,93.,-85.6256418711642));
#62901=CARTESIAN_POINT('',(46.6257899182262,93.,-61.8690733253138));
#62902=CARTESIAN_POINT('',(49.3140562659462,93.,-62.9210036352912));
#62903=CARTESIAN_POINT('',(11.4955586967812,93.,-48.1224611082264));
#62904=CARTESIAN_POINT('',(49.7471910683549,93.,-65.7750757395443));
#62905=CARTESIAN_POINT('',(50.366567225251,93.,-69.856355289481));
#62906=CARTESIAN_POINT('',(47.4920595230436,93.,-67.5772175338199));
#62907=CARTESIAN_POINT('',(13.6696590519515,93.,-94.6056902623451));
#62908=CARTESIAN_POINT('',(44.8037931753235,93.,-66.5252872238425));
#62909=CARTESIAN_POINT('',(9.6735619538787,93.,-52.7786750067551));
#62910=CARTESIAN_POINT('',(44.3706583729148,93.,-63.6712151195895));
#62911=CARTESIAN_POINT('',(45.4231693322196,93.,-70.6065667737789));
#62912=CARTESIAN_POINT('',(10.5482579018228,93.,-90.6996878481147));
#62913=CARTESIAN_POINT('',(-24.3427357861525,93.,-27.1240253422278));
#62914=CARTESIAN_POINT('',(-21.6544694384325,93.,-28.1759556522052));
#62915=CARTESIAN_POINT('',(13.8624018942305,93.,-42.0738618258562));
#62916=CARTESIAN_POINT('',(-21.2213346360238,93.,-31.0300277564583));
#62917=CARTESIAN_POINT('',(-13.8500551204439,93.,-79.6018883436771));
#62918=CARTESIAN_POINT('',(-23.4764661813351,93.,-32.832169550734));
#62919=CARTESIAN_POINT('',(-30.9333503563712,93.,-38.7911845158899));
#62920=CARTESIAN_POINT('',(-26.1647325290551,93.,-31.7802392407566));
#62921=CARTESIAN_POINT('',(12.0404051513279,93.,-46.730075724385));
#62922=CARTESIAN_POINT('',(-26.5978673314639,93.,-28.9261671365035));
#62923=CARTESIAN_POINT('',(-18.7934530134749,93.,-80.3520998279754));
#62924=CARTESIAN_POINT('',(-34.0547515065,93.,-34.8851821016595));
#62925=CARTESIAN_POINT('',(-17.3584149383594,93.,-29.8570204565817));
#62926=CARTESIAN_POINT('',(-14.6701485906394,93.,-30.9089507665591));
#62927=CARTESIAN_POINT('',(13.8624018942305,93.,-42.0738618258562));
#62928=CARTESIAN_POINT('',(-14.2370137882306,93.,-33.7630228708122));
#62929=CARTESIAN_POINT('',(-7.42839288587444,93.,-78.6273350382575));
#62930=CARTESIAN_POINT('',(-16.492145333542,93.,-35.5651646650879));
#62931=CARTESIAN_POINT('',(-26.878531319251,93.,-43.8652304928404));
#62932=CARTESIAN_POINT('',(-19.180411681262,93.,-34.5132343551105));
#62933=CARTESIAN_POINT('',(12.0404051513279,93.,-46.730075724385));
#62934=CARTESIAN_POINT('',(-19.6135464836707,93.,-31.6591622508574));
#62935=CARTESIAN_POINT('',(-12.3717907789055,93.,-79.3775465225558));
#62936=CARTESIAN_POINT('',(-29.9999324693798,93.,-39.95922807861));
#62937=CARTESIAN_POINT('',(40.7667862968804,93.,-66.5511750505069));
#62938=CARTESIAN_POINT('',(43.4550526446004,93.,-67.6031053604843));
#62939=CARTESIAN_POINT('',(9.12871549933199,93.,-54.1710603905965));
#62940=CARTESIAN_POINT('',(43.8881874470091,93.,-70.4571774647375));
#62941=CARTESIAN_POINT('',(43.9449049906816,93.,-70.8309085949006));
#62942=CARTESIAN_POINT('',(41.6330559016978,93.,-72.2593192590131));
#62943=CARTESIAN_POINT('',(13.6696590519515,93.,-94.6056902623452));
#62944=CARTESIAN_POINT('',(38.9447895539778,93.,-71.2073889490357));
#62945=CARTESIAN_POINT('',(7.30671875642947,93.,-58.8272742891252));
#62946=CARTESIAN_POINT('',(38.5116547515691,93.,-68.3533168447826));
#62947=CARTESIAN_POINT('',(39.0015070976502,93.,-71.5811200791985));
#62948=CARTESIAN_POINT('',(10.5482579018228,93.,-90.6996878481147));
#62949=CARTESIAN_POINT('',(47.7511071446736,93.,-69.2841701648608));
#62950=CARTESIAN_POINT('',(50.4393734923936,93.,-70.3361004748382));
#62951=CARTESIAN_POINT('',(9.12871549933199,93.,-54.1710603905965));
#62952=CARTESIAN_POINT('',(50.8725082948023,93.,-73.1901725790914));
#62953=CARTESIAN_POINT('',(50.366567225251,93.,-69.856355289481));
#62954=CARTESIAN_POINT('',(48.617376749491,93.,-74.992314373367));
#62955=CARTESIAN_POINT('',(17.7244780890717,93.,-99.6797362392957));
#62956=CARTESIAN_POINT('',(45.9291104017709,93.,-73.9403840633896));
#62957=CARTESIAN_POINT('',(7.30671875642947,93.,-58.8272742891252));
#62958=CARTESIAN_POINT('',(45.4959755993622,93.,-71.0863119591365));
#62959=CARTESIAN_POINT('',(45.4231693322196,93.,-70.6065667737789));
#62960=CARTESIAN_POINT('',(14.603076938943,93.,-95.7737338250652));
#62961=CARTESIAN_POINT('',(-30.2017394074983,93.,-31.806127067421));
#62962=CARTESIAN_POINT('',(-27.5134730597783,93.,-32.8580573773984));
#62963=CARTESIAN_POINT('',(11.4955586967813,93.,-48.1224611082263));
#62964=CARTESIAN_POINT('',(-27.0803382573695,93.,-35.7121294816515));
#62965=CARTESIAN_POINT('',(-20.2717173550133,93.,-80.5764416490967));
#62966=CARTESIAN_POINT('',(-29.3354698026809,93.,-37.5142712759272));
#62967=CARTESIAN_POINT('',(-30.9333503563712,93.,-38.7911845158899));
#62968=CARTESIAN_POINT('',(-32.0237361504009,93.,-36.4623409659497));
#62969=CARTESIAN_POINT('',(9.67356195387868,93.,-52.7786750067551));
#62970=CARTESIAN_POINT('',(-32.4568709528096,93.,-33.6082688616967));
#62971=CARTESIAN_POINT('',(-25.2151152480444,93.,-81.3266531333951));
#62972=CARTESIAN_POINT('',(-34.0547515065,93.,-34.8851821016595));
#62973=CARTESIAN_POINT('',(-23.2174185597051,93.,-34.5391221817749));
#62974=CARTESIAN_POINT('',(-20.5291522119851,93.,-35.5910524917523));
#62975=CARTESIAN_POINT('',(11.4955586967813,93.,-48.1224611082263));
#62976=CARTESIAN_POINT('',(-20.0960174095764,93.,-38.4451245960054));
#62977=CARTESIAN_POINT('',(-13.8500551204439,93.,-79.6018883436771));
#62978=CARTESIAN_POINT('',(-22.3511489548877,93.,-40.2472663902811));
#62979=CARTESIAN_POINT('',(-26.878531319251,93.,-43.8652304928404));
#62980=CARTESIAN_POINT('',(-25.0394153026078,93.,-39.1953360803036));
#62981=CARTESIAN_POINT('',(9.67356195387869,93.,-52.7786750067551));
#62982=CARTESIAN_POINT('',(-25.4725501050165,93.,-36.3412639760506));
#62983=CARTESIAN_POINT('',(-18.7934530134749,93.,-80.3520998279754));
#62984=CARTESIAN_POINT('',(-29.9999324693798,93.,-39.9592280786099));
#62985=CARTESIAN_POINT('',(-16.233097711912,93.,-37.2721172961288));
#62986=CARTESIAN_POINT('',(-13.544831364192,93.,-38.3240476061062));
#62987=CARTESIAN_POINT('',(11.4955586967812,93.,-48.1224611082263));
#62988=CARTESIAN_POINT('',(-13.1116965617833,93.,-41.1781197103593));
#62989=CARTESIAN_POINT('',(-7.42839288587437,93.,-78.6273350382575));
#62990=CARTESIAN_POINT('',(-15.3668281070946,93.,-42.9802615046349));
#62991=CARTESIAN_POINT('',(-22.8237122821307,93.,-48.9392764697909));
#62992=CARTESIAN_POINT('',(-18.0550944548146,93.,-41.9283311946575));
#62993=CARTESIAN_POINT('',(9.67356195387869,93.,-52.7786750067551));
#62994=CARTESIAN_POINT('',(-18.4882292572234,93.,-39.0742590904044));
#62995=CARTESIAN_POINT('',(-12.3717907789055,93.,-79.3775465225558));
#62996=CARTESIAN_POINT('',(-25.9451134322595,93.,-45.0332740555604));
#62997=CARTESIAN_POINT('',(-9.24877686411887,93.,-40.0051124104826));
#62998=CARTESIAN_POINT('',(-6.56051051639886,93.,-41.0570427204601));
#62999=CARTESIAN_POINT('',(11.4955586967812,93.,-48.1224611082263));
#63000=CARTESIAN_POINT('',(-6.12737571399014,93.,-43.9111148247132));
#63001=CARTESIAN_POINT('',(-1.00673065130489,93.,-77.6527817328379));
#63002=CARTESIAN_POINT('',(-8.38250725930147,93.,-45.7132566189888));
#63003=CARTESIAN_POINT('',(-18.7688932450105,93.,-54.0133224467414));
#63004=CARTESIAN_POINT('',(-11.0707736070215,93.,-44.6613263090114));
#63005=CARTESIAN_POINT('',(9.67356195387869,93.,-52.7786750067551));
#63006=CARTESIAN_POINT('',(-11.5039084094302,93.,-41.8072542047583));
#63007=CARTESIAN_POINT('',(-5.95012854433601,93.,-78.4029932171361));
#63008=CARTESIAN_POINT('',(-21.8902943951393,93.,-50.1073200325109));
#63009=CARTESIAN_POINT('',(-2.26445601632574,93.,-42.7381075248365));
#63010=CARTESIAN_POINT('',(0.423810331394273,93.,-43.7900378348139));
#63011=CARTESIAN_POINT('',(11.4955586967812,93.,-48.1224611082263));
#63012=CARTESIAN_POINT('',(0.856945133802991,93.,-46.6441099390671));
#63013=CARTESIAN_POINT('',(5.4149315832646,93.,-76.6782284274183));
#63014=CARTESIAN_POINT('',(-1.39818641150833,93.,-48.4462517333427));
#63015=CARTESIAN_POINT('',(-14.7140742078902,93.,-59.0873684236918));
#63016=CARTESIAN_POINT('',(-4.08645275922836,93.,-47.3943214233653));
#63017=CARTESIAN_POINT('',(9.67356195387869,93.,-52.7786750067551));
#63018=CARTESIAN_POINT('',(-4.51958756163709,93.,-44.5402493191122));
#63019=CARTESIAN_POINT('',(0.471533690233444,93.,-77.4284399117165));
#63020=CARTESIAN_POINT('',(-17.835475358019,93.,-55.1813660094614));
#63021=CARTESIAN_POINT('',(4.7198648314674,93.,-45.4711026391904));
#63022=CARTESIAN_POINT('',(7.40813117918741,93.,-46.5230329491678));
#63023=CARTESIAN_POINT('',(11.4955586967812,93.,-48.1224611082263));
#63024=CARTESIAN_POINT('',(7.84126598159612,93.,-49.3771050534209));
#63025=CARTESIAN_POINT('',(11.8365938178341,93.,-75.7036751219987));
#63026=CARTESIAN_POINT('',(5.5861344362848,93.,-51.1792468476966));
#63027=CARTESIAN_POINT('',(-10.65925517077,93.,-64.1614144006423));
#63028=CARTESIAN_POINT('',(2.89786808856477,93.,-50.1273165377192));
#63029=CARTESIAN_POINT('',(9.67356195387869,93.,-52.7786750067551));
#63030=CARTESIAN_POINT('',(2.46473328615604,93.,-47.2732444334661));
#63031=CARTESIAN_POINT('',(6.8931959248029,93.,-76.4538866062968));
#63032=CARTESIAN_POINT('',(-13.7806563208988,93.,-60.2554119864119));
#63033=CARTESIAN_POINT('',(-37.6508952335091,93.,-112.588303798924));
#63034=CARTESIAN_POINT('',(-34.9626288857891,93.,-113.640234108901));
#63035=CARTESIAN_POINT('',(-16.9065596726092,93.,-120.705652496668));
#63036=CARTESIAN_POINT('',(-34.5294940833804,93.,-116.494306213155));
#63037=CARTESIAN_POINT('',(-39.5367040587209,93.,-83.5001015653555));
#63038=CARTESIAN_POINT('',(-36.7846256286917,93.,-118.29644800743));
#63039=CARTESIAN_POINT('',(5.56002097771104,93.,-84.4575983084443));
#63040=CARTESIAN_POINT('',(-39.4728919764118,93.,-117.244517697453));
#63041=CARTESIAN_POINT('',(-18.728556415512,93.,-125.361866395196));
#63042=CARTESIAN_POINT('',(-39.9060267788205,93.,-114.3904455932));
#63043=CARTESIAN_POINT('',(-44.4801019517525,93.,-84.250313049654));
#63044=CARTESIAN_POINT('',(2.43861982758226,93.,-80.5515958942138));
#63045=CARTESIAN_POINT('',(-30.666574385716,93.,-115.321298913278));
#63046=CARTESIAN_POINT('',(-27.978308037996,93.,-116.373229223255));
#63047=CARTESIAN_POINT('',(-16.9065596726093,93.,-120.705652496668));
#63048=CARTESIAN_POINT('',(-27.5451732355873,93.,-119.227301327508));
#63049=CARTESIAN_POINT('',(-33.1150418241515,93.,-82.5255482599358));
#63050=CARTESIAN_POINT('',(-29.8003047808986,93.,-121.029443121784));
#63051=CARTESIAN_POINT('',(9.6148400148313,93.,-89.5316442853948));
#63052=CARTESIAN_POINT('',(-32.4885711286186,93.,-119.977512811807));
#63053=CARTESIAN_POINT('',(-18.728556415512,93.,-125.361866395196));
#63054=CARTESIAN_POINT('',(-32.9217059310274,93.,-117.123440707554));
#63055=CARTESIAN_POINT('',(-38.058439717183,93.,-83.2757597442344));
#63056=CARTESIAN_POINT('',(6.49343886470252,93.,-85.6256418711642));
#63057=CARTESIAN_POINT('Origin',(-27.978308037996,83.8,-116.373229223255));
#63058=CARTESIAN_POINT('',(-27.978308037996,83.8,-116.373229223255));
#63059=CARTESIAN_POINT('',(-27.5451732355873,83.8,-119.227301327508));
#63060=CARTESIAN_POINT('Origin',(-30.666574385716,83.8,-115.321298913278));
#63061=CARTESIAN_POINT('',(-30.666574385716,83.8,-115.321298913278));
#63062=CARTESIAN_POINT('Origin',(-32.9217059310274,83.8,-117.123440707554));
#63063=CARTESIAN_POINT('',(-32.9217059310274,83.8,-117.123440707554));
#63064=CARTESIAN_POINT('Origin',(-32.4885711286186,83.8,-119.977512811807));
#63065=CARTESIAN_POINT('',(-32.4885711286186,83.8,-119.977512811807));
#63066=CARTESIAN_POINT('Origin',(-29.8003047808986,83.8,-121.029443121784));
#63067=CARTESIAN_POINT('',(-29.8003047808986,83.8,-121.029443121784));
#63068=CARTESIAN_POINT('Origin',(-27.5451732355873,83.8,-119.227301327508));
#63069=CARTESIAN_POINT('Origin',(-34.9626288857891,83.8,-113.640234108901));
#63070=CARTESIAN_POINT('',(-34.9626288857891,83.8,-113.640234108901));
#63071=CARTESIAN_POINT('',(-34.5294940833804,83.8,-116.494306213155));
#63072=CARTESIAN_POINT('Origin',(-37.6508952335091,83.8,-112.588303798924));
#63073=CARTESIAN_POINT('',(-37.6508952335091,83.8,-112.588303798924));
#63074=CARTESIAN_POINT('Origin',(-39.9060267788205,83.8,-114.3904455932));
#63075=CARTESIAN_POINT('',(-39.9060267788205,83.8,-114.3904455932));
#63076=CARTESIAN_POINT('Origin',(-39.4728919764118,83.8,-117.244517697453));
#63077=CARTESIAN_POINT('',(-39.4728919764118,83.8,-117.244517697453));
#63078=CARTESIAN_POINT('Origin',(-36.7846256286917,83.8,-118.29644800743));
#63079=CARTESIAN_POINT('',(-36.7846256286917,83.8,-118.29644800743));
#63080=CARTESIAN_POINT('Origin',(-34.5294940833804,83.8,-116.494306213155));
#63081=CARTESIAN_POINT('Origin',(7.40813117918741,83.8,-46.5230329491678));
#63082=CARTESIAN_POINT('',(7.40813117918741,83.8,-46.5230329491678));
#63083=CARTESIAN_POINT('',(7.84126598159612,83.8,-49.3771050534209));
#63084=CARTESIAN_POINT('Origin',(4.7198648314674,83.8,-45.4711026391904));
#63085=CARTESIAN_POINT('',(4.7198648314674,83.8,-45.4711026391904));
#63086=CARTESIAN_POINT('Origin',(2.46473328615604,83.8,-47.2732444334661));
#63087=CARTESIAN_POINT('',(2.46473328615604,83.8,-47.2732444334661));
#63088=CARTESIAN_POINT('Origin',(2.89786808856477,83.8,-50.1273165377192));
#63089=CARTESIAN_POINT('',(2.89786808856477,83.8,-50.1273165377192));
#63090=CARTESIAN_POINT('Origin',(5.5861344362848,83.8,-51.1792468476966));
#63091=CARTESIAN_POINT('',(5.5861344362848,83.8,-51.1792468476966));
#63092=CARTESIAN_POINT('Origin',(7.84126598159612,83.8,-49.3771050534209));
#63093=CARTESIAN_POINT('Origin',(0.423810331394273,83.8,-43.7900378348139));
#63094=CARTESIAN_POINT('',(0.423810331394273,83.8,-43.7900378348139));
#63095=CARTESIAN_POINT('',(0.856945133802991,83.8,-46.6441099390671));
#63096=CARTESIAN_POINT('Origin',(-2.26445601632574,83.8,-42.7381075248365));
#63097=CARTESIAN_POINT('',(-2.26445601632574,83.8,-42.7381075248365));
#63098=CARTESIAN_POINT('Origin',(-4.51958756163709,83.8,-44.5402493191122));
#63099=CARTESIAN_POINT('',(-4.51958756163709,83.8,-44.5402493191122));
#63100=CARTESIAN_POINT('Origin',(-4.08645275922836,83.8,-47.3943214233653));
#63101=CARTESIAN_POINT('',(-4.08645275922836,83.8,-47.3943214233653));
#63102=CARTESIAN_POINT('Origin',(-1.39818641150833,83.8,-48.4462517333427));
#63103=CARTESIAN_POINT('',(-1.39818641150833,83.8,-48.4462517333427));
#63104=CARTESIAN_POINT('Origin',(0.856945133802991,83.8,-46.6441099390671));
#63105=CARTESIAN_POINT('Origin',(-6.56051051639886,83.8,-41.0570427204601));
#63106=CARTESIAN_POINT('',(-6.56051051639886,83.8,-41.0570427204601));
#63107=CARTESIAN_POINT('',(-6.12737571399014,83.8,-43.9111148247132));
#63108=CARTESIAN_POINT('Origin',(-9.24877686411887,83.8,-40.0051124104826));
#63109=CARTESIAN_POINT('',(-9.24877686411887,83.8,-40.0051124104826));
#63110=CARTESIAN_POINT('Origin',(-11.5039084094302,83.8,-41.8072542047583));
#63111=CARTESIAN_POINT('',(-11.5039084094302,83.8,-41.8072542047583));
#63112=CARTESIAN_POINT('Origin',(-11.0707736070215,83.8,-44.6613263090114));
#63113=CARTESIAN_POINT('',(-11.0707736070215,83.8,-44.6613263090114));
#63114=CARTESIAN_POINT('Origin',(-8.38250725930147,83.8,-45.7132566189888));
#63115=CARTESIAN_POINT('',(-8.38250725930147,83.8,-45.7132566189888));
#63116=CARTESIAN_POINT('Origin',(-6.12737571399014,83.8,-43.9111148247132));
#63117=CARTESIAN_POINT('Origin',(-13.544831364192,83.8,-38.3240476061062));
#63118=CARTESIAN_POINT('',(-13.544831364192,83.8,-38.3240476061062));
#63119=CARTESIAN_POINT('',(-13.1116965617833,83.8,-41.1781197103593));
#63120=CARTESIAN_POINT('Origin',(-16.233097711912,83.8,-37.2721172961288));
#63121=CARTESIAN_POINT('',(-16.233097711912,83.8,-37.2721172961288));
#63122=CARTESIAN_POINT('Origin',(-18.4882292572234,83.8,-39.0742590904044));
#63123=CARTESIAN_POINT('',(-18.4882292572234,83.8,-39.0742590904044));
#63124=CARTESIAN_POINT('Origin',(-18.0550944548146,83.8,-41.9283311946575));
#63125=CARTESIAN_POINT('',(-18.0550944548146,83.8,-41.9283311946575));
#63126=CARTESIAN_POINT('Origin',(-15.3668281070946,83.8,-42.9802615046349));
#63127=CARTESIAN_POINT('',(-15.3668281070946,83.8,-42.9802615046349));
#63128=CARTESIAN_POINT('Origin',(-13.1116965617833,83.8,-41.1781197103593));
#63129=CARTESIAN_POINT('Origin',(-20.5291522119851,83.8,-35.5910524917523));
#63130=CARTESIAN_POINT('',(-20.5291522119851,83.8,-35.5910524917523));
#63131=CARTESIAN_POINT('',(-20.0960174095764,83.8,-38.4451245960054));
#63132=CARTESIAN_POINT('Origin',(-23.2174185597051,83.8,-34.5391221817749));
#63133=CARTESIAN_POINT('',(-23.2174185597051,83.8,-34.5391221817749));
#63134=CARTESIAN_POINT('Origin',(-25.4725501050165,83.8,-36.3412639760506));
#63135=CARTESIAN_POINT('',(-25.4725501050165,83.8,-36.3412639760506));
#63136=CARTESIAN_POINT('Origin',(-25.0394153026078,83.8,-39.1953360803036));
#63137=CARTESIAN_POINT('',(-25.0394153026078,83.8,-39.1953360803036));
#63138=CARTESIAN_POINT('Origin',(-22.3511489548877,83.8,-40.2472663902811));
#63139=CARTESIAN_POINT('',(-22.3511489548877,83.8,-40.2472663902811));
#63140=CARTESIAN_POINT('Origin',(-20.0960174095764,83.8,-38.4451245960054));
#63141=CARTESIAN_POINT('Origin',(-27.5134730597783,83.8,-32.8580573773984));
#63142=CARTESIAN_POINT('',(-27.5134730597783,83.8,-32.8580573773984));
#63143=CARTESIAN_POINT('',(-27.0803382573695,83.8,-35.7121294816515));
#63144=CARTESIAN_POINT('Origin',(-30.2017394074983,83.8,-31.806127067421));
#63145=CARTESIAN_POINT('',(-30.2017394074983,83.8,-31.806127067421));
#63146=CARTESIAN_POINT('Origin',(-32.4568709528096,83.8,-33.6082688616967));
#63147=CARTESIAN_POINT('',(-32.4568709528096,83.8,-33.6082688616967));
#63148=CARTESIAN_POINT('Origin',(-32.0237361504009,83.8,-36.4623409659497));
#63149=CARTESIAN_POINT('',(-32.0237361504009,83.8,-36.4623409659497));
#63150=CARTESIAN_POINT('Origin',(-29.3354698026809,83.8,-37.5142712759272));
#63151=CARTESIAN_POINT('',(-29.3354698026809,83.8,-37.5142712759272));
#63152=CARTESIAN_POINT('Origin',(-27.0803382573695,83.8,-35.7121294816515));
#63153=CARTESIAN_POINT('Origin',(50.4393734923936,83.8,-70.3361004748382));
#63154=CARTESIAN_POINT('',(50.4393734923936,83.8,-70.3361004748382));
#63155=CARTESIAN_POINT('',(50.8725082948023,83.8,-73.1901725790914));
#63156=CARTESIAN_POINT('Origin',(47.7511071446736,83.8,-69.2841701648608));
#63157=CARTESIAN_POINT('',(47.7511071446736,83.8,-69.2841701648608));
#63158=CARTESIAN_POINT('Origin',(45.4959755993622,83.8,-71.0863119591365));
#63159=CARTESIAN_POINT('',(45.4959755993622,83.8,-71.0863119591365));
#63160=CARTESIAN_POINT('Origin',(45.9291104017709,83.8,-73.9403840633896));
#63161=CARTESIAN_POINT('',(45.9291104017709,83.8,-73.9403840633896));
#63162=CARTESIAN_POINT('Origin',(48.617376749491,83.8,-74.992314373367));
#63163=CARTESIAN_POINT('',(48.617376749491,83.8,-74.992314373367));
#63164=CARTESIAN_POINT('Origin',(50.8725082948023,83.8,-73.1901725790914));
#63165=CARTESIAN_POINT('Origin',(43.4550526446004,83.8,-67.6031053604843));
#63166=CARTESIAN_POINT('',(43.4550526446004,83.8,-67.6031053604843));
#63167=CARTESIAN_POINT('',(43.8881874470091,83.8,-70.4571774647375));
#63168=CARTESIAN_POINT('Origin',(40.7667862968804,83.8,-66.5511750505069));
#63169=CARTESIAN_POINT('',(40.7667862968804,83.8,-66.5511750505069));
#63170=CARTESIAN_POINT('Origin',(38.5116547515691,83.8,-68.3533168447826));
#63171=CARTESIAN_POINT('',(38.5116547515691,83.8,-68.3533168447826));
#63172=CARTESIAN_POINT('Origin',(38.9447895539778,83.8,-71.2073889490357));
#63173=CARTESIAN_POINT('',(38.9447895539778,83.8,-71.2073889490357));
#63174=CARTESIAN_POINT('Origin',(41.6330559016978,83.8,-72.2593192590131));
#63175=CARTESIAN_POINT('',(41.6330559016978,83.8,-72.2593192590131));
#63176=CARTESIAN_POINT('Origin',(43.8881874470091,83.8,-70.4571774647375));
#63177=CARTESIAN_POINT('Origin',(-14.6701485906394,83.8,-30.9089507665591));
#63178=CARTESIAN_POINT('',(-14.6701485906394,83.8,-30.9089507665591));
#63179=CARTESIAN_POINT('',(-14.2370137882306,83.8,-33.7630228708122));
#63180=CARTESIAN_POINT('Origin',(-17.3584149383594,83.8,-29.8570204565817));
#63181=CARTESIAN_POINT('',(-17.3584149383594,83.8,-29.8570204565817));
#63182=CARTESIAN_POINT('Origin',(-19.6135464836707,83.8,-31.6591622508574));
#63183=CARTESIAN_POINT('',(-19.6135464836707,83.8,-31.6591622508574));
#63184=CARTESIAN_POINT('Origin',(-19.180411681262,83.8,-34.5132343551105));
#63185=CARTESIAN_POINT('',(-19.180411681262,83.8,-34.5132343551105));
#63186=CARTESIAN_POINT('Origin',(-16.492145333542,83.8,-35.5651646650879));
#63187=CARTESIAN_POINT('',(-16.492145333542,83.8,-35.5651646650879));
#63188=CARTESIAN_POINT('Origin',(-14.2370137882306,83.8,-33.7630228708122));
#63189=CARTESIAN_POINT('Origin',(-21.6544694384325,83.8,-28.1759556522052));
#63190=CARTESIAN_POINT('',(-21.6544694384325,83.8,-28.1759556522052));
#63191=CARTESIAN_POINT('',(-21.2213346360238,83.8,-31.0300277564583));
#63192=CARTESIAN_POINT('Origin',(-24.3427357861525,83.8,-27.1240253422278));
#63193=CARTESIAN_POINT('',(-24.3427357861525,83.8,-27.1240253422278));
#63194=CARTESIAN_POINT('Origin',(-26.5978673314639,83.8,-28.9261671365035));
#63195=CARTESIAN_POINT('',(-26.5978673314639,83.8,-28.9261671365035));
#63196=CARTESIAN_POINT('Origin',(-26.1647325290551,83.8,-31.7802392407566));
#63197=CARTESIAN_POINT('',(-26.1647325290551,83.8,-31.7802392407566));
#63198=CARTESIAN_POINT('Origin',(-23.4764661813351,83.8,-32.832169550734));
#63199=CARTESIAN_POINT('',(-23.4764661813351,83.8,-32.832169550734));
#63200=CARTESIAN_POINT('Origin',(-21.2213346360238,83.8,-31.0300277564583));
#63201=CARTESIAN_POINT('Origin',(49.3140562659462,83.8,-62.9210036352912));
#63202=CARTESIAN_POINT('',(49.3140562659462,83.8,-62.9210036352912));
#63203=CARTESIAN_POINT('',(49.7471910683549,83.8,-65.7750757395443));
#63204=CARTESIAN_POINT('Origin',(46.6257899182262,83.8,-61.8690733253138));
#63205=CARTESIAN_POINT('',(46.6257899182262,83.8,-61.8690733253138));
#63206=CARTESIAN_POINT('Origin',(44.3706583729148,83.8,-63.6712151195895));
#63207=CARTESIAN_POINT('',(44.3706583729148,83.8,-63.6712151195895));
#63208=CARTESIAN_POINT('Origin',(44.8037931753235,83.8,-66.5252872238425));
#63209=CARTESIAN_POINT('',(44.8037931753235,83.8,-66.5252872238425));
#63210=CARTESIAN_POINT('Origin',(47.4920595230436,83.8,-67.5772175338199));
#63211=CARTESIAN_POINT('',(47.4920595230436,83.8,-67.5772175338199));
#63212=CARTESIAN_POINT('Origin',(49.7471910683549,83.8,-65.7750757395443));
#63213=CARTESIAN_POINT('Origin',(42.3297354181531,83.8,-60.1880085209373));
#63214=CARTESIAN_POINT('',(42.3297354181531,83.8,-60.1880085209373));
#63215=CARTESIAN_POINT('',(42.7628702205618,83.8,-63.0420806251904));
#63216=CARTESIAN_POINT('Origin',(39.641469070433,83.8,-59.1360782109599));
#63217=CARTESIAN_POINT('',(39.641469070433,83.8,-59.1360782109599));
#63218=CARTESIAN_POINT('Origin',(37.3863375251217,83.8,-60.9382200052356));
#63219=CARTESIAN_POINT('',(37.3863375251217,83.8,-60.9382200052356));
#63220=CARTESIAN_POINT('Origin',(37.8194723275304,83.8,-63.7922921094886));
#63221=CARTESIAN_POINT('',(37.8194723275304,83.8,-63.7922921094886));
#63222=CARTESIAN_POINT('Origin',(40.5077386752504,83.8,-64.844222419466));
#63223=CARTESIAN_POINT('',(40.5077386752504,83.8,-64.844222419466));
#63224=CARTESIAN_POINT('Origin',(42.7628702205618,83.8,-63.0420806251904));
#63225=CARTESIAN_POINT('Origin',(35.3454145703599,83.8,-57.4550134065834));
#63226=CARTESIAN_POINT('',(35.3454145703599,83.8,-57.4550134065834));
#63227=CARTESIAN_POINT('',(35.7785493727686,83.8,-60.3090855108365));
#63228=CARTESIAN_POINT('Origin',(32.6571482226399,83.8,-56.403083096606));
#63229=CARTESIAN_POINT('',(32.6571482226399,83.8,-56.403083096606));
#63230=CARTESIAN_POINT('Origin',(30.4020166773286,83.8,-58.2052248908817));
#63231=CARTESIAN_POINT('',(30.4020166773286,83.8,-58.2052248908817));
#63232=CARTESIAN_POINT('Origin',(30.8351514797373,83.8,-61.0592969951347));
#63233=CARTESIAN_POINT('',(30.8351514797373,83.8,-61.0592969951347));
#63234=CARTESIAN_POINT('Origin',(33.5234178274573,83.8,-62.1112273051122));
#63235=CARTESIAN_POINT('',(33.5234178274573,83.8,-62.1112273051122));
#63236=CARTESIAN_POINT('Origin',(35.7785493727686,83.8,-60.3090855108365));
#63237=CARTESIAN_POINT('Origin',(28.3610937225668,83.8,-54.7220182922295));
#63238=CARTESIAN_POINT('',(28.3610937225668,83.8,-54.7220182922295));
#63239=CARTESIAN_POINT('',(28.7942285249755,83.8,-57.5760903964826));
#63240=CARTESIAN_POINT('Origin',(25.6728273748468,83.8,-53.6700879822521));
#63241=CARTESIAN_POINT('',(25.6728273748468,83.8,-53.6700879822521));
#63242=CARTESIAN_POINT('Origin',(23.4176958295354,83.8,-55.4722297765278));
#63243=CARTESIAN_POINT('',(23.4176958295354,83.8,-55.4722297765278));
#63244=CARTESIAN_POINT('Origin',(23.8508306319442,83.8,-58.3263018807808));
#63245=CARTESIAN_POINT('',(23.8508306319442,83.8,-58.3263018807808));
#63246=CARTESIAN_POINT('Origin',(26.5390969796642,83.8,-59.3782321907583));
#63247=CARTESIAN_POINT('',(26.5390969796642,83.8,-59.3782321907583));
#63248=CARTESIAN_POINT('Origin',(28.7942285249755,83.8,-57.5760903964826));
#63249=CARTESIAN_POINT('Origin',(21.3767728747737,83.8,-51.9890231778756));
#63250=CARTESIAN_POINT('',(21.3767728747737,83.8,-51.9890231778756));
#63251=CARTESIAN_POINT('',(21.8099076771824,83.8,-54.8430952821287));
#63252=CARTESIAN_POINT('Origin',(18.6885065270537,83.8,-50.9370928678982));
#63253=CARTESIAN_POINT('',(18.6885065270537,83.8,-50.9370928678982));
#63254=CARTESIAN_POINT('Origin',(16.4333749817423,83.8,-52.7392346621739));
#63255=CARTESIAN_POINT('',(16.4333749817423,83.8,-52.7392346621739));
#63256=CARTESIAN_POINT('Origin',(16.866509784151,83.8,-55.593306766427));
#63257=CARTESIAN_POINT('',(16.866509784151,83.8,-55.593306766427));
#63258=CARTESIAN_POINT('Origin',(19.5547761318711,83.8,-56.6452370764044));
#63259=CARTESIAN_POINT('',(19.5547761318711,83.8,-56.6452370764044));
#63260=CARTESIAN_POINT('Origin',(21.8099076771824,83.8,-54.8430952821287));
#63261=CARTESIAN_POINT('Origin',(14.3924520269805,83.8,-49.2560280635217));
#63262=CARTESIAN_POINT('',(14.3924520269805,83.8,-49.2560280635217));
#63263=CARTESIAN_POINT('',(14.8255868293893,83.8,-52.1101001677748));
#63264=CARTESIAN_POINT('Origin',(11.7041856792605,83.8,-48.2040977535443));
#63265=CARTESIAN_POINT('',(11.7041856792605,83.8,-48.2040977535443));
#63266=CARTESIAN_POINT('Origin',(9.44905413394917,83.8,-50.00623954782));
#63267=CARTESIAN_POINT('',(9.44905413394917,83.8,-50.00623954782));
#63268=CARTESIAN_POINT('Origin',(9.8821889363579,83.8,-52.8603116520731));
#63269=CARTESIAN_POINT('',(9.8821889363579,83.8,-52.8603116520731));
#63270=CARTESIAN_POINT('Origin',(12.5704552840779,83.8,-53.9122419620505));
#63271=CARTESIAN_POINT('',(12.5704552840779,83.8,-53.9122419620505));
#63272=CARTESIAN_POINT('Origin',(14.8255868293893,83.8,-52.1101001677748));
#63273=CARTESIAN_POINT('Origin',(51.5646907188409,83.8,-77.7511973143853));
#63274=CARTESIAN_POINT('',(51.5646907188409,83.8,-77.7511973143853));
#63275=CARTESIAN_POINT('',(51.9978255212496,83.8,-80.6052694186384));
#63276=CARTESIAN_POINT('Origin',(48.8764243711209,83.8,-76.6992670044079));
#63277=CARTESIAN_POINT('',(48.8764243711209,83.8,-76.6992670044079));
#63278=CARTESIAN_POINT('Origin',(46.6212928258096,83.8,-78.5014087986836));
#63279=CARTESIAN_POINT('',(46.6212928258096,83.8,-78.5014087986836));
#63280=CARTESIAN_POINT('Origin',(47.0544276282183,83.8,-81.3554809029366));
#63281=CARTESIAN_POINT('',(47.0544276282183,83.8,-81.3554809029366));
#63282=CARTESIAN_POINT('Origin',(49.7426939759383,83.8,-82.4074112129141));
#63283=CARTESIAN_POINT('',(49.7426939759383,83.8,-82.4074112129141));
#63284=CARTESIAN_POINT('Origin',(51.9978255212496,83.8,-80.6052694186384));
#63285=CARTESIAN_POINT('Origin',(-33.372476681124,83.8,-37.5401591025916));
#63286=CARTESIAN_POINT('',(-33.372476681124,83.8,-37.5401591025916));
#63287=CARTESIAN_POINT('',(-32.9393418787153,83.8,-40.3942312068447));
#63288=CARTESIAN_POINT('Origin',(-36.060743028844,83.8,-36.4882287926142));
#63289=CARTESIAN_POINT('',(-36.060743028844,83.8,-36.4882287926142));
#63290=CARTESIAN_POINT('Origin',(-38.3158745741554,83.8,-38.2903705868898));
#63291=CARTESIAN_POINT('',(-38.3158745741554,83.8,-38.2903705868898));
#63292=CARTESIAN_POINT('Origin',(-37.8827397717466,83.8,-41.1444426911429));
#63293=CARTESIAN_POINT('',(-37.8827397717466,83.8,-41.1444426911429));
#63294=CARTESIAN_POINT('Origin',(-35.1944734240266,83.8,-42.1963730011203));
#63295=CARTESIAN_POINT('',(-35.1944734240266,83.8,-42.1963730011203));
#63296=CARTESIAN_POINT('Origin',(-32.9393418787153,83.8,-40.3942312068447));
#63297=CARTESIAN_POINT('Origin',(-26.3881558333309,83.8,-40.2731542169454));
#63298=CARTESIAN_POINT('',(-26.3881558333309,83.8,-40.2731542169454));
#63299=CARTESIAN_POINT('',(-25.9550210309222,83.8,-43.1272263211986));
#63300=CARTESIAN_POINT('Origin',(-29.0764221810509,83.8,-39.221223906968));
#63301=CARTESIAN_POINT('',(-29.0764221810509,83.8,-39.221223906968));
#63302=CARTESIAN_POINT('Origin',(-31.3315537263622,83.8,-41.0233657012437));
#63303=CARTESIAN_POINT('',(-31.3315537263622,83.8,-41.0233657012437));
#63304=CARTESIAN_POINT('Origin',(-30.8984189239535,83.8,-43.8774378054968));
#63305=CARTESIAN_POINT('',(-30.8984189239535,83.8,-43.8774378054968));
#63306=CARTESIAN_POINT('Origin',(-28.2101525762335,83.8,-44.9293681154742));
#63307=CARTESIAN_POINT('',(-28.2101525762335,83.8,-44.9293681154742));
#63308=CARTESIAN_POINT('Origin',(-25.9550210309222,83.8,-43.1272263211986));
#63309=CARTESIAN_POINT('Origin',(-19.4038349855377,83.8,-43.0061493312993));
#63310=CARTESIAN_POINT('',(-19.4038349855377,83.8,-43.0061493312993));
#63311=CARTESIAN_POINT('',(-18.970700183129,83.8,-45.8602214355524));
#63312=CARTESIAN_POINT('Origin',(-22.0921013332578,83.8,-41.9542190213219));
#63313=CARTESIAN_POINT('',(-22.0921013332578,83.8,-41.9542190213219));
#63314=CARTESIAN_POINT('Origin',(-24.3472328785691,83.8,-43.7563608155976));
#63315=CARTESIAN_POINT('',(-24.3472328785691,83.8,-43.7563608155976));
#63316=CARTESIAN_POINT('Origin',(-23.9140980761604,83.8,-46.6104329198507));
#63317=CARTESIAN_POINT('',(-23.9140980761604,83.8,-46.6104329198507));
#63318=CARTESIAN_POINT('Origin',(-21.2258317284404,83.8,-47.6623632298281));
#63319=CARTESIAN_POINT('',(-21.2258317284404,83.8,-47.6623632298281));
#63320=CARTESIAN_POINT('Origin',(-18.970700183129,83.8,-45.8602214355524));
#63321=CARTESIAN_POINT('Origin',(44.5803698710478,83.8,-75.0182022000314));
#63322=CARTESIAN_POINT('',(44.5803698710478,83.8,-75.0182022000314));
#63323=CARTESIAN_POINT('',(45.0135046734565,83.8,-77.8722743042845));
#63324=CARTESIAN_POINT('Origin',(41.8921035233278,83.8,-73.966271890054));
#63325=CARTESIAN_POINT('',(41.8921035233278,83.8,-73.966271890054));
#63326=CARTESIAN_POINT('Origin',(39.6369719780164,83.8,-75.7684136843297));
#63327=CARTESIAN_POINT('',(39.6369719780164,83.8,-75.7684136843297));
#63328=CARTESIAN_POINT('Origin',(40.0701067804252,83.8,-78.6224857885828));
#63329=CARTESIAN_POINT('',(40.0701067804252,83.8,-78.6224857885828));
#63330=CARTESIAN_POINT('Origin',(42.7583731281452,83.8,-79.6744160985602));
#63331=CARTESIAN_POINT('',(42.7583731281452,83.8,-79.6744160985602));
#63332=CARTESIAN_POINT('Origin',(45.0135046734565,83.8,-77.8722743042845));
#63333=CARTESIAN_POINT('Origin',(37.5960490232547,83.8,-72.2852070856775));
#63334=CARTESIAN_POINT('',(37.5960490232547,83.8,-72.2852070856775));
#63335=CARTESIAN_POINT('',(38.0291838256634,83.8,-75.1392791899306));
#63336=CARTESIAN_POINT('Origin',(34.9077826755347,83.8,-71.2332767757001));
#63337=CARTESIAN_POINT('',(34.9077826755347,83.8,-71.2332767757001));
#63338=CARTESIAN_POINT('Origin',(32.6526511302233,83.8,-73.0354185699758));
#63339=CARTESIAN_POINT('',(32.6526511302233,83.8,-73.0354185699758));
#63340=CARTESIAN_POINT('Origin',(33.085785932632,83.8,-75.8894906742289));
#63341=CARTESIAN_POINT('',(33.085785932632,83.8,-75.8894906742289));
#63342=CARTESIAN_POINT('Origin',(35.7740522803521,83.8,-76.9414209842063));
#63343=CARTESIAN_POINT('',(35.7740522803521,83.8,-76.9414209842063));
#63344=CARTESIAN_POINT('Origin',(38.0291838256634,83.8,-75.1392791899306));
#63345=CARTESIAN_POINT('Origin',(30.6117281754615,83.8,-69.5522119713236));
#63346=CARTESIAN_POINT('',(30.6117281754615,83.8,-69.5522119713236));
#63347=CARTESIAN_POINT('',(31.0448629778703,83.8,-72.4062840755767));
#63348=CARTESIAN_POINT('Origin',(27.9234618277415,83.8,-68.5002816613462));
#63349=CARTESIAN_POINT('',(27.9234618277415,83.8,-68.5002816613462));
#63350=CARTESIAN_POINT('Origin',(25.6683302824302,83.8,-70.3024234556219));
#63351=CARTESIAN_POINT('',(25.6683302824302,83.8,-70.3024234556219));
#63352=CARTESIAN_POINT('Origin',(26.1014650848389,83.8,-73.156495559875));
#63353=CARTESIAN_POINT('',(26.1014650848389,83.8,-73.156495559875));
#63354=CARTESIAN_POINT('Origin',(28.7897314325589,83.8,-74.2084258698524));
#63355=CARTESIAN_POINT('',(28.7897314325589,83.8,-74.2084258698524));
#63356=CARTESIAN_POINT('Origin',(31.0448629778703,83.8,-72.4062840755767));
#63357=CARTESIAN_POINT('Origin',(23.6274073276684,83.8,-66.8192168569697));
#63358=CARTESIAN_POINT('',(23.6274073276684,83.8,-66.8192168569697));
#63359=CARTESIAN_POINT('',(24.0605421300771,83.8,-69.6732889612228));
#63360=CARTESIAN_POINT('Origin',(20.9391409799484,83.8,-65.7672865469923));
#63361=CARTESIAN_POINT('',(20.9391409799484,83.8,-65.7672865469923));
#63362=CARTESIAN_POINT('Origin',(18.684009434637,83.8,-67.569428341268));
#63363=CARTESIAN_POINT('',(18.684009434637,83.8,-67.569428341268));
#63364=CARTESIAN_POINT('Origin',(19.1171442370458,83.8,-70.4235004455211));
#63365=CARTESIAN_POINT('',(19.1171442370458,83.8,-70.4235004455211));
#63366=CARTESIAN_POINT('Origin',(21.8054105847658,83.8,-71.4754307554985));
#63367=CARTESIAN_POINT('',(21.8054105847658,83.8,-71.4754307554985));
#63368=CARTESIAN_POINT('Origin',(24.0605421300771,83.8,-69.6732889612228));
#63369=CARTESIAN_POINT('Origin',(-12.4195141377446,83.8,-45.7391444456532));
#63370=CARTESIAN_POINT('',(-12.4195141377446,83.8,-45.7391444456532));
#63371=CARTESIAN_POINT('',(-11.9863793353359,83.8,-48.5932165499063));
#63372=CARTESIAN_POINT('Origin',(-15.1077804854646,83.8,-44.6872141356758));
#63373=CARTESIAN_POINT('',(-15.1077804854646,83.8,-44.6872141356758));
#63374=CARTESIAN_POINT('Origin',(-17.362912030776,83.8,-46.4893559299515));
#63375=CARTESIAN_POINT('',(-17.362912030776,83.8,-46.4893559299515));
#63376=CARTESIAN_POINT('Origin',(-16.9297772283673,83.8,-49.3434280342046));
#63377=CARTESIAN_POINT('',(-16.9297772283673,83.8,-49.3434280342046));
#63378=CARTESIAN_POINT('Origin',(-14.2415108806472,83.8,-50.395358344182));
#63379=CARTESIAN_POINT('',(-14.2415108806472,83.8,-50.395358344182));
#63380=CARTESIAN_POINT('Origin',(-11.9863793353359,83.8,-48.5932165499063));
#63381=CARTESIAN_POINT('Origin',(-5.43519328995148,83.8,-48.4721395600071));
#63382=CARTESIAN_POINT('',(-5.43519328995148,83.8,-48.4721395600071));
#63383=CARTESIAN_POINT('',(-5.00205848754277,83.8,-51.3262116642602));
#63384=CARTESIAN_POINT('Origin',(-8.12345963767149,83.8,-47.4202092500297));
#63385=CARTESIAN_POINT('',(-8.12345963767149,83.8,-47.4202092500297));
#63386=CARTESIAN_POINT('Origin',(-10.3785911829829,83.8,-49.2223510443054));
#63387=CARTESIAN_POINT('',(-10.3785911829829,83.8,-49.2223510443054));
#63388=CARTESIAN_POINT('Origin',(-9.94545638057412,83.8,-52.0764231485585));
#63389=CARTESIAN_POINT('',(-9.94545638057412,83.8,-52.0764231485585));
#63390=CARTESIAN_POINT('Origin',(-7.25719003285409,83.8,-53.1283534585359));
#63391=CARTESIAN_POINT('',(-7.25719003285409,83.8,-53.1283534585359));
#63392=CARTESIAN_POINT('Origin',(-5.00205848754277,83.8,-51.3262116642602));
#63393=CARTESIAN_POINT('Origin',(1.54912755784165,83.8,-51.205134674361));
#63394=CARTESIAN_POINT('',(1.54912755784165,83.8,-51.205134674361));
#63395=CARTESIAN_POINT('',(1.98226236025037,83.8,-54.0592067786141));
#63396=CARTESIAN_POINT('Origin',(-1.13913878987836,83.8,-50.1532043643836));
#63397=CARTESIAN_POINT('',(-1.13913878987836,83.8,-50.1532043643836));
#63398=CARTESIAN_POINT('Origin',(-3.39427033518972,83.8,-51.9553461586593));
#63399=CARTESIAN_POINT('',(-3.39427033518972,83.8,-51.9553461586593));
#63400=CARTESIAN_POINT('Origin',(-2.96113553278099,83.8,-54.8094182629124));
#63401=CARTESIAN_POINT('',(-2.96113553278099,83.8,-54.8094182629124));
#63402=CARTESIAN_POINT('Origin',(-0.272869185060958,83.8,-55.8613485728898));
#63403=CARTESIAN_POINT('',(-0.272869185060958,83.8,-55.8613485728898));
#63404=CARTESIAN_POINT('Origin',(1.98226236025037,83.8,-54.0592067786141));
#63405=CARTESIAN_POINT('Origin',(8.53344840563478,83.8,-53.9381297887149));
#63406=CARTESIAN_POINT('',(8.53344840563478,83.8,-53.9381297887149));
#63407=CARTESIAN_POINT('',(8.9665832080435,83.8,-56.792201892968));
#63408=CARTESIAN_POINT('Origin',(5.84518205791477,83.8,-52.8861994787375));
#63409=CARTESIAN_POINT('',(5.84518205791477,83.8,-52.8861994787375));
#63410=CARTESIAN_POINT('Origin',(3.59005051260342,83.8,-54.6883412730132));
#63411=CARTESIAN_POINT('',(3.59005051260342,83.8,-54.6883412730132));
#63412=CARTESIAN_POINT('Origin',(4.02318531501215,83.8,-57.5424133772663));
#63413=CARTESIAN_POINT('',(4.02318531501215,83.8,-57.5424133772663));
#63414=CARTESIAN_POINT('Origin',(6.71145166273218,83.8,-58.5943436872437));
#63415=CARTESIAN_POINT('',(6.71145166273218,83.8,-58.5943436872437));
#63416=CARTESIAN_POINT('Origin',(8.9665832080435,83.8,-56.792201892968));
#63417=CARTESIAN_POINT('Origin',(15.5177692534279,83.8,-56.6711249030688));
#63418=CARTESIAN_POINT('',(15.5177692534279,83.8,-56.6711249030688));
#63419=CARTESIAN_POINT('',(15.9509040558366,83.8,-59.5251970073219));
#63420=CARTESIAN_POINT('Origin',(12.8295029057079,83.8,-55.6191945930914));
#63421=CARTESIAN_POINT('',(12.8295029057079,83.8,-55.6191945930914));
#63422=CARTESIAN_POINT('Origin',(10.5743713603965,83.8,-57.4213363873671));
#63423=CARTESIAN_POINT('',(10.5743713603965,83.8,-57.4213363873671));
#63424=CARTESIAN_POINT('Origin',(11.0075061628053,83.8,-60.2754084916201));
#63425=CARTESIAN_POINT('',(11.0075061628053,83.8,-60.2754084916201));
#63426=CARTESIAN_POINT('Origin',(13.6957725105253,83.8,-61.3273388015976));
#63427=CARTESIAN_POINT('',(13.6957725105253,83.8,-61.3273388015976));
#63428=CARTESIAN_POINT('Origin',(15.9509040558366,83.8,-59.5251970073219));
#63429=CARTESIAN_POINT('Origin',(22.502090101221,83.8,-59.4041200174227));
#63430=CARTESIAN_POINT('',(22.502090101221,83.8,-59.4041200174227));
#63431=CARTESIAN_POINT('',(22.9352249036298,83.8,-62.2581921216758));
#63432=CARTESIAN_POINT('Origin',(19.813823753501,83.8,-58.3521897074453));
#63433=CARTESIAN_POINT('',(19.813823753501,83.8,-58.3521897074453));
#63434=CARTESIAN_POINT('Origin',(17.5586922081897,83.8,-60.154331501721));
#63435=CARTESIAN_POINT('',(17.5586922081897,83.8,-60.154331501721));
#63436=CARTESIAN_POINT('Origin',(17.9918270105984,83.8,-63.008403605974));
#63437=CARTESIAN_POINT('',(17.9918270105984,83.8,-63.008403605974));
#63438=CARTESIAN_POINT('Origin',(20.6800933583184,83.8,-64.0603339159514));
#63439=CARTESIAN_POINT('',(20.6800933583184,83.8,-64.0603339159514));
#63440=CARTESIAN_POINT('Origin',(22.9352249036298,83.8,-62.2581921216758));
#63441=CARTESIAN_POINT('Origin',(29.4864109490142,83.8,-62.1371151317766));
#63442=CARTESIAN_POINT('',(29.4864109490142,83.8,-62.1371151317766));
#63443=CARTESIAN_POINT('',(29.9195457514229,83.8,-64.9911872360297));
#63444=CARTESIAN_POINT('Origin',(26.7981446012942,83.8,-61.0851848217992));
#63445=CARTESIAN_POINT('',(26.7981446012942,83.8,-61.0851848217992));
#63446=CARTESIAN_POINT('Origin',(24.5430130559828,83.8,-62.8873266160749));
#63447=CARTESIAN_POINT('',(24.5430130559828,83.8,-62.8873266160749));
#63448=CARTESIAN_POINT('Origin',(24.9761478583915,83.8,-65.7413987203279));
#63449=CARTESIAN_POINT('',(24.9761478583915,83.8,-65.7413987203279));
#63450=CARTESIAN_POINT('Origin',(27.6644142061116,83.8,-66.7933290303053));
#63451=CARTESIAN_POINT('',(27.6644142061116,83.8,-66.7933290303053));
#63452=CARTESIAN_POINT('Origin',(29.9195457514229,83.8,-64.9911872360297));
#63453=CARTESIAN_POINT('Origin',(36.4707317968073,83.8,-64.8701102461305));
#63454=CARTESIAN_POINT('',(36.4707317968073,83.8,-64.8701102461305));
#63455=CARTESIAN_POINT('',(36.903866599216,83.8,-67.7241823503836));
#63456=CARTESIAN_POINT('Origin',(33.7824654490873,83.8,-63.818179936153));
#63457=CARTESIAN_POINT('',(33.7824654490873,83.8,-63.818179936153));
#63458=CARTESIAN_POINT('Origin',(31.5273339037759,83.8,-65.6203217304287));
#63459=CARTESIAN_POINT('',(31.5273339037759,83.8,-65.6203217304287));
#63460=CARTESIAN_POINT('Origin',(31.9604687061847,83.8,-68.4743938346818));
#63461=CARTESIAN_POINT('',(31.9604687061847,83.8,-68.4743938346818));
#63462=CARTESIAN_POINT('Origin',(34.6487350539047,83.8,-69.5263241446592));
#63463=CARTESIAN_POINT('',(34.6487350539047,83.8,-69.5263241446592));
#63464=CARTESIAN_POINT('Origin',(36.903866599216,83.8,-67.7241823503836));
#63465=CARTESIAN_POINT('Origin',(40.0791009652583,83.8,-45.3578148418432));
#63466=CARTESIAN_POINT('',(40.0791009652583,83.8,-45.3578148418432));
#63467=CARTESIAN_POINT('',(40.512235767667,83.8,-48.2118869460963));
#63468=CARTESIAN_POINT('Origin',(37.3908346175383,83.8,-44.3058845318658));
#63469=CARTESIAN_POINT('',(37.3908346175383,83.8,-44.3058845318658));
#63470=CARTESIAN_POINT('Origin',(35.1357030722269,83.8,-46.1080263261415));
#63471=CARTESIAN_POINT('',(35.1357030722269,83.8,-46.1080263261415));
#63472=CARTESIAN_POINT('Origin',(35.5688378746357,83.8,-48.9620984303945));
#63473=CARTESIAN_POINT('',(35.5688378746357,83.8,-48.9620984303945));
#63474=CARTESIAN_POINT('Origin',(38.2571042223557,83.8,-50.014028740372));
#63475=CARTESIAN_POINT('',(38.2571042223557,83.8,-50.014028740372));
#63476=CARTESIAN_POINT('Origin',(40.512235767667,83.8,-48.2118869460963));
#63477=CARTESIAN_POINT('Origin',(47.0634218130514,83.8,-48.0908099561971));
#63478=CARTESIAN_POINT('',(47.0634218130514,83.8,-48.0908099561971));
#63479=CARTESIAN_POINT('',(47.4965566154602,83.8,-50.9448820604502));
#63480=CARTESIAN_POINT('Origin',(44.3751554653314,83.8,-47.0388796462197));
#63481=CARTESIAN_POINT('',(44.3751554653314,83.8,-47.0388796462197));
#63482=CARTESIAN_POINT('Origin',(42.1200239200201,83.8,-48.8410214404954));
#63483=CARTESIAN_POINT('',(42.1200239200201,83.8,-48.8410214404954));
#63484=CARTESIAN_POINT('Origin',(42.5531587224288,83.8,-51.6950935447484));
#63485=CARTESIAN_POINT('',(42.5531587224288,83.8,-51.6950935447484));
#63486=CARTESIAN_POINT('Origin',(45.2414250701488,83.8,-52.7470238547258));
#63487=CARTESIAN_POINT('',(45.2414250701488,83.8,-52.7470238547258));
#63488=CARTESIAN_POINT('Origin',(47.4965566154602,83.8,-50.9448820604502));
#63489=CARTESIAN_POINT('Origin',(4.03217949984528,83.8,-24.2777424305267));
#63490=CARTESIAN_POINT('',(4.03217949984528,83.8,-24.2777424305267));
#63491=CARTESIAN_POINT('',(4.465314302254,83.8,-27.1318145347798));
#63492=CARTESIAN_POINT('Origin',(1.34391315212527,83.8,-23.2258121205493));
#63493=CARTESIAN_POINT('',(1.34391315212527,83.8,-23.2258121205493));
#63494=CARTESIAN_POINT('Origin',(-0.911218393186086,83.8,-25.0279539148249));
#63495=CARTESIAN_POINT('',(-0.911218393186086,83.8,-25.0279539148249));
#63496=CARTESIAN_POINT('Origin',(-0.478083590777355,83.8,-27.882026019078));
#63497=CARTESIAN_POINT('',(-0.478083590777355,83.8,-27.882026019078));
#63498=CARTESIAN_POINT('Origin',(2.21018275694267,83.8,-28.9339563290554));
#63499=CARTESIAN_POINT('',(2.21018275694267,83.8,-28.9339563290554));
#63500=CARTESIAN_POINT('Origin',(4.465314302254,83.8,-27.1318145347798));
#63501=CARTESIAN_POINT('Origin',(11.0165003476384,83.8,-27.0107375448806));
#63502=CARTESIAN_POINT('',(11.0165003476384,83.8,-27.0107375448806));
#63503=CARTESIAN_POINT('',(11.4496351500471,83.8,-29.8648096491337));
#63504=CARTESIAN_POINT('Origin',(8.3282339999184,83.8,-25.9588072349031));
#63505=CARTESIAN_POINT('',(8.3282339999184,83.8,-25.9588072349031));
#63506=CARTESIAN_POINT('Origin',(6.07310245460704,83.8,-27.7609490291788));
#63507=CARTESIAN_POINT('',(6.07310245460704,83.8,-27.7609490291788));
#63508=CARTESIAN_POINT('Origin',(6.50623725701577,83.8,-30.6150211334319));
#63509=CARTESIAN_POINT('',(6.50623725701577,83.8,-30.6150211334319));
#63510=CARTESIAN_POINT('Origin',(9.1945036047358,83.8,-31.6669514434093));
#63511=CARTESIAN_POINT('',(9.1945036047358,83.8,-31.6669514434093));
#63512=CARTESIAN_POINT('Origin',(11.4496351500471,83.8,-29.8648096491337));
#63513=CARTESIAN_POINT('Origin',(18.0008211954315,83.8,-29.7437326592344));
#63514=CARTESIAN_POINT('',(18.0008211954315,83.8,-29.7437326592344));
#63515=CARTESIAN_POINT('',(18.4339559978403,83.8,-32.5978047634875));
#63516=CARTESIAN_POINT('Origin',(15.3125548477115,83.8,-28.691802349257));
#63517=CARTESIAN_POINT('',(15.3125548477115,83.8,-28.691802349257));
#63518=CARTESIAN_POINT('Origin',(13.0574233024002,83.8,-30.4939441435327));
#63519=CARTESIAN_POINT('',(13.0574233024002,83.8,-30.4939441435327));
#63520=CARTESIAN_POINT('Origin',(13.4905581048089,83.8,-33.3480162477858));
#63521=CARTESIAN_POINT('',(13.4905581048089,83.8,-33.3480162477858));
#63522=CARTESIAN_POINT('Origin',(16.1788244525289,83.8,-34.3999465577632));
#63523=CARTESIAN_POINT('',(16.1788244525289,83.8,-34.3999465577632));
#63524=CARTESIAN_POINT('Origin',(18.4339559978403,83.8,-32.5978047634875));
#63525=CARTESIAN_POINT('Origin',(24.9851420432247,83.8,-32.4767277735883));
#63526=CARTESIAN_POINT('',(24.9851420432247,83.8,-32.4767277735883));
#63527=CARTESIAN_POINT('',(25.4182768456334,83.8,-35.3307998778414));
#63528=CARTESIAN_POINT('Origin',(22.2968756955047,83.8,-31.4247974636109));
#63529=CARTESIAN_POINT('',(22.2968756955047,83.8,-31.4247974636109));
#63530=CARTESIAN_POINT('Origin',(20.0417441501933,83.8,-33.2269392578866));
#63531=CARTESIAN_POINT('',(20.0417441501933,83.8,-33.2269392578866));
#63532=CARTESIAN_POINT('Origin',(20.474878952602,83.8,-36.0810113621397));
#63533=CARTESIAN_POINT('',(20.474878952602,83.8,-36.0810113621397));
#63534=CARTESIAN_POINT('Origin',(23.1631453003221,83.8,-37.1329416721171));
#63535=CARTESIAN_POINT('',(23.1631453003221,83.8,-37.1329416721171));
#63536=CARTESIAN_POINT('Origin',(25.4182768456334,83.8,-35.3307998778414));
#63537=CARTESIAN_POINT('Origin',(31.9694628910178,83.8,-35.2097228879422));
#63538=CARTESIAN_POINT('',(31.9694628910178,83.8,-35.2097228879422));
#63539=CARTESIAN_POINT('',(32.4025976934265,83.8,-38.0637949921953));
#63540=CARTESIAN_POINT('Origin',(29.2811965432978,83.8,-34.1577925779648));
#63541=CARTESIAN_POINT('',(29.2811965432978,83.8,-34.1577925779648));
#63542=CARTESIAN_POINT('Origin',(27.0260649979864,83.8,-35.9599343722405));
#63543=CARTESIAN_POINT('',(27.0260649979864,83.8,-35.9599343722405));
#63544=CARTESIAN_POINT('Origin',(27.4591998003952,83.8,-38.8140064764936));
#63545=CARTESIAN_POINT('',(27.4591998003952,83.8,-38.8140064764936));
#63546=CARTESIAN_POINT('Origin',(30.1474661481152,83.8,-39.865936786471));
#63547=CARTESIAN_POINT('',(30.1474661481152,83.8,-39.865936786471));
#63548=CARTESIAN_POINT('Origin',(32.4025976934265,83.8,-38.0637949921953));
#63549=CARTESIAN_POINT('Origin',(38.9537837388109,83.8,-37.9427180022961));
#63550=CARTESIAN_POINT('',(38.9537837388109,83.8,-37.9427180022961));
#63551=CARTESIAN_POINT('',(39.3869185412196,83.8,-40.7967901065492));
#63552=CARTESIAN_POINT('Origin',(36.2655173910909,83.8,-36.8907876923187));
#63553=CARTESIAN_POINT('',(36.2655173910909,83.8,-36.8907876923187));
#63554=CARTESIAN_POINT('Origin',(34.0103858457796,83.8,-38.6929294865944));
#63555=CARTESIAN_POINT('',(34.0103858457796,83.8,-38.6929294865944));
#63556=CARTESIAN_POINT('Origin',(34.4435206481883,83.8,-41.5470015908475));
#63557=CARTESIAN_POINT('',(34.4435206481883,83.8,-41.5470015908475));
#63558=CARTESIAN_POINT('Origin',(37.1317869959083,83.8,-42.5989319008249));
#63559=CARTESIAN_POINT('',(37.1317869959083,83.8,-42.5989319008249));
#63560=CARTESIAN_POINT('Origin',(39.3869185412196,83.8,-40.7967901065492));
#63561=CARTESIAN_POINT('Origin',(-7.68582774284623,83.8,-33.641945880913));
#63562=CARTESIAN_POINT('',(-7.68582774284623,83.8,-33.641945880913));
#63563=CARTESIAN_POINT('',(-7.25269294043752,83.8,-36.4960179851661));
#63564=CARTESIAN_POINT('Origin',(-10.3740940905662,83.8,-32.5900155709356));
#63565=CARTESIAN_POINT('',(-10.3740940905662,83.8,-32.5900155709356));
#63566=CARTESIAN_POINT('Origin',(-12.6292256358776,83.8,-34.3921573652113));
#63567=CARTESIAN_POINT('',(-12.6292256358776,83.8,-34.3921573652113));
#63568=CARTESIAN_POINT('Origin',(-12.1960908334689,83.8,-37.2462294694643));
#63569=CARTESIAN_POINT('',(-12.1960908334689,83.8,-37.2462294694643));
#63570=CARTESIAN_POINT('Origin',(-9.50782448574884,83.8,-38.2981597794418));
#63571=CARTESIAN_POINT('',(-9.50782448574884,83.8,-38.2981597794418));
#63572=CARTESIAN_POINT('Origin',(-7.25269294043752,83.8,-36.4960179851661));
#63573=CARTESIAN_POINT('Origin',(-0.701506895053102,83.8,-36.3749409952669));
#63574=CARTESIAN_POINT('',(-0.701506895053102,83.8,-36.3749409952669));
#63575=CARTESIAN_POINT('',(-0.268372092644385,83.8,-39.22901309952));
#63576=CARTESIAN_POINT('Origin',(-3.38977324277311,83.8,-35.3230106852895));
#63577=CARTESIAN_POINT('',(-3.38977324277311,83.8,-35.3230106852895));
#63578=CARTESIAN_POINT('Origin',(-5.64490478808447,83.8,-37.1251524795652));
#63579=CARTESIAN_POINT('',(-5.64490478808447,83.8,-37.1251524795652));
#63580=CARTESIAN_POINT('Origin',(-5.21176998567574,83.8,-39.9792245838182));
#63581=CARTESIAN_POINT('',(-5.21176998567574,83.8,-39.9792245838182));
#63582=CARTESIAN_POINT('Origin',(-2.52350363795571,83.8,-41.0311548937957));
#63583=CARTESIAN_POINT('',(-2.52350363795571,83.8,-41.0311548937957));
#63584=CARTESIAN_POINT('Origin',(-0.268372092644385,83.8,-39.22901309952));
#63585=CARTESIAN_POINT('Origin',(6.28281395274003,83.8,-39.1079361096208));
#63586=CARTESIAN_POINT('',(6.28281395274003,83.8,-39.1079361096208));
#63587=CARTESIAN_POINT('',(6.71594875514875,83.8,-41.9620082138739));
#63588=CARTESIAN_POINT('Origin',(3.59454760502002,83.8,-38.0560057996434));
#63589=CARTESIAN_POINT('',(3.59454760502002,83.8,-38.0560057996434));
#63590=CARTESIAN_POINT('Origin',(1.33941605970866,83.8,-39.8581475939191));
#63591=CARTESIAN_POINT('',(1.33941605970866,83.8,-39.8581475939191));
#63592=CARTESIAN_POINT('Origin',(1.7725508621174,83.8,-42.7122196981721));
#63593=CARTESIAN_POINT('',(1.7725508621174,83.8,-42.7122196981721));
#63594=CARTESIAN_POINT('Origin',(4.46081720983742,83.8,-43.7641500081495));
#63595=CARTESIAN_POINT('',(4.46081720983742,83.8,-43.7641500081495));
#63596=CARTESIAN_POINT('Origin',(6.71594875514875,83.8,-41.9620082138739));
#63597=CARTESIAN_POINT('Origin',(13.2671348005332,83.8,-41.8409312239747));
#63598=CARTESIAN_POINT('',(13.2671348005332,83.8,-41.8409312239747));
#63599=CARTESIAN_POINT('',(13.7002696029419,83.8,-44.6950033282278));
#63600=CARTESIAN_POINT('Origin',(10.5788684528132,83.8,-40.7890009139973));
#63601=CARTESIAN_POINT('',(10.5788684528132,83.8,-40.7890009139973));
#63602=CARTESIAN_POINT('Origin',(8.32373690750179,83.8,-42.591142708273));
#63603=CARTESIAN_POINT('',(8.32373690750179,83.8,-42.591142708273));
#63604=CARTESIAN_POINT('Origin',(8.75687170991053,83.8,-45.445214812526));
#63605=CARTESIAN_POINT('',(8.75687170991053,83.8,-45.445214812526));
#63606=CARTESIAN_POINT('Origin',(11.4451380576306,83.8,-46.4971451225034));
#63607=CARTESIAN_POINT('',(11.4451380576306,83.8,-46.4971451225034));
#63608=CARTESIAN_POINT('Origin',(13.7002696029419,83.8,-44.6950033282278));
#63609=CARTESIAN_POINT('Origin',(20.2514556483263,83.8,-44.5739263383286));
#63610=CARTESIAN_POINT('',(20.2514556483263,83.8,-44.5739263383286));
#63611=CARTESIAN_POINT('',(20.684590450735,83.8,-47.4279984425817));
#63612=CARTESIAN_POINT('Origin',(17.5631893006063,83.8,-43.5219960283511));
#63613=CARTESIAN_POINT('',(17.5631893006063,83.8,-43.5219960283511));
#63614=CARTESIAN_POINT('Origin',(15.3080577552949,83.8,-45.3241378226269));
#63615=CARTESIAN_POINT('',(15.3080577552949,83.8,-45.3241378226269));
#63616=CARTESIAN_POINT('Origin',(15.7411925577037,83.8,-48.1782099268799));
#63617=CARTESIAN_POINT('',(15.7411925577037,83.8,-48.1782099268799));
#63618=CARTESIAN_POINT('Origin',(18.4294589054237,83.8,-49.2301402368573));
#63619=CARTESIAN_POINT('',(18.4294589054237,83.8,-49.2301402368573));
#63620=CARTESIAN_POINT('Origin',(20.684590450735,83.8,-47.4279984425817));
#63621=CARTESIAN_POINT('Origin',(27.2357764961194,83.8,-47.3069214526824));
#63622=CARTESIAN_POINT('',(27.2357764961194,83.8,-47.3069214526824));
#63623=CARTESIAN_POINT('',(27.6689112985281,83.8,-50.1609935569356));
#63624=CARTESIAN_POINT('Origin',(24.5475101483994,83.8,-46.254991142705));
#63625=CARTESIAN_POINT('',(24.5475101483994,83.8,-46.254991142705));
#63626=CARTESIAN_POINT('Origin',(22.2923786030881,83.8,-48.0571329369807));
#63627=CARTESIAN_POINT('',(22.2923786030881,83.8,-48.0571329369807));
#63628=CARTESIAN_POINT('Origin',(22.7255134054968,83.8,-50.9112050412338));
#63629=CARTESIAN_POINT('',(22.7255134054968,83.8,-50.9112050412338));
#63630=CARTESIAN_POINT('Origin',(25.4137797532168,83.8,-51.9631353512112));
#63631=CARTESIAN_POINT('',(25.4137797532168,83.8,-51.9631353512112));
#63632=CARTESIAN_POINT('Origin',(27.6689112985281,83.8,-50.1609935569356));
#63633=CARTESIAN_POINT('Origin',(34.2200973439125,83.8,-50.0399165670363));
#63634=CARTESIAN_POINT('',(34.2200973439125,83.8,-50.0399165670363));
#63635=CARTESIAN_POINT('',(34.6532321463213,83.8,-52.8939886712894));
#63636=CARTESIAN_POINT('Origin',(31.5318309961925,83.8,-48.9879862570589));
#63637=CARTESIAN_POINT('',(31.5318309961925,83.8,-48.9879862570589));
#63638=CARTESIAN_POINT('Origin',(29.2766994508812,83.8,-50.7901280513346));
#63639=CARTESIAN_POINT('',(29.2766994508812,83.8,-50.7901280513346));
#63640=CARTESIAN_POINT('Origin',(29.7098342532899,83.8,-53.6442001555877));
#63641=CARTESIAN_POINT('',(29.7098342532899,83.8,-53.6442001555877));
#63642=CARTESIAN_POINT('Origin',(32.3981006010099,83.8,-54.6961304655651));
#63643=CARTESIAN_POINT('',(32.3981006010099,83.8,-54.6961304655651));
#63644=CARTESIAN_POINT('Origin',(34.6532321463213,83.8,-52.8939886712894));
#63645=CARTESIAN_POINT('Origin',(41.2044181917057,83.8,-52.7729116813902));
#63646=CARTESIAN_POINT('',(41.2044181917057,83.8,-52.7729116813902));
#63647=CARTESIAN_POINT('',(41.6375529941144,83.8,-55.6269837856433));
#63648=CARTESIAN_POINT('Origin',(38.5161518439857,83.8,-51.7209813714128));
#63649=CARTESIAN_POINT('',(38.5161518439857,83.8,-51.7209813714128));
#63650=CARTESIAN_POINT('Origin',(36.2610202986743,83.8,-53.5231231656885));
#63651=CARTESIAN_POINT('',(36.2610202986743,83.8,-53.5231231656885));
#63652=CARTESIAN_POINT('Origin',(36.694155101083,83.8,-56.3771952699416));
#63653=CARTESIAN_POINT('',(36.694155101083,83.8,-56.3771952699416));
#63654=CARTESIAN_POINT('Origin',(39.3824214488031,83.8,-57.429125579919));
#63655=CARTESIAN_POINT('',(39.3824214488031,83.8,-57.429125579919));
#63656=CARTESIAN_POINT('Origin',(41.6375529941144,83.8,-55.6269837856433));
#63657=CARTESIAN_POINT('Origin',(33.0947801174652,83.8,-42.6248197274893));
#63658=CARTESIAN_POINT('',(33.0947801174652,83.8,-42.6248197274893));
#63659=CARTESIAN_POINT('',(33.5279149198739,83.8,-45.4788918317424));
#63660=CARTESIAN_POINT('Origin',(30.4065137697452,83.8,-41.5728894175119));
#63661=CARTESIAN_POINT('',(30.4065137697452,83.8,-41.5728894175119));
#63662=CARTESIAN_POINT('Origin',(28.1513822244338,83.8,-43.3750312117876));
#63663=CARTESIAN_POINT('',(28.1513822244338,83.8,-43.3750312117876));
#63664=CARTESIAN_POINT('Origin',(28.5845170268425,83.8,-46.2291033160406));
#63665=CARTESIAN_POINT('',(28.5845170268425,83.8,-46.2291033160406));
#63666=CARTESIAN_POINT('Origin',(31.2727833745626,83.8,-47.2810336260181));
#63667=CARTESIAN_POINT('',(31.2727833745626,83.8,-47.2810336260181));
#63668=CARTESIAN_POINT('Origin',(33.5279149198739,83.8,-45.4788918317424));
#63669=CARTESIAN_POINT('Origin',(26.110459269672,83.8,-39.8918246131354));
#63670=CARTESIAN_POINT('',(26.110459269672,83.8,-39.8918246131354));
#63671=CARTESIAN_POINT('',(26.5435940720808,83.8,-42.7458967173885));
#63672=CARTESIAN_POINT('Origin',(23.422192921952,83.8,-38.839894303158));
#63673=CARTESIAN_POINT('',(23.422192921952,83.8,-38.839894303158));
#63674=CARTESIAN_POINT('Origin',(21.1670613766407,83.8,-40.6420360974337));
#63675=CARTESIAN_POINT('',(21.1670613766407,83.8,-40.6420360974337));
#63676=CARTESIAN_POINT('Origin',(21.6001961790494,83.8,-43.4961082016867));
#63677=CARTESIAN_POINT('',(21.6001961790494,83.8,-43.4961082016867));
#63678=CARTESIAN_POINT('Origin',(24.2884625267694,83.8,-44.5480385116642));
#63679=CARTESIAN_POINT('',(24.2884625267694,83.8,-44.5480385116642));
#63680=CARTESIAN_POINT('Origin',(26.5435940720808,83.8,-42.7458967173885));
#63681=CARTESIAN_POINT('Origin',(19.1261384218789,83.8,-37.1588294987815));
#63682=CARTESIAN_POINT('',(19.1261384218789,83.8,-37.1588294987815));
#63683=CARTESIAN_POINT('',(19.5592732242876,83.8,-40.0129016030346));
#63684=CARTESIAN_POINT('Origin',(16.4378720741589,83.8,-36.1068991888041));
#63685=CARTESIAN_POINT('',(16.4378720741589,83.8,-36.1068991888041));
#63686=CARTESIAN_POINT('Origin',(14.1827405288475,83.8,-37.9090409830798));
#63687=CARTESIAN_POINT('',(14.1827405288475,83.8,-37.9090409830798));
#63688=CARTESIAN_POINT('Origin',(14.6158753312563,83.8,-40.7631130873329));
#63689=CARTESIAN_POINT('',(14.6158753312563,83.8,-40.7631130873329));
#63690=CARTESIAN_POINT('Origin',(17.3041416789763,83.8,-41.8150433973103));
#63691=CARTESIAN_POINT('',(17.3041416789763,83.8,-41.8150433973103));
#63692=CARTESIAN_POINT('Origin',(19.5592732242876,83.8,-40.0129016030346));
#63693=CARTESIAN_POINT('Origin',(12.1418175740858,83.8,-34.4258343844276));
#63694=CARTESIAN_POINT('',(12.1418175740858,83.8,-34.4258343844276));
#63695=CARTESIAN_POINT('',(12.5749523764945,83.8,-37.2799064886807));
#63696=CARTESIAN_POINT('Origin',(9.45355122636578,83.8,-33.3739040744502));
#63697=CARTESIAN_POINT('',(9.45355122636578,83.8,-33.3739040744502));
#63698=CARTESIAN_POINT('Origin',(7.19841968105442,83.8,-35.1760458687259));
#63699=CARTESIAN_POINT('',(7.19841968105442,83.8,-35.1760458687259));
#63700=CARTESIAN_POINT('Origin',(7.63155448346315,83.8,-38.030117972979));
#63701=CARTESIAN_POINT('',(7.63155448346315,83.8,-38.030117972979));
#63702=CARTESIAN_POINT('Origin',(10.3198208311832,83.8,-39.0820482829564));
#63703=CARTESIAN_POINT('',(10.3198208311832,83.8,-39.0820482829564));
#63704=CARTESIAN_POINT('Origin',(12.5749523764945,83.8,-37.2799064886807));
#63705=CARTESIAN_POINT('Origin',(48.1887390394988,83.8,-55.5059067957441));
#63706=CARTESIAN_POINT('',(48.1887390394988,83.8,-55.5059067957441));
#63707=CARTESIAN_POINT('',(48.6218738419075,83.8,-58.3599788999972));
#63708=CARTESIAN_POINT('Origin',(45.5004726917788,83.8,-54.4539764857667));
#63709=CARTESIAN_POINT('',(45.5004726917788,83.8,-54.4539764857667));
#63710=CARTESIAN_POINT('Origin',(43.2453411464674,83.8,-56.2561182800424));
#63711=CARTESIAN_POINT('',(43.2453411464674,83.8,-56.2561182800424));
#63712=CARTESIAN_POINT('Origin',(43.6784759488762,83.8,-59.1101903842955));
#63713=CARTESIAN_POINT('',(43.6784759488762,83.8,-59.1101903842955));
#63714=CARTESIAN_POINT('Origin',(46.3667422965962,83.8,-60.1621206942729));
#63715=CARTESIAN_POINT('',(46.3667422965962,83.8,-60.1621206942729));
#63716=CARTESIAN_POINT('Origin',(48.6218738419075,83.8,-58.3599788999972));
#63717=CARTESIAN_POINT('Origin',(-8.81114496929361,83.8,-26.2268490413659));
#63718=CARTESIAN_POINT('',(-8.81114496929361,83.8,-26.2268490413659));
#63719=CARTESIAN_POINT('',(-8.37801016688489,83.8,-29.080921145619));
#63720=CARTESIAN_POINT('Origin',(-11.4994113170136,83.8,-25.1749187313885));
#63721=CARTESIAN_POINT('',(-11.4994113170136,83.8,-25.1749187313885));
#63722=CARTESIAN_POINT('Origin',(-13.754542862325,83.8,-26.9770605256642));
#63723=CARTESIAN_POINT('',(-13.754542862325,83.8,-26.9770605256642));
#63724=CARTESIAN_POINT('Origin',(-13.3214080599162,83.8,-29.8311326299173));
#63725=CARTESIAN_POINT('',(-13.3214080599162,83.8,-29.8311326299173));
#63726=CARTESIAN_POINT('Origin',(-10.6331417121962,83.8,-30.8830629398947));
#63727=CARTESIAN_POINT('',(-10.6331417121962,83.8,-30.8830629398947));
#63728=CARTESIAN_POINT('Origin',(-8.37801016688489,83.8,-29.080921145619));
#63729=CARTESIAN_POINT('Origin',(-1.82682412150048,83.8,-28.9598441557198));
#63730=CARTESIAN_POINT('',(-1.82682412150048,83.8,-28.9598441557198));
#63731=CARTESIAN_POINT('',(-1.39368931909176,83.8,-31.8139162599729));
#63732=CARTESIAN_POINT('Origin',(-4.51509046922049,83.8,-27.9079138457424));
#63733=CARTESIAN_POINT('',(-4.51509046922049,83.8,-27.9079138457424));
#63734=CARTESIAN_POINT('Origin',(-6.77022201453184,83.8,-29.7100556400181));
#63735=CARTESIAN_POINT('',(-6.77022201453184,83.8,-29.7100556400181));
#63736=CARTESIAN_POINT('Origin',(-6.33708721212311,83.8,-32.5641277442712));
#63737=CARTESIAN_POINT('',(-6.33708721212311,83.8,-32.5641277442712));
#63738=CARTESIAN_POINT('Origin',(-3.64882086440308,83.8,-33.6160580542486));
#63739=CARTESIAN_POINT('',(-3.64882086440308,83.8,-33.6160580542486));
#63740=CARTESIAN_POINT('Origin',(-1.39368931909176,83.8,-31.8139162599729));
#63741=CARTESIAN_POINT('Origin',(5.15749672629266,83.8,-31.6928392700737));
#63742=CARTESIAN_POINT('',(5.15749672629266,83.8,-31.6928392700737));
#63743=CARTESIAN_POINT('',(5.59063152870137,83.8,-34.5469113743268));
#63744=CARTESIAN_POINT('Origin',(2.46923037857264,83.8,-30.6409089600963));
#63745=CARTESIAN_POINT('',(2.46923037857264,83.8,-30.6409089600963));
#63746=CARTESIAN_POINT('Origin',(0.214098833261289,83.8,-32.443050754372));
#63747=CARTESIAN_POINT('',(0.214098833261289,83.8,-32.443050754372));
#63748=CARTESIAN_POINT('Origin',(0.647233635670021,83.8,-35.2971228586251));
#63749=CARTESIAN_POINT('',(0.647233635670021,83.8,-35.2971228586251));
#63750=CARTESIAN_POINT('Origin',(3.33549998339005,83.8,-36.3490531686025));
#63751=CARTESIAN_POINT('',(3.33549998339005,83.8,-36.3490531686025));
#63752=CARTESIAN_POINT('Origin',(5.59063152870137,83.8,-34.5469113743268));
#63753=CARTESIAN_POINT('Origin',(30.3793106863527,83.8,-111.309797894252));
#63754=CARTESIAN_POINT('',(30.3793106863527,83.8,-111.309797894252));
#63755=CARTESIAN_POINT('',(30.8124454887614,83.8,-114.163869998505));
#63756=CARTESIAN_POINT('Origin',(27.6910443386327,83.8,-110.257867584275));
#63757=CARTESIAN_POINT('',(27.6910443386327,83.8,-110.257867584275));
#63758=CARTESIAN_POINT('Origin',(25.4359127933213,83.8,-112.06000937855));
#63759=CARTESIAN_POINT('',(25.4359127933213,83.8,-112.06000937855));
#63760=CARTESIAN_POINT('Origin',(25.86904759573,83.8,-114.914081482803));
#63761=CARTESIAN_POINT('',(25.86904759573,83.8,-114.914081482803));
#63762=CARTESIAN_POINT('Origin',(28.5573139434501,83.8,-115.966011792781));
#63763=CARTESIAN_POINT('',(28.5573139434501,83.8,-115.966011792781));
#63764=CARTESIAN_POINT('Origin',(30.8124454887614,83.8,-114.163869998505));
#63765=CARTESIAN_POINT('Origin',(23.3949898385595,83.8,-108.576802779898));
#63766=CARTESIAN_POINT('',(23.3949898385595,83.8,-108.576802779898));
#63767=CARTESIAN_POINT('',(23.8281246409682,83.8,-111.430874884151));
#63768=CARTESIAN_POINT('Origin',(20.7067234908395,83.8,-107.524872469921));
#63769=CARTESIAN_POINT('',(20.7067234908395,83.8,-107.524872469921));
#63770=CARTESIAN_POINT('Origin',(18.4515919455282,83.8,-109.327014264196));
#63771=CARTESIAN_POINT('',(18.4515919455282,83.8,-109.327014264196));
#63772=CARTESIAN_POINT('Origin',(18.8847267479369,83.8,-112.18108636845));
#63773=CARTESIAN_POINT('',(18.8847267479369,83.8,-112.18108636845));
#63774=CARTESIAN_POINT('Origin',(21.5729930956569,83.8,-113.233016678427));
#63775=CARTESIAN_POINT('',(21.5729930956569,83.8,-113.233016678427));
#63776=CARTESIAN_POINT('Origin',(23.8281246409682,83.8,-111.430874884151));
#63777=CARTESIAN_POINT('Origin',(16.4106689907664,83.8,-105.843807665544));
#63778=CARTESIAN_POINT('',(16.4106689907664,83.8,-105.843807665544));
#63779=CARTESIAN_POINT('',(16.8438037931751,83.8,-108.697879769797));
#63780=CARTESIAN_POINT('Origin',(13.7224026430464,83.8,-104.791877355567));
#63781=CARTESIAN_POINT('',(13.7224026430464,83.8,-104.791877355567));
#63782=CARTESIAN_POINT('Origin',(11.467271097735,83.8,-106.594019149843));
#63783=CARTESIAN_POINT('',(11.467271097735,83.8,-106.594019149843));
#63784=CARTESIAN_POINT('Origin',(11.9004059001438,83.8,-109.448091254096));
#63785=CARTESIAN_POINT('',(11.9004059001438,83.8,-109.448091254096));
#63786=CARTESIAN_POINT('Origin',(14.5886722478638,83.8,-110.500021564073));
#63787=CARTESIAN_POINT('',(14.5886722478638,83.8,-110.500021564073));
#63788=CARTESIAN_POINT('Origin',(16.8438037931751,83.8,-108.697879769797));
#63789=CARTESIAN_POINT('Origin',(9.42634814297327,83.8,-103.11081255119));
#63790=CARTESIAN_POINT('',(9.42634814297327,83.8,-103.11081255119));
#63791=CARTESIAN_POINT('',(9.85948294538199,83.8,-105.964884655444));
#63792=CARTESIAN_POINT('Origin',(6.73808179525326,83.8,-102.058882241213));
#63793=CARTESIAN_POINT('',(6.73808179525326,83.8,-102.058882241213));
#63794=CARTESIAN_POINT('Origin',(4.48295024994191,83.8,-103.861024035489));
#63795=CARTESIAN_POINT('',(4.48295024994191,83.8,-103.861024035489));
#63796=CARTESIAN_POINT('Origin',(4.91608505235064,83.8,-106.715096139742));
#63797=CARTESIAN_POINT('',(4.91608505235064,83.8,-106.715096139742));
#63798=CARTESIAN_POINT('Origin',(7.60435140007067,83.8,-107.767026449719));
#63799=CARTESIAN_POINT('',(7.60435140007067,83.8,-107.767026449719));
#63800=CARTESIAN_POINT('Origin',(9.85948294538199,83.8,-105.964884655444));
#63801=CARTESIAN_POINT('Origin',(2.44202729518014,83.8,-100.377817436837));
#63802=CARTESIAN_POINT('',(2.44202729518014,83.8,-100.377817436837));
#63803=CARTESIAN_POINT('',(2.87516209758886,83.8,-103.23188954109));
#63804=CARTESIAN_POINT('Origin',(-0.246239052539871,83.8,-99.3258871268591));
#63805=CARTESIAN_POINT('',(-0.246239052539871,83.8,-99.3258871268591));
#63806=CARTESIAN_POINT('Origin',(-2.50137059785123,83.8,-101.128028921135));
#63807=CARTESIAN_POINT('',(-2.50137059785123,83.8,-101.128028921135));
#63808=CARTESIAN_POINT('Origin',(-2.06823579544249,83.8,-103.982101025388));
#63809=CARTESIAN_POINT('',(-2.06823579544249,83.8,-103.982101025388));
#63810=CARTESIAN_POINT('Origin',(0.620030552277533,83.8,-105.034031335365));
#63811=CARTESIAN_POINT('',(0.620030552277533,83.8,-105.034031335365));
#63812=CARTESIAN_POINT('Origin',(2.87516209758886,83.8,-103.23188954109));
#63813=CARTESIAN_POINT('Origin',(-4.54229355261299,83.8,-97.6448223224826));
#63814=CARTESIAN_POINT('',(-4.54229355261299,83.8,-97.6448223224826));
#63815=CARTESIAN_POINT('',(-4.10915875020428,83.8,-100.498894426736));
#63816=CARTESIAN_POINT('Origin',(-7.230559900333,83.8,-96.5928920125052));
#63817=CARTESIAN_POINT('',(-7.230559900333,83.8,-96.5928920125052));
#63818=CARTESIAN_POINT('Origin',(-9.48569144564436,83.8,-98.3950338067809));
#63819=CARTESIAN_POINT('',(-9.48569144564436,83.8,-98.3950338067809));
#63820=CARTESIAN_POINT('Origin',(-9.05255664323563,83.8,-101.249105911034));
#63821=CARTESIAN_POINT('',(-9.05255664323563,83.8,-101.249105911034));
#63822=CARTESIAN_POINT('Origin',(-6.3642902955156,83.8,-102.301036221011));
#63823=CARTESIAN_POINT('',(-6.3642902955156,83.8,-102.301036221011));
#63824=CARTESIAN_POINT('Origin',(-4.10915875020428,83.8,-100.498894426736));
#63825=CARTESIAN_POINT('Origin',(-11.5266144004061,83.8,-94.9118272081287));
#63826=CARTESIAN_POINT('',(-11.5266144004061,83.8,-94.9118272081287));
#63827=CARTESIAN_POINT('',(-11.0934795979974,83.8,-97.7658993123818));
#63828=CARTESIAN_POINT('Origin',(-14.2148807481261,83.8,-93.8598968981513));
#63829=CARTESIAN_POINT('',(-14.2148807481261,83.8,-93.8598968981513));
#63830=CARTESIAN_POINT('Origin',(-16.4700122934375,83.8,-95.662038692427));
#63831=CARTESIAN_POINT('',(-16.4700122934375,83.8,-95.662038692427));
#63832=CARTESIAN_POINT('Origin',(-16.0368774910288,83.8,-98.5161107966801));
#63833=CARTESIAN_POINT('',(-16.0368774910288,83.8,-98.5161107966801));
#63834=CARTESIAN_POINT('Origin',(-13.3486111433087,83.8,-99.5680411066575));
#63835=CARTESIAN_POINT('',(-13.3486111433087,83.8,-99.5680411066575));
#63836=CARTESIAN_POINT('Origin',(-11.0934795979974,83.8,-97.7658993123818));
#63837=CARTESIAN_POINT('Origin',(-18.5109352481993,83.8,-92.1788320937748));
#63838=CARTESIAN_POINT('',(-18.5109352481993,83.8,-92.1788320937748));
#63839=CARTESIAN_POINT('',(-18.0778004457905,83.8,-95.0329041980279));
#63840=CARTESIAN_POINT('Origin',(-21.1992015959193,83.8,-91.1269017837974));
#63841=CARTESIAN_POINT('',(-21.1992015959193,83.8,-91.1269017837974));
#63842=CARTESIAN_POINT('Origin',(-23.4543331412306,83.8,-92.9290435780731));
#63843=CARTESIAN_POINT('',(-23.4543331412306,83.8,-92.9290435780731));
#63844=CARTESIAN_POINT('Origin',(-23.0211983388219,83.8,-95.7831156823262));
#63845=CARTESIAN_POINT('',(-23.0211983388219,83.8,-95.7831156823262));
#63846=CARTESIAN_POINT('Origin',(-20.3329319911019,83.8,-96.8350459923036));
#63847=CARTESIAN_POINT('',(-20.3329319911019,83.8,-96.8350459923036));
#63848=CARTESIAN_POINT('Origin',(-18.0778004457905,83.8,-95.0329041980279));
#63849=CARTESIAN_POINT('Origin',(-25.4952560959924,83.8,-89.4458369794209));
#63850=CARTESIAN_POINT('',(-25.4952560959924,83.8,-89.4458369794209));
#63851=CARTESIAN_POINT('',(-25.0621212935837,83.8,-92.2999090836741));
#63852=CARTESIAN_POINT('Origin',(-28.1835224437124,83.8,-88.3939066694435));
#63853=CARTESIAN_POINT('',(-28.1835224437124,83.8,-88.3939066694435));
#63854=CARTESIAN_POINT('Origin',(-30.4386539890237,83.8,-90.1960484637193));
#63855=CARTESIAN_POINT('',(-30.4386539890237,83.8,-90.1960484637193));
#63856=CARTESIAN_POINT('Origin',(-30.005519186615,83.8,-93.0501205679723));
#63857=CARTESIAN_POINT('',(-30.005519186615,83.8,-93.0501205679723));
#63858=CARTESIAN_POINT('Origin',(-27.317252838895,83.8,-94.1020508779497));
#63859=CARTESIAN_POINT('',(-27.317252838895,83.8,-94.1020508779497));
#63860=CARTESIAN_POINT('Origin',(-25.0621212935837,83.8,-92.2999090836741));
#63861=CARTESIAN_POINT('Origin',(-32.4795769437855,83.8,-86.7128418650671));
#63862=CARTESIAN_POINT('',(-32.4795769437855,83.8,-86.7128418650671));
#63863=CARTESIAN_POINT('',(-32.0464421413768,83.8,-89.5669139693202));
#63864=CARTESIAN_POINT('Origin',(-35.1678432915055,83.8,-85.6609115550896));
#63865=CARTESIAN_POINT('',(-35.1678432915055,83.8,-85.6609115550896));
#63866=CARTESIAN_POINT('Origin',(-37.4229748368169,83.8,-87.4630533493654));
#63867=CARTESIAN_POINT('',(-37.4229748368169,83.8,-87.4630533493654));
#63868=CARTESIAN_POINT('Origin',(-36.9898400344081,83.8,-90.3171254536184));
#63869=CARTESIAN_POINT('',(-36.9898400344081,83.8,-90.3171254536184));
#63870=CARTESIAN_POINT('Origin',(-34.3015736866881,83.8,-91.3690557635958));
#63871=CARTESIAN_POINT('',(-34.3015736866881,83.8,-91.3690557635958));
#63872=CARTESIAN_POINT('Origin',(-32.0464421413768,83.8,-89.5669139693202));
#63873=CARTESIAN_POINT('Origin',(-39.4638977915786,83.8,-83.9798467507132));
#63874=CARTESIAN_POINT('',(-39.4638977915786,83.8,-83.9798467507132));
#63875=CARTESIAN_POINT('',(-39.0307629891699,83.8,-86.8339188549663));
#63876=CARTESIAN_POINT('Origin',(-42.1521641392987,83.8,-82.9279164407358));
#63877=CARTESIAN_POINT('',(-42.1521641392987,83.8,-82.9279164407358));
#63878=CARTESIAN_POINT('Origin',(-44.40729568461,83.8,-84.7300582350115));
#63879=CARTESIAN_POINT('',(-44.40729568461,83.8,-84.7300582350115));
#63880=CARTESIAN_POINT('Origin',(-43.9741608822013,83.8,-87.5841303392645));
#63881=CARTESIAN_POINT('',(-43.9741608822013,83.8,-87.5841303392645));
#63882=CARTESIAN_POINT('Origin',(-41.2858945344812,83.8,-88.636060649242));
#63883=CARTESIAN_POINT('',(-41.2858945344812,83.8,-88.636060649242));
#63884=CARTESIAN_POINT('Origin',(-39.0307629891699,83.8,-86.8339188549663));
#63885=CARTESIAN_POINT('Origin',(-46.4482186393718,83.8,-81.2468516363593));
#63886=CARTESIAN_POINT('',(-46.4482186393718,83.8,-81.2468516363593));
#63887=CARTESIAN_POINT('',(-46.0150838369631,83.8,-84.1009237406124));
#63888=CARTESIAN_POINT('Origin',(-49.1364849870918,83.8,-80.1949213263819));
#63889=CARTESIAN_POINT('',(-49.1364849870918,83.8,-80.1949213263819));
#63890=CARTESIAN_POINT('Origin',(-51.3916165324031,83.8,-81.9970631206576));
#63891=CARTESIAN_POINT('',(-51.3916165324031,83.8,-81.9970631206576));
#63892=CARTESIAN_POINT('Origin',(-50.9584817299944,83.8,-84.8511352249106));
#63893=CARTESIAN_POINT('',(-50.9584817299944,83.8,-84.8511352249106));
#63894=CARTESIAN_POINT('Origin',(-48.2702153822744,83.8,-85.9030655348881));
#63895=CARTESIAN_POINT('',(-48.2702153822744,83.8,-85.9030655348881));
#63896=CARTESIAN_POINT('Origin',(-46.0150838369631,83.8,-84.1009237406124));
#63897=CARTESIAN_POINT('Origin',(31.5046279128,83.8,-118.724894733799));
#63898=CARTESIAN_POINT('',(31.5046279128,83.8,-118.724894733799));
#63899=CARTESIAN_POINT('',(31.9377627152088,83.8,-121.578966838052));
#63900=CARTESIAN_POINT('Origin',(28.81636156508,83.8,-117.672964423822));
#63901=CARTESIAN_POINT('',(28.81636156508,83.8,-117.672964423822));
#63902=CARTESIAN_POINT('Origin',(26.5612300197687,83.8,-119.475106218097));
#63903=CARTESIAN_POINT('',(26.5612300197687,83.8,-119.475106218097));
#63904=CARTESIAN_POINT('Origin',(26.9943648221774,83.8,-122.32917832235));
#63905=CARTESIAN_POINT('',(26.9943648221774,83.8,-122.32917832235));
#63906=CARTESIAN_POINT('Origin',(29.6826311698974,83.8,-123.381108632328));
#63907=CARTESIAN_POINT('',(29.6826311698974,83.8,-123.381108632328));
#63908=CARTESIAN_POINT('Origin',(31.9377627152088,83.8,-121.578966838052));
#63909=CARTESIAN_POINT('Origin',(24.5203070650069,83.8,-115.991899619445));
#63910=CARTESIAN_POINT('',(24.5203070650069,83.8,-115.991899619445));
#63911=CARTESIAN_POINT('',(24.9534418674156,83.8,-118.845971723698));
#63912=CARTESIAN_POINT('Origin',(21.8320407172869,83.8,-114.939969309468));
#63913=CARTESIAN_POINT('',(21.8320407172869,83.8,-114.939969309468));
#63914=CARTESIAN_POINT('Origin',(19.5769091719755,83.8,-116.742111103744));
#63915=CARTESIAN_POINT('',(19.5769091719755,83.8,-116.742111103744));
#63916=CARTESIAN_POINT('Origin',(20.0100439743843,83.8,-119.596183207997));
#63917=CARTESIAN_POINT('',(20.0100439743843,83.8,-119.596183207997));
#63918=CARTESIAN_POINT('Origin',(22.6983103221043,83.8,-120.648113517974));
#63919=CARTESIAN_POINT('',(22.6983103221043,83.8,-120.648113517974));
#63920=CARTESIAN_POINT('Origin',(24.9534418674156,83.8,-118.845971723698));
#63921=CARTESIAN_POINT('Origin',(17.5359862172138,83.8,-113.258904505091));
#63922=CARTESIAN_POINT('',(17.5359862172138,83.8,-113.258904505091));
#63923=CARTESIAN_POINT('',(17.9691210196225,83.8,-116.112976609344));
#63924=CARTESIAN_POINT('Origin',(14.8477198694938,83.8,-112.206974195114));
#63925=CARTESIAN_POINT('',(14.8477198694938,83.8,-112.206974195114));
#63926=CARTESIAN_POINT('Origin',(12.5925883241824,83.8,-114.00911598939));
#63927=CARTESIAN_POINT('',(12.5925883241824,83.8,-114.00911598939));
#63928=CARTESIAN_POINT('Origin',(13.0257231265911,83.8,-116.863188093643));
#63929=CARTESIAN_POINT('',(13.0257231265911,83.8,-116.863188093643));
#63930=CARTESIAN_POINT('Origin',(15.7139894743112,83.8,-117.91511840362));
#63931=CARTESIAN_POINT('',(15.7139894743112,83.8,-117.91511840362));
#63932=CARTESIAN_POINT('Origin',(17.9691210196225,83.8,-116.112976609344));
#63933=CARTESIAN_POINT('Origin',(10.5516653694206,83.8,-110.525909390737));
#63934=CARTESIAN_POINT('',(10.5516653694206,83.8,-110.525909390737));
#63935=CARTESIAN_POINT('',(10.9848001718294,83.8,-113.379981494991));
#63936=CARTESIAN_POINT('Origin',(7.86339902170064,83.8,-109.47397908076));
#63937=CARTESIAN_POINT('',(7.86339902170064,83.8,-109.47397908076));
#63938=CARTESIAN_POINT('Origin',(5.60826747638928,83.8,-111.276120875036));
#63939=CARTESIAN_POINT('',(5.60826747638928,83.8,-111.276120875036));
#63940=CARTESIAN_POINT('Origin',(6.04140227879801,83.8,-114.130192979289));
#63941=CARTESIAN_POINT('',(6.04140227879801,83.8,-114.130192979289));
#63942=CARTESIAN_POINT('Origin',(8.72966862651804,83.8,-115.182123289266));
#63943=CARTESIAN_POINT('',(8.72966862651804,83.8,-115.182123289266));
#63944=CARTESIAN_POINT('Origin',(10.9848001718294,83.8,-113.379981494991));
#63945=CARTESIAN_POINT('Origin',(1.31671006873277,83.8,-92.9627205972894));
#63946=CARTESIAN_POINT('',(1.31671006873277,83.8,-92.9627205972894));
#63947=CARTESIAN_POINT('',(1.74984487114149,83.8,-95.8167927015425));
#63948=CARTESIAN_POINT('Origin',(-1.37155627898724,83.8,-91.910790287312));
#63949=CARTESIAN_POINT('',(-1.37155627898724,83.8,-91.910790287312));
#63950=CARTESIAN_POINT('Origin',(-3.6266878242986,83.8,-93.7129320815877));
#63951=CARTESIAN_POINT('',(-3.6266878242986,83.8,-93.7129320815877));
#63952=CARTESIAN_POINT('Origin',(-3.19355302188986,83.8,-96.5670041858408));
#63953=CARTESIAN_POINT('',(-3.19355302188986,83.8,-96.5670041858408));
#63954=CARTESIAN_POINT('Origin',(-0.505286674169835,83.8,-97.6189344958182));
#63955=CARTESIAN_POINT('',(-0.505286674169835,83.8,-97.6189344958182));
#63956=CARTESIAN_POINT('Origin',(1.74984487114149,83.8,-95.8167927015425));
#63957=CARTESIAN_POINT('Origin',(8.3010309165259,83.8,-95.6957157116433));
#63958=CARTESIAN_POINT('',(8.3010309165259,83.8,-95.6957157116433));
#63959=CARTESIAN_POINT('',(8.73416571893462,83.8,-98.5497878158964));
#63960=CARTESIAN_POINT('Origin',(5.6127645688059,83.8,-94.6437854016659));
#63961=CARTESIAN_POINT('',(5.6127645688059,83.8,-94.6437854016659));
#63962=CARTESIAN_POINT('Origin',(3.35763302349454,83.8,-96.4459271959416));
#63963=CARTESIAN_POINT('',(3.35763302349454,83.8,-96.4459271959416));
#63964=CARTESIAN_POINT('Origin',(3.79076782590327,83.8,-99.2999993001947));
#63965=CARTESIAN_POINT('',(3.79076782590327,83.8,-99.2999993001947));
#63966=CARTESIAN_POINT('Origin',(6.4790341736233,83.8,-100.351929610172));
#63967=CARTESIAN_POINT('',(6.4790341736233,83.8,-100.351929610172));
#63968=CARTESIAN_POINT('Origin',(8.73416571893462,83.8,-98.5497878158964));
#63969=CARTESIAN_POINT('Origin',(15.285351764319,83.8,-98.4287108259972));
#63970=CARTESIAN_POINT('',(15.285351764319,83.8,-98.4287108259972));
#63971=CARTESIAN_POINT('',(15.7184865667278,83.8,-101.28278293025));
#63972=CARTESIAN_POINT('Origin',(12.597085416599,83.8,-97.3767805160198));
#63973=CARTESIAN_POINT('',(12.597085416599,83.8,-97.3767805160198));
#63974=CARTESIAN_POINT('Origin',(10.3419538712877,83.8,-99.1789223102955));
#63975=CARTESIAN_POINT('',(10.3419538712877,83.8,-99.1789223102955));
#63976=CARTESIAN_POINT('Origin',(10.7750886736964,83.8,-102.032994414549));
#63977=CARTESIAN_POINT('',(10.7750886736964,83.8,-102.032994414549));
#63978=CARTESIAN_POINT('Origin',(13.4633550214164,83.8,-103.084924724526));
#63979=CARTESIAN_POINT('',(13.4633550214164,83.8,-103.084924724526));
#63980=CARTESIAN_POINT('Origin',(15.7184865667278,83.8,-101.28278293025));
#63981=CARTESIAN_POINT('Origin',(22.2696726121122,83.8,-101.161705940351));
#63982=CARTESIAN_POINT('',(22.2696726121122,83.8,-101.161705940351));
#63983=CARTESIAN_POINT('',(22.7028074145209,83.8,-104.015778044604));
#63984=CARTESIAN_POINT('Origin',(19.5814062643922,83.8,-100.109775630374));
#63985=CARTESIAN_POINT('',(19.5814062643922,83.8,-100.109775630374));
#63986=CARTESIAN_POINT('Origin',(17.3262747190808,83.8,-101.911917424649));
#63987=CARTESIAN_POINT('',(17.3262747190808,83.8,-101.911917424649));
#63988=CARTESIAN_POINT('Origin',(17.7594095214895,83.8,-104.765989528902));
#63989=CARTESIAN_POINT('',(17.7594095214895,83.8,-104.765989528902));
#63990=CARTESIAN_POINT('Origin',(20.4476758692096,83.8,-105.81791983888));
#63991=CARTESIAN_POINT('',(20.4476758692096,83.8,-105.81791983888));
#63992=CARTESIAN_POINT('Origin',(22.7028074145209,83.8,-104.015778044604));
#63993=CARTESIAN_POINT('Origin',(-48.6988530922665,83.8,-66.4166579572652));
#63994=CARTESIAN_POINT('',(-48.6988530922665,83.8,-66.4166579572652));
#63995=CARTESIAN_POINT('',(-48.2657182898578,83.8,-69.2707300615183));
#63996=CARTESIAN_POINT('Origin',(-51.3871194399865,83.8,-65.3647276472878));
#63997=CARTESIAN_POINT('',(-51.3871194399865,83.8,-65.3647276472878));
#63998=CARTESIAN_POINT('Origin',(-53.6422509852979,83.8,-67.1668694415634));
#63999=CARTESIAN_POINT('',(-53.6422509852979,83.8,-67.1668694415634));
#64000=CARTESIAN_POINT('Origin',(-53.2091161828892,83.8,-70.0209415458165));
#64001=CARTESIAN_POINT('',(-53.2091161828892,83.8,-70.0209415458165));
#64002=CARTESIAN_POINT('Origin',(-50.5208498351691,83.8,-71.0728718557939));
#64003=CARTESIAN_POINT('',(-50.5208498351691,83.8,-71.0728718557939));
#64004=CARTESIAN_POINT('Origin',(-48.2657182898578,83.8,-69.2707300615183));
#64005=CARTESIAN_POINT('Origin',(43.2226351554916,83.8,-109.360691283413));
#64006=CARTESIAN_POINT('',(43.2226351554916,83.8,-109.360691283413));
#64007=CARTESIAN_POINT('',(43.6557699579003,83.8,-112.214763387666));
#64008=CARTESIAN_POINT('Origin',(40.5343688077715,83.8,-108.308760973435));
#64009=CARTESIAN_POINT('',(40.5343688077715,83.8,-108.308760973435));
#64010=CARTESIAN_POINT('Origin',(38.2792372624602,83.8,-110.110902767711));
#64011=CARTESIAN_POINT('',(38.2792372624602,83.8,-110.110902767711));
#64012=CARTESIAN_POINT('Origin',(38.7123720648689,83.8,-112.964974871964));
#64013=CARTESIAN_POINT('',(38.7123720648689,83.8,-112.964974871964));
#64014=CARTESIAN_POINT('Origin',(41.4006384125889,83.8,-114.016905181942));
#64015=CARTESIAN_POINT('',(41.4006384125889,83.8,-114.016905181942));
#64016=CARTESIAN_POINT('Origin',(43.6557699579003,83.8,-112.214763387666));
#64017=CARTESIAN_POINT('Origin',(36.2383143076984,83.8,-106.627696169059));
#64018=CARTESIAN_POINT('',(36.2383143076984,83.8,-106.627696169059));
#64019=CARTESIAN_POINT('',(36.6714491101071,83.8,-109.481768273312));
#64020=CARTESIAN_POINT('Origin',(33.5500479599784,83.8,-105.575765859081));
#64021=CARTESIAN_POINT('',(33.5500479599784,83.8,-105.575765859081));
#64022=CARTESIAN_POINT('Origin',(31.2949164146671,83.8,-107.377907653357));
#64023=CARTESIAN_POINT('',(31.2949164146671,83.8,-107.377907653357));
#64024=CARTESIAN_POINT('Origin',(31.7280512170758,83.8,-110.23197975761));
#64025=CARTESIAN_POINT('',(31.7280512170758,83.8,-110.23197975761));
#64026=CARTESIAN_POINT('Origin',(34.4163175647958,83.8,-111.283910067588));
#64027=CARTESIAN_POINT('',(34.4163175647958,83.8,-111.283910067588));
#64028=CARTESIAN_POINT('Origin',(36.6714491101071,83.8,-109.481768273312));
#64029=CARTESIAN_POINT('Origin',(29.2539934599053,83.8,-103.894701054705));
#64030=CARTESIAN_POINT('',(29.2539934599053,83.8,-103.894701054705));
#64031=CARTESIAN_POINT('',(29.687128262314,83.8,-106.748773158958));
#64032=CARTESIAN_POINT('Origin',(26.5657271121853,83.8,-102.842770744728));
#64033=CARTESIAN_POINT('',(26.5657271121853,83.8,-102.842770744728));
#64034=CARTESIAN_POINT('Origin',(24.3105955668739,83.8,-104.644912539003));
#64035=CARTESIAN_POINT('',(24.3105955668739,83.8,-104.644912539003));
#64036=CARTESIAN_POINT('Origin',(24.7437303692827,83.8,-107.498984643256));
#64037=CARTESIAN_POINT('',(24.7437303692827,83.8,-107.498984643256));
#64038=CARTESIAN_POINT('Origin',(27.4319967170027,83.8,-108.550914953234));
#64039=CARTESIAN_POINT('',(27.4319967170027,83.8,-108.550914953234));
#64040=CARTESIAN_POINT('Origin',(29.687128262314,83.8,-106.748773158958));
#64041=CARTESIAN_POINT('Origin',(-33.6048941702329,83.8,-79.29774502552));
#64042=CARTESIAN_POINT('',(-33.6048941702329,83.8,-79.29774502552));
#64043=CARTESIAN_POINT('',(-33.1717593678242,83.8,-82.1518171297731));
#64044=CARTESIAN_POINT('Origin',(-36.2931605179529,83.8,-78.2458147155426));
#64045=CARTESIAN_POINT('',(-36.2931605179529,83.8,-78.2458147155426));
#64046=CARTESIAN_POINT('Origin',(-38.5482920632642,83.8,-80.0479565098183));
#64047=CARTESIAN_POINT('',(-38.5482920632642,83.8,-80.0479565098183));
#64048=CARTESIAN_POINT('Origin',(-38.1151572608555,83.8,-82.9020286140714));
#64049=CARTESIAN_POINT('',(-38.1151572608555,83.8,-82.9020286140714));
#64050=CARTESIAN_POINT('Origin',(-35.4268909131355,83.8,-83.9539589240488));
#64051=CARTESIAN_POINT('',(-35.4268909131355,83.8,-83.9539589240488));
#64052=CARTESIAN_POINT('Origin',(-33.1717593678242,83.8,-82.1518171297731));
#64053=CARTESIAN_POINT('Origin',(-40.589215018026,83.8,-76.5647499111661));
#64054=CARTESIAN_POINT('',(-40.589215018026,83.8,-76.5647499111661));
#64055=CARTESIAN_POINT('',(-40.1560802156173,83.8,-79.4188220154192));
#64056=CARTESIAN_POINT('Origin',(-43.277481365746,83.8,-75.5128196011887));
#64057=CARTESIAN_POINT('',(-43.277481365746,83.8,-75.5128196011887));
#64058=CARTESIAN_POINT('Origin',(-45.5326129110574,83.8,-77.3149613954644));
#64059=CARTESIAN_POINT('',(-45.5326129110574,83.8,-77.3149613954644));
#64060=CARTESIAN_POINT('Origin',(-45.0994781086486,83.8,-80.1690334997174));
#64061=CARTESIAN_POINT('',(-45.0994781086486,83.8,-80.1690334997174));
#64062=CARTESIAN_POINT('Origin',(-42.4112117609286,83.8,-81.2209638096949));
#64063=CARTESIAN_POINT('',(-42.4112117609286,83.8,-81.2209638096949));
#64064=CARTESIAN_POINT('Origin',(-40.1560802156173,83.8,-79.4188220154192));
#64065=CARTESIAN_POINT('Origin',(-47.5735358658191,83.8,-73.8317547968122));
#64066=CARTESIAN_POINT('',(-47.5735358658191,83.8,-73.8317547968122));
#64067=CARTESIAN_POINT('',(-47.1404010634104,83.8,-76.6858269010653));
#64068=CARTESIAN_POINT('Origin',(-50.2618022135392,83.8,-72.7798244868348));
#64069=CARTESIAN_POINT('',(-50.2618022135392,83.8,-72.7798244868348));
#64070=CARTESIAN_POINT('Origin',(-52.5169337588505,83.8,-74.5819662811105));
#64071=CARTESIAN_POINT('',(-52.5169337588505,83.8,-74.5819662811105));
#64072=CARTESIAN_POINT('Origin',(-52.0837989564418,83.8,-77.4360383853636));
#64073=CARTESIAN_POINT('',(-52.0837989564418,83.8,-77.4360383853636));
#64074=CARTESIAN_POINT('Origin',(-49.3955326087217,83.8,-78.487968695341));
#64075=CARTESIAN_POINT('',(-49.3955326087217,83.8,-78.487968695341));
#64076=CARTESIAN_POINT('Origin',(-47.1404010634104,83.8,-76.6858269010653));
#64077=CARTESIAN_POINT('Origin',(37.3636315341458,83.8,-114.042793008606));
#64078=CARTESIAN_POINT('',(37.3636315341458,83.8,-114.042793008606));
#64079=CARTESIAN_POINT('',(37.7967663365545,83.8,-116.896865112859));
#64080=CARTESIAN_POINT('Origin',(34.6753651864258,83.8,-112.990862698629));
#64081=CARTESIAN_POINT('',(34.6753651864258,83.8,-112.990862698629));
#64082=CARTESIAN_POINT('Origin',(32.4202336411144,83.8,-114.793004492904));
#64083=CARTESIAN_POINT('',(32.4202336411144,83.8,-114.793004492904));
#64084=CARTESIAN_POINT('Origin',(32.8533684435232,83.8,-117.647076597157));
#64085=CARTESIAN_POINT('',(32.8533684435232,83.8,-117.647076597157));
#64086=CARTESIAN_POINT('Origin',(35.5416347912432,83.8,-118.699006907135));
#64087=CARTESIAN_POINT('',(35.5416347912432,83.8,-118.699006907135));
#64088=CARTESIAN_POINT('Origin',(37.7967663365545,83.8,-116.896865112859));
#64089=CARTESIAN_POINT('Origin',(-26.6205733224398,83.8,-82.0307401398739));
#64090=CARTESIAN_POINT('',(-26.6205733224398,83.8,-82.0307401398739));
#64091=CARTESIAN_POINT('',(-26.187438520031,83.8,-84.884812244127));
#64092=CARTESIAN_POINT('Origin',(-29.3088396701598,83.8,-80.9788098298965));
#64093=CARTESIAN_POINT('',(-29.3088396701598,83.8,-80.9788098298965));
#64094=CARTESIAN_POINT('Origin',(-31.5639712154711,83.8,-82.7809516241722));
#64095=CARTESIAN_POINT('',(-31.5639712154711,83.8,-82.7809516241722));
#64096=CARTESIAN_POINT('Origin',(-31.1308364130624,83.8,-85.6350237284252));
#64097=CARTESIAN_POINT('',(-31.1308364130624,83.8,-85.6350237284252));
#64098=CARTESIAN_POINT('Origin',(-28.4425700653424,83.8,-86.6869540384027));
#64099=CARTESIAN_POINT('',(-28.4425700653424,83.8,-86.6869540384027));
#64100=CARTESIAN_POINT('Origin',(-26.187438520031,83.8,-84.884812244127));
#64101=CARTESIAN_POINT('Origin',(-19.6362524746466,83.8,-84.7637352542278));
#64102=CARTESIAN_POINT('',(-19.6362524746466,83.8,-84.7637352542278));
#64103=CARTESIAN_POINT('',(-19.2031176722379,83.8,-87.6178073584809));
#64104=CARTESIAN_POINT('Origin',(-22.3245188223666,83.8,-83.7118049442504));
#64105=CARTESIAN_POINT('',(-22.3245188223666,83.8,-83.7118049442504));
#64106=CARTESIAN_POINT('Origin',(-24.579650367678,83.8,-85.5139467385261));
#64107=CARTESIAN_POINT('',(-24.579650367678,83.8,-85.5139467385261));
#64108=CARTESIAN_POINT('Origin',(-24.1465155652693,83.8,-88.3680188427791));
#64109=CARTESIAN_POINT('',(-24.1465155652693,83.8,-88.3680188427791));
#64110=CARTESIAN_POINT('Origin',(-21.4582492175492,83.8,-89.4199491527566));
#64111=CARTESIAN_POINT('',(-21.4582492175492,83.8,-89.4199491527566));
#64112=CARTESIAN_POINT('Origin',(-19.2031176722379,83.8,-87.6178073584809));
#64113=CARTESIAN_POINT('Origin',(-12.6519316268535,83.8,-87.4967303685817));
#64114=CARTESIAN_POINT('',(-12.6519316268535,83.8,-87.4967303685817));
#64115=CARTESIAN_POINT('',(-12.2187968244448,83.8,-90.3508024728348));
#64116=CARTESIAN_POINT('Origin',(-15.3401979745735,83.8,-86.4448000586042));
#64117=CARTESIAN_POINT('',(-15.3401979745735,83.8,-86.4448000586042));
#64118=CARTESIAN_POINT('Origin',(-17.5953295198849,83.8,-88.2469418528799));
#64119=CARTESIAN_POINT('',(-17.5953295198849,83.8,-88.2469418528799));
#64120=CARTESIAN_POINT('Origin',(-17.1621947174761,83.8,-91.101013957133));
#64121=CARTESIAN_POINT('',(-17.1621947174761,83.8,-91.101013957133));
#64122=CARTESIAN_POINT('Origin',(-14.4739283697561,83.8,-92.1529442671104));
#64123=CARTESIAN_POINT('',(-14.4739283697561,83.8,-92.1529442671104));
#64124=CARTESIAN_POINT('Origin',(-12.2187968244448,83.8,-90.3508024728348));
#64125=CARTESIAN_POINT('Origin',(-5.66761077906036,83.8,-90.2297254829355));
#64126=CARTESIAN_POINT('',(-5.66761077906036,83.8,-90.2297254829355));
#64127=CARTESIAN_POINT('',(-5.23447597665164,83.8,-93.0837975871887));
#64128=CARTESIAN_POINT('Origin',(-8.35587712678037,83.8,-89.1777951729581));
#64129=CARTESIAN_POINT('',(-8.35587712678037,83.8,-89.1777951729581));
#64130=CARTESIAN_POINT('Origin',(-10.6110086720917,83.8,-90.9799369672338));
#64131=CARTESIAN_POINT('',(-10.6110086720917,83.8,-90.9799369672338));
#64132=CARTESIAN_POINT('Origin',(-10.177873869683,83.8,-93.8340090714869));
#64133=CARTESIAN_POINT('',(-10.177873869683,83.8,-93.8340090714869));
#64134=CARTESIAN_POINT('Origin',(-7.48960752196297,83.8,-94.8859393814643));
#64135=CARTESIAN_POINT('',(-7.48960752196297,83.8,-94.8859393814643));
#64136=CARTESIAN_POINT('Origin',(-5.23447597665164,83.8,-93.0837975871887));
#64137=CARTESIAN_POINT('Origin',(-15.1349835688571,83.8,-114.424122612416));
#64138=CARTESIAN_POINT('',(-15.1349835688571,83.8,-114.424122612416));
#64139=CARTESIAN_POINT('',(-14.7018487664484,83.8,-117.278194716669));
#64140=CARTESIAN_POINT('Origin',(-17.8232499165771,83.8,-113.372192302439));
#64141=CARTESIAN_POINT('',(-17.8232499165771,83.8,-113.372192302439));
#64142=CARTESIAN_POINT('Origin',(-20.0783814618885,83.8,-115.174334096714));
#64143=CARTESIAN_POINT('',(-20.0783814618885,83.8,-115.174334096714));
#64144=CARTESIAN_POINT('Origin',(-19.6452466594797,83.8,-118.028406200967));
#64145=CARTESIAN_POINT('',(-19.6452466594797,83.8,-118.028406200967));
#64146=CARTESIAN_POINT('Origin',(-16.9569803117597,83.8,-119.080336510945));
#64147=CARTESIAN_POINT('',(-16.9569803117597,83.8,-119.080336510945));
#64148=CARTESIAN_POINT('Origin',(-14.7018487664484,83.8,-117.278194716669));
#64149=CARTESIAN_POINT('Origin',(-8.15066272106398,83.8,-117.15711772677));
#64150=CARTESIAN_POINT('',(-8.15066272106398,83.8,-117.15711772677));
#64151=CARTESIAN_POINT('',(-7.71752791865526,83.8,-120.011189831023));
#64152=CARTESIAN_POINT('Origin',(-10.838929068784,83.8,-116.105187416792));
#64153=CARTESIAN_POINT('',(-10.838929068784,83.8,-116.105187416792));
#64154=CARTESIAN_POINT('Origin',(-13.0940606140953,83.8,-117.907329211068));
#64155=CARTESIAN_POINT('',(-13.0940606140953,83.8,-117.907329211068));
#64156=CARTESIAN_POINT('Origin',(-12.6609258116866,83.8,-120.761401315321));
#64157=CARTESIAN_POINT('',(-12.6609258116866,83.8,-120.761401315321));
#64158=CARTESIAN_POINT('Origin',(-9.97265946396659,83.8,-121.813331625299));
#64159=CARTESIAN_POINT('',(-9.97265946396659,83.8,-121.813331625299));
#64160=CARTESIAN_POINT('Origin',(-7.71752791865526,83.8,-120.011189831023));
#64161=CARTESIAN_POINT('Origin',(-1.16634187327085,83.8,-119.890112841124));
#64162=CARTESIAN_POINT('',(-1.16634187327085,83.8,-119.890112841124));
#64163=CARTESIAN_POINT('',(-0.733207070862132,83.8,-122.744184945377));
#64164=CARTESIAN_POINT('Origin',(-3.85460822099086,83.8,-118.838182531146));
#64165=CARTESIAN_POINT('',(-3.85460822099086,83.8,-118.838182531146));
#64166=CARTESIAN_POINT('Origin',(-6.10973976630222,83.8,-120.640324325422));
#64167=CARTESIAN_POINT('',(-6.10973976630222,83.8,-120.640324325422));
#64168=CARTESIAN_POINT('Origin',(-5.67660496389348,83.8,-123.494396429675));
#64169=CARTESIAN_POINT('',(-5.67660496389348,83.8,-123.494396429675));
#64170=CARTESIAN_POINT('Origin',(-2.98833861617346,83.8,-124.546326739653));
#64171=CARTESIAN_POINT('',(-2.98833861617346,83.8,-124.546326739653));
#64172=CARTESIAN_POINT('Origin',(-0.733207070862132,83.8,-122.744184945377));
#64173=CARTESIAN_POINT('Origin',(5.81797897452228,83.8,-122.623107955478));
#64174=CARTESIAN_POINT('',(5.81797897452228,83.8,-122.623107955478));
#64175=CARTESIAN_POINT('',(6.251113776931,83.8,-125.477180059731));
#64176=CARTESIAN_POINT('Origin',(3.12971262680227,83.8,-121.5711776455));
#64177=CARTESIAN_POINT('',(3.12971262680227,83.8,-121.5711776455));
#64178=CARTESIAN_POINT('Origin',(0.874581081490917,83.8,-123.373319439776));
#64179=CARTESIAN_POINT('',(0.874581081490917,83.8,-123.373319439776));
#64180=CARTESIAN_POINT('Origin',(1.30771588389965,83.8,-126.227391544029));
#64181=CARTESIAN_POINT('',(1.30771588389965,83.8,-126.227391544029));
#64182=CARTESIAN_POINT('Origin',(3.99598223161968,83.8,-127.279321854006));
#64183=CARTESIAN_POINT('',(3.99598223161968,83.8,-127.279321854006));
#64184=CARTESIAN_POINT('Origin',(6.251113776931,83.8,-125.477180059731));
#64185=CARTESIAN_POINT('Origin',(-30.2289424908907,83.8,-101.543035544161));
#64186=CARTESIAN_POINT('',(-30.2289424908907,83.8,-101.543035544161));
#64187=CARTESIAN_POINT('',(-29.795807688482,83.8,-104.397107648414));
#64188=CARTESIAN_POINT('Origin',(-32.9172088386108,83.8,-100.491105234184));
#64189=CARTESIAN_POINT('',(-32.9172088386108,83.8,-100.491105234184));
#64190=CARTESIAN_POINT('Origin',(-35.1723403839221,83.8,-102.293247028459));
#64191=CARTESIAN_POINT('',(-35.1723403839221,83.8,-102.293247028459));
#64192=CARTESIAN_POINT('Origin',(-34.7392055815134,83.8,-105.147319132713));
#64193=CARTESIAN_POINT('',(-34.7392055815134,83.8,-105.147319132713));
#64194=CARTESIAN_POINT('Origin',(-32.0509392337934,83.8,-106.19924944269));
#64195=CARTESIAN_POINT('',(-32.0509392337934,83.8,-106.19924944269));
#64196=CARTESIAN_POINT('Origin',(-29.795807688482,83.8,-104.397107648414));
#64197=CARTESIAN_POINT('Origin',(-37.2132633386839,83.8,-98.8100404298073));
#64198=CARTESIAN_POINT('',(-37.2132633386839,83.8,-98.8100404298073));
#64199=CARTESIAN_POINT('',(-36.7801285362752,83.8,-101.66411253406));
#64200=CARTESIAN_POINT('Origin',(-39.9015296864039,83.8,-97.7581101198299));
#64201=CARTESIAN_POINT('',(-39.9015296864039,83.8,-97.7581101198299));
#64202=CARTESIAN_POINT('Origin',(-42.1566612317152,83.8,-99.5602519141056));
#64203=CARTESIAN_POINT('',(-42.1566612317152,83.8,-99.5602519141056));
#64204=CARTESIAN_POINT('Origin',(-41.7235264293065,83.8,-102.414324018359));
#64205=CARTESIAN_POINT('',(-41.7235264293065,83.8,-102.414324018359));
#64206=CARTESIAN_POINT('Origin',(-39.0352600815865,83.8,-103.466254328336));
#64207=CARTESIAN_POINT('',(-39.0352600815865,83.8,-103.466254328336));
#64208=CARTESIAN_POINT('Origin',(-36.7801285362752,83.8,-101.66411253406));
#64209=CARTESIAN_POINT('Origin',(-44.197584186477,83.8,-96.0770453154534));
#64210=CARTESIAN_POINT('',(-44.197584186477,83.8,-96.0770453154534));
#64211=CARTESIAN_POINT('',(-43.7644493840683,83.8,-98.9311174197065));
#64212=CARTESIAN_POINT('Origin',(-46.885850534197,83.8,-95.025115005476));
#64213=CARTESIAN_POINT('',(-46.885850534197,83.8,-95.025115005476));
#64214=CARTESIAN_POINT('Origin',(-49.1409820795084,83.8,-96.8272567997517));
#64215=CARTESIAN_POINT('',(-49.1409820795084,83.8,-96.8272567997517));
#64216=CARTESIAN_POINT('Origin',(-48.7078472770996,83.8,-99.6813289040047));
#64217=CARTESIAN_POINT('',(-48.7078472770996,83.8,-99.6813289040047));
#64218=CARTESIAN_POINT('Origin',(-46.0195809293796,83.8,-100.733259213982));
#64219=CARTESIAN_POINT('',(-46.0195809293796,83.8,-100.733259213982));
#64220=CARTESIAN_POINT('Origin',(-43.7644493840683,83.8,-98.9311174197065));
#64221=CARTESIAN_POINT('Origin',(12.8022998223154,83.8,-125.356103069832));
#64222=CARTESIAN_POINT('',(12.8022998223154,83.8,-125.356103069832));
#64223=CARTESIAN_POINT('',(13.2354346247241,83.8,-128.210175174085));
#64224=CARTESIAN_POINT('Origin',(10.1140334745954,83.8,-124.304172759854));
#64225=CARTESIAN_POINT('',(10.1140334745954,83.8,-124.304172759854));
#64226=CARTESIAN_POINT('Origin',(7.85890192928405,83.8,-126.10631455413));
#64227=CARTESIAN_POINT('',(7.85890192928405,83.8,-126.10631455413));
#64228=CARTESIAN_POINT('Origin',(8.29203673169278,83.8,-128.960386658383));
#64229=CARTESIAN_POINT('',(8.29203673169278,83.8,-128.960386658383));
#64230=CARTESIAN_POINT('Origin',(10.9803030794128,83.8,-130.01231696836));
#64231=CARTESIAN_POINT('',(10.9803030794128,83.8,-130.01231696836));
#64232=CARTESIAN_POINT('Origin',(13.2354346247241,83.8,-128.210175174085));
#64233=CARTESIAN_POINT('Origin',(-22.1193044166502,83.8,-111.691127498062));
#64234=CARTESIAN_POINT('',(-22.1193044166502,83.8,-111.691127498062));
#64235=CARTESIAN_POINT('',(-21.6861696142415,83.8,-114.545199602315));
#64236=CARTESIAN_POINT('Origin',(-24.8075707643703,83.8,-110.639197188085));
#64237=CARTESIAN_POINT('',(-24.8075707643703,83.8,-110.639197188085));
#64238=CARTESIAN_POINT('Origin',(-27.0627023096816,83.8,-112.44133898236));
#64239=CARTESIAN_POINT('',(-27.0627023096816,83.8,-112.44133898236));
#64240=CARTESIAN_POINT('Origin',(-26.6295675072729,83.8,-115.295411086613));
#64241=CARTESIAN_POINT('',(-26.6295675072729,83.8,-115.295411086613));
#64242=CARTESIAN_POINT('Origin',(-23.9413011595528,83.8,-116.347341396591));
#64243=CARTESIAN_POINT('',(-23.9413011595528,83.8,-116.347341396591));
#64244=CARTESIAN_POINT('Origin',(-21.6861696142415,83.8,-114.545199602315));
#64245=CARTESIAN_POINT('Origin',(-29.1036252644434,83.8,-108.958132383708));
#64246=CARTESIAN_POINT('',(-29.1036252644434,83.8,-108.958132383708));
#64247=CARTESIAN_POINT('',(-28.6704904620347,83.8,-111.812204487961));
#64248=CARTESIAN_POINT('Origin',(-31.7918916121634,83.8,-107.906202073731));
#64249=CARTESIAN_POINT('',(-31.7918916121634,83.8,-107.906202073731));
#64250=CARTESIAN_POINT('Origin',(-34.0470231574747,83.8,-109.708343868006));
#64251=CARTESIAN_POINT('',(-34.0470231574747,83.8,-109.708343868006));
#64252=CARTESIAN_POINT('Origin',(-33.613888355066,83.8,-112.56241597226));
#64253=CARTESIAN_POINT('',(-33.613888355066,83.8,-112.56241597226));
#64254=CARTESIAN_POINT('Origin',(-30.925622007346,83.8,-113.614346282237));
#64255=CARTESIAN_POINT('',(-30.925622007346,83.8,-113.614346282237));
#64256=CARTESIAN_POINT('Origin',(-28.6704904620347,83.8,-111.812204487961));
#64257=CARTESIAN_POINT('Origin',(-36.0879461122365,83.8,-106.225137269354));
#64258=CARTESIAN_POINT('',(-36.0879461122365,83.8,-106.225137269354));
#64259=CARTESIAN_POINT('',(-35.6548113098278,83.8,-109.079209373607));
#64260=CARTESIAN_POINT('Origin',(-38.7762124599565,83.8,-105.173206959377));
#64261=CARTESIAN_POINT('',(-38.7762124599565,83.8,-105.173206959377));
#64262=CARTESIAN_POINT('Origin',(-41.0313440052679,83.8,-106.975348753653));
#64263=CARTESIAN_POINT('',(-41.0313440052679,83.8,-106.975348753653));
#64264=CARTESIAN_POINT('Origin',(-40.5982092028591,83.8,-109.829420857906));
#64265=CARTESIAN_POINT('',(-40.5982092028591,83.8,-109.829420857906));
#64266=CARTESIAN_POINT('Origin',(-37.9099428551391,83.8,-110.881351167883));
#64267=CARTESIAN_POINT('',(-37.9099428551391,83.8,-110.881351167883));
#64268=CARTESIAN_POINT('Origin',(-35.6548113098278,83.8,-109.079209373607));
#64269=CARTESIAN_POINT('Origin',(-43.0722669600296,83.8,-103.492142155));
#64270=CARTESIAN_POINT('',(-43.0722669600296,83.8,-103.492142155));
#64271=CARTESIAN_POINT('',(-42.6391321576209,83.8,-106.346214259254));
#64272=CARTESIAN_POINT('Origin',(-45.7605333077496,83.8,-102.440211845023));
#64273=CARTESIAN_POINT('',(-45.7605333077496,83.8,-102.440211845023));
#64274=CARTESIAN_POINT('Origin',(-48.015664853061,83.8,-104.242353639299));
#64275=CARTESIAN_POINT('',(-48.015664853061,83.8,-104.242353639299));
#64276=CARTESIAN_POINT('Origin',(-47.5825300506523,83.8,-107.096425743552));
#64277=CARTESIAN_POINT('',(-47.5825300506523,83.8,-107.096425743552));
#64278=CARTESIAN_POINT('Origin',(-44.8942637029322,83.8,-108.148356053529));
#64279=CARTESIAN_POINT('',(-44.8942637029322,83.8,-108.148356053529));
#64280=CARTESIAN_POINT('Origin',(-42.6391321576209,83.8,-106.346214259254));
#64281=CARTESIAN_POINT('Origin',(-0.0410246468234739,83.8,-127.305209680671));
#64282=CARTESIAN_POINT('',(-0.0410246468234739,83.8,-127.305209680671));
#64283=CARTESIAN_POINT('',(0.392110155585244,83.8,-130.159281784924));
#64284=CARTESIAN_POINT('Origin',(-2.72929099454348,83.8,-126.253279370693));
#64285=CARTESIAN_POINT('',(-2.72929099454348,83.8,-126.253279370693));
#64286=CARTESIAN_POINT('Origin',(-4.98442253985484,83.8,-128.055421164969));
#64287=CARTESIAN_POINT('',(-4.98442253985484,83.8,-128.055421164969));
#64288=CARTESIAN_POINT('Origin',(-4.55128773744611,83.8,-130.909493269222));
#64289=CARTESIAN_POINT('',(-4.55128773744611,83.8,-130.909493269222));
#64290=CARTESIAN_POINT('Origin',(-1.86302138972608,83.8,-131.9614235792));
#64291=CARTESIAN_POINT('',(-1.86302138972608,83.8,-131.9614235792));
#64292=CARTESIAN_POINT('Origin',(0.392110155585244,83.8,-130.159281784924));
#64293=CARTESIAN_POINT('Origin',(-7.02534549461661,83.8,-124.572214566317));
#64294=CARTESIAN_POINT('',(-7.02534549461661,83.8,-124.572214566317));
#64295=CARTESIAN_POINT('',(-6.59221069220789,83.8,-127.42628667057));
#64296=CARTESIAN_POINT('Origin',(-9.71361184233662,83.8,-123.52028425634));
#64297=CARTESIAN_POINT('',(-9.71361184233662,83.8,-123.52028425634));
#64298=CARTESIAN_POINT('Origin',(-11.968743387648,83.8,-125.322426050615));
#64299=CARTESIAN_POINT('',(-11.968743387648,83.8,-125.322426050615));
#64300=CARTESIAN_POINT('Origin',(-11.5356085852392,83.8,-128.176498154868));
#64301=CARTESIAN_POINT('',(-11.5356085852392,83.8,-128.176498154868));
#64302=CARTESIAN_POINT('Origin',(-8.84734223751921,83.8,-129.228428464846));
#64303=CARTESIAN_POINT('',(-8.84734223751921,83.8,-129.228428464846));
#64304=CARTESIAN_POINT('Origin',(-6.59221069220789,83.8,-127.42628667057));
#64305=CARTESIAN_POINT('Origin',(-14.0096663424097,83.8,-121.839219451963));
#64306=CARTESIAN_POINT('',(-14.0096663424097,83.8,-121.839219451963));
#64307=CARTESIAN_POINT('',(-13.576531540001,83.8,-124.693291556216));
#64308=CARTESIAN_POINT('Origin',(-16.6979326901297,83.8,-120.787289141986));
#64309=CARTESIAN_POINT('',(-16.6979326901297,83.8,-120.787289141986));
#64310=CARTESIAN_POINT('Origin',(-18.9530642354411,83.8,-122.589430936261));
#64311=CARTESIAN_POINT('',(-18.9530642354411,83.8,-122.589430936261));
#64312=CARTESIAN_POINT('Origin',(-18.5199294330324,83.8,-125.443503040514));
#64313=CARTESIAN_POINT('',(-18.5199294330324,83.8,-125.443503040514));
#64314=CARTESIAN_POINT('Origin',(-15.8316630853123,83.8,-126.495433350492));
#64315=CARTESIAN_POINT('',(-15.8316630853123,83.8,-126.495433350492));
#64316=CARTESIAN_POINT('Origin',(-13.576531540001,83.8,-124.693291556216));
#64317=CARTESIAN_POINT('Origin',(-20.9939871902029,83.8,-119.106224337609));
#64318=CARTESIAN_POINT('',(-20.9939871902029,83.8,-119.106224337609));
#64319=CARTESIAN_POINT('',(-20.5608523877941,83.8,-121.960296441862));
#64320=CARTESIAN_POINT('Origin',(-23.6822535379229,83.8,-118.054294027632));
#64321=CARTESIAN_POINT('',(-23.6822535379229,83.8,-118.054294027632));
#64322=CARTESIAN_POINT('Origin',(-25.9373850832342,83.8,-119.856435821907));
#64323=CARTESIAN_POINT('',(-25.9373850832342,83.8,-119.856435821907));
#64324=CARTESIAN_POINT('Origin',(-25.5042502808255,83.8,-122.710507926161));
#64325=CARTESIAN_POINT('',(-25.5042502808255,83.8,-122.710507926161));
#64326=CARTESIAN_POINT('Origin',(-22.8159839331055,83.8,-123.762438236138));
#64327=CARTESIAN_POINT('',(-22.8159839331055,83.8,-123.762438236138));
#64328=CARTESIAN_POINT('Origin',(-20.5608523877941,83.8,-121.960296441862));
#64329=CARTESIAN_POINT('Origin',(3.56734452162752,83.8,-107.792914276384));
#64330=CARTESIAN_POINT('',(3.56734452162752,83.8,-107.792914276384));
#64331=CARTESIAN_POINT('',(4.00047932403624,83.8,-110.646986380637));
#64332=CARTESIAN_POINT('Origin',(0.879078173907508,83.8,-106.740983966406));
#64333=CARTESIAN_POINT('',(0.879078173907508,83.8,-106.740983966406));
#64334=CARTESIAN_POINT('Origin',(-1.37605337140385,83.8,-108.543125760682));
#64335=CARTESIAN_POINT('',(-1.37605337140385,83.8,-108.543125760682));
#64336=CARTESIAN_POINT('Origin',(-0.942918568995116,83.8,-111.397197864935));
#64337=CARTESIAN_POINT('',(-0.942918568995116,83.8,-111.397197864935));
#64338=CARTESIAN_POINT('Origin',(1.74534777872491,83.8,-112.449128174912));
#64339=CARTESIAN_POINT('',(1.74534777872491,83.8,-112.449128174912));
#64340=CARTESIAN_POINT('Origin',(4.00047932403624,83.8,-110.646986380637));
#64341=CARTESIAN_POINT('Origin',(-3.41697632616561,83.8,-105.05991916203));
#64342=CARTESIAN_POINT('',(-3.41697632616561,83.8,-105.05991916203));
#64343=CARTESIAN_POINT('',(-2.9838415237569,83.8,-107.913991266283));
#64344=CARTESIAN_POINT('Origin',(-6.10524267388563,83.8,-104.007988852052));
#64345=CARTESIAN_POINT('',(-6.10524267388563,83.8,-104.007988852052));
#64346=CARTESIAN_POINT('Origin',(-8.36037421919698,83.8,-105.810130646328));
#64347=CARTESIAN_POINT('',(-8.36037421919698,83.8,-105.810130646328));
#64348=CARTESIAN_POINT('Origin',(-7.92723941678825,83.8,-108.664202750581));
#64349=CARTESIAN_POINT('',(-7.92723941678825,83.8,-108.664202750581));
#64350=CARTESIAN_POINT('Origin',(-5.23897306906822,83.8,-109.716133060558));
#64351=CARTESIAN_POINT('',(-5.23897306906822,83.8,-109.716133060558));
#64352=CARTESIAN_POINT('Origin',(-2.9838415237569,83.8,-107.913991266283));
#64353=CARTESIAN_POINT('Origin',(-10.4012971739587,83.8,-102.326924047676));
#64354=CARTESIAN_POINT('',(-10.4012971739587,83.8,-102.326924047676));
#64355=CARTESIAN_POINT('',(-9.96816237155003,83.8,-105.180996151929));
#64356=CARTESIAN_POINT('Origin',(-13.0895635216788,83.8,-101.274993737698));
#64357=CARTESIAN_POINT('',(-13.0895635216788,83.8,-101.274993737698));
#64358=CARTESIAN_POINT('Origin',(-15.3446950669901,83.8,-103.077135531974));
#64359=CARTESIAN_POINT('',(-15.3446950669901,83.8,-103.077135531974));
#64360=CARTESIAN_POINT('Origin',(-14.9115602645814,83.8,-105.931207636227));
#64361=CARTESIAN_POINT('',(-14.9115602645814,83.8,-105.931207636227));
#64362=CARTESIAN_POINT('Origin',(-12.2232939168614,83.8,-106.983137946205));
#64363=CARTESIAN_POINT('',(-12.2232939168614,83.8,-106.983137946205));
#64364=CARTESIAN_POINT('Origin',(-9.96816237155003,83.8,-105.180996151929));
#64365=CARTESIAN_POINT('Origin',(-17.3856180217519,83.8,-99.5939289333219));
#64366=CARTESIAN_POINT('',(-17.3856180217519,83.8,-99.5939289333219));
#64367=CARTESIAN_POINT('',(-16.9524832193432,83.8,-102.448001037575));
#64368=CARTESIAN_POINT('Origin',(-20.0738843694719,83.8,-98.5419986233445));
#64369=CARTESIAN_POINT('',(-20.0738843694719,83.8,-98.5419986233445));
#64370=CARTESIAN_POINT('Origin',(-22.3290159147832,83.8,-100.34414041762));
#64371=CARTESIAN_POINT('',(-22.3290159147832,83.8,-100.34414041762));
#64372=CARTESIAN_POINT('Origin',(-21.8958811123745,83.8,-103.198212521873));
#64373=CARTESIAN_POINT('',(-21.8958811123745,83.8,-103.198212521873));
#64374=CARTESIAN_POINT('Origin',(-19.2076147646545,83.8,-104.250142831851));
#64375=CARTESIAN_POINT('',(-19.2076147646545,83.8,-104.250142831851));
#64376=CARTESIAN_POINT('Origin',(-16.9524832193432,83.8,-102.448001037575));
#64377=CARTESIAN_POINT('Origin',(-24.369938869545,83.8,-96.860933818968));
#64378=CARTESIAN_POINT('',(-24.369938869545,83.8,-96.860933818968));
#64379=CARTESIAN_POINT('',(-23.9368040671363,83.8,-99.7150059232211));
#64380=CARTESIAN_POINT('Origin',(-27.058205217265,83.8,-95.8090035089906));
#64381=CARTESIAN_POINT('',(-27.058205217265,83.8,-95.8090035089906));
#64382=CARTESIAN_POINT('Origin',(-29.3133367625764,83.8,-97.6111453032663));
#64383=CARTESIAN_POINT('',(-29.3133367625764,83.8,-97.6111453032663));
#64384=CARTESIAN_POINT('Origin',(-28.8802019601676,83.8,-100.465217407519));
#64385=CARTESIAN_POINT('',(-28.8802019601676,83.8,-100.465217407519));
#64386=CARTESIAN_POINT('Origin',(-26.1919356124476,83.8,-101.517147717497));
#64387=CARTESIAN_POINT('',(-26.1919356124476,83.8,-101.517147717497));
#64388=CARTESIAN_POINT('Origin',(-23.9368040671363,83.8,-99.7150059232211));
#64389=CARTESIAN_POINT('Origin',(-31.3542597173381,83.8,-94.1279387046141));
#64390=CARTESIAN_POINT('',(-31.3542597173381,83.8,-94.1279387046141));
#64391=CARTESIAN_POINT('',(-30.9211249149294,83.8,-96.9820108088672));
#64392=CARTESIAN_POINT('Origin',(-34.0425260650581,83.8,-93.0760083946367));
#64393=CARTESIAN_POINT('',(-34.0425260650581,83.8,-93.0760083946367));
#64394=CARTESIAN_POINT('Origin',(-36.2976576103695,83.8,-94.8781501889124));
#64395=CARTESIAN_POINT('',(-36.2976576103695,83.8,-94.8781501889124));
#64396=CARTESIAN_POINT('Origin',(-35.8645228079608,83.8,-97.7322222931655));
#64397=CARTESIAN_POINT('',(-35.8645228079608,83.8,-97.7322222931655));
#64398=CARTESIAN_POINT('Origin',(-33.1762564602408,83.8,-98.7841526031429));
#64399=CARTESIAN_POINT('',(-33.1762564602408,83.8,-98.7841526031429));
#64400=CARTESIAN_POINT('Origin',(-30.9211249149294,83.8,-96.9820108088672));
#64401=CARTESIAN_POINT('Origin',(-38.3385805651313,83.8,-91.3949435902602));
#64402=CARTESIAN_POINT('',(-38.3385805651313,83.8,-91.3949435902602));
#64403=CARTESIAN_POINT('',(-37.9054457627226,83.8,-94.2490156945133));
#64404=CARTESIAN_POINT('Origin',(-41.0268469128513,83.8,-90.3430132802828));
#64405=CARTESIAN_POINT('',(-41.0268469128513,83.8,-90.3430132802828));
#64406=CARTESIAN_POINT('Origin',(-43.2819784581626,83.8,-92.1451550745585));
#64407=CARTESIAN_POINT('',(-43.2819784581626,83.8,-92.1451550745585));
#64408=CARTESIAN_POINT('Origin',(-42.8488436557539,83.8,-94.9992271788116));
#64409=CARTESIAN_POINT('',(-42.8488436557539,83.8,-94.9992271788116));
#64410=CARTESIAN_POINT('Origin',(-40.1605773080339,83.8,-96.051157488789));
#64411=CARTESIAN_POINT('',(-40.1605773080339,83.8,-96.051157488789));
#64412=CARTESIAN_POINT('Origin',(-37.9054457627226,83.8,-94.2490156945133));
#64413=CARTESIAN_POINT('Origin',(-45.3229014129244,83.8,-88.6619484759063));
#64414=CARTESIAN_POINT('',(-45.3229014129244,83.8,-88.6619484759063));
#64415=CARTESIAN_POINT('',(-44.8897666105157,83.8,-91.5160205801594));
#64416=CARTESIAN_POINT('Origin',(-48.0111677606444,83.8,-87.6100181659289));
#64417=CARTESIAN_POINT('',(-48.0111677606444,83.8,-87.6100181659289));
#64418=CARTESIAN_POINT('Origin',(-50.2662993059558,83.8,-89.4121599602046));
#64419=CARTESIAN_POINT('',(-50.2662993059558,83.8,-89.4121599602046));
#64420=CARTESIAN_POINT('Origin',(-49.833164503547,83.8,-92.2662320644577));
#64421=CARTESIAN_POINT('',(-49.833164503547,83.8,-92.2662320644577));
#64422=CARTESIAN_POINT('Origin',(-47.144898155827,83.8,-93.3181623744351));
#64423=CARTESIAN_POINT('',(-47.144898155827,83.8,-93.3181623744351));
#64424=CARTESIAN_POINT('Origin',(-44.8897666105157,83.8,-91.5160205801594));
#64425=CARTESIAN_POINT('Origin',(25.6456242914543,83.8,-123.406996458992));
#64426=CARTESIAN_POINT('',(25.6456242914543,83.8,-123.406996458992));
#64427=CARTESIAN_POINT('',(26.078759093863,83.8,-126.261068563245));
#64428=CARTESIAN_POINT('Origin',(22.9573579437343,83.8,-122.355066149015));
#64429=CARTESIAN_POINT('',(22.9573579437343,83.8,-122.355066149015));
#64430=CARTESIAN_POINT('Origin',(20.7022263984229,83.8,-124.157207943291));
#64431=CARTESIAN_POINT('',(20.7022263984229,83.8,-124.157207943291));
#64432=CARTESIAN_POINT('Origin',(21.1353612008317,83.8,-127.011280047544));
#64433=CARTESIAN_POINT('',(21.1353612008317,83.8,-127.011280047544));
#64434=CARTESIAN_POINT('Origin',(23.8236275485517,83.8,-128.063210357521));
#64435=CARTESIAN_POINT('',(23.8236275485517,83.8,-128.063210357521));
#64436=CARTESIAN_POINT('Origin',(26.078759093863,83.8,-126.261068563245));
#64437=CARTESIAN_POINT('Origin',(18.6613034436612,83.8,-120.674001344638));
#64438=CARTESIAN_POINT('',(18.6613034436612,83.8,-120.674001344638));
#64439=CARTESIAN_POINT('',(19.0944382460699,83.8,-123.528073448892));
#64440=CARTESIAN_POINT('Origin',(15.9730370959412,83.8,-119.622071034661));
#64441=CARTESIAN_POINT('',(15.9730370959412,83.8,-119.622071034661));
#64442=CARTESIAN_POINT('Origin',(13.7179055506298,83.8,-121.424212828937));
#64443=CARTESIAN_POINT('',(13.7179055506298,83.8,-121.424212828937));
#64444=CARTESIAN_POINT('Origin',(14.1510403530385,83.8,-124.27828493319));
#64445=CARTESIAN_POINT('',(14.1510403530385,83.8,-124.27828493319));
#64446=CARTESIAN_POINT('Origin',(16.8393067007586,83.8,-125.330215243167));
#64447=CARTESIAN_POINT('',(16.8393067007586,83.8,-125.330215243167));
#64448=CARTESIAN_POINT('Origin',(19.0944382460699,83.8,-123.528073448892));
#64449=CARTESIAN_POINT('Origin',(11.676982595868,83.8,-117.941006230285));
#64450=CARTESIAN_POINT('',(11.676982595868,83.8,-117.941006230285));
#64451=CARTESIAN_POINT('',(12.1101173982768,83.8,-120.795078334538));
#64452=CARTESIAN_POINT('Origin',(8.98871624814803,83.8,-116.889075920307));
#64453=CARTESIAN_POINT('',(8.98871624814803,83.8,-116.889075920307));
#64454=CARTESIAN_POINT('Origin',(6.73358470283667,83.8,-118.691217714583));
#64455=CARTESIAN_POINT('',(6.73358470283667,83.8,-118.691217714583));
#64456=CARTESIAN_POINT('Origin',(7.1667195052454,83.8,-121.545289818836));
#64457=CARTESIAN_POINT('',(7.1667195052454,83.8,-121.545289818836));
#64458=CARTESIAN_POINT('Origin',(9.85498585296543,83.8,-122.597220128813));
#64459=CARTESIAN_POINT('',(9.85498585296543,83.8,-122.597220128813));
#64460=CARTESIAN_POINT('Origin',(12.1101173982768,83.8,-120.795078334538));
#64461=CARTESIAN_POINT('Origin',(4.69266174807491,83.8,-115.208011115931));
#64462=CARTESIAN_POINT('',(4.69266174807491,83.8,-115.208011115931));
#64463=CARTESIAN_POINT('',(5.12579655048363,83.8,-118.062083220184));
#64464=CARTESIAN_POINT('Origin',(2.0043954003549,83.8,-114.156080805953));
#64465=CARTESIAN_POINT('',(2.0043954003549,83.8,-114.156080805953));
#64466=CARTESIAN_POINT('Origin',(-0.250736144956458,83.8,-115.958222600229));
#64467=CARTESIAN_POINT('',(-0.250736144956458,83.8,-115.958222600229));
#64468=CARTESIAN_POINT('Origin',(0.182398657452273,83.8,-118.812294704482));
#64469=CARTESIAN_POINT('',(0.182398657452273,83.8,-118.812294704482));
#64470=CARTESIAN_POINT('Origin',(2.8706650051723,83.8,-119.864225014459));
#64471=CARTESIAN_POINT('',(2.8706650051723,83.8,-119.864225014459));
#64472=CARTESIAN_POINT('Origin',(5.12579655048363,83.8,-118.062083220184));
#64473=CARTESIAN_POINT('Origin',(-2.29165909971822,83.8,-112.475016001577));
#64474=CARTESIAN_POINT('',(-2.29165909971822,83.8,-112.475016001577));
#64475=CARTESIAN_POINT('',(-1.85852429730951,83.8,-115.32908810583));
#64476=CARTESIAN_POINT('Origin',(-4.97992544743824,83.8,-111.423085691599));
#64477=CARTESIAN_POINT('',(-4.97992544743824,83.8,-111.423085691599));
#64478=CARTESIAN_POINT('Origin',(-7.23505699274959,83.8,-113.225227485875));
#64479=CARTESIAN_POINT('',(-7.23505699274959,83.8,-113.225227485875));
#64480=CARTESIAN_POINT('Origin',(-6.80192219034086,83.8,-116.079299590128));
#64481=CARTESIAN_POINT('',(-6.80192219034086,83.8,-116.079299590128));
#64482=CARTESIAN_POINT('Origin',(-4.11365584262083,83.8,-117.131229900105));
#64483=CARTESIAN_POINT('',(-4.11365584262083,83.8,-117.131229900105));
#64484=CARTESIAN_POINT('Origin',(-1.85852429730951,83.8,-115.32908810583));
#64485=CARTESIAN_POINT('Origin',(-9.27597994751136,83.8,-109.742020887223));
#64486=CARTESIAN_POINT('',(-9.27597994751136,83.8,-109.742020887223));
#64487=CARTESIAN_POINT('',(-8.84284514510264,83.8,-112.596092991476));
#64488=CARTESIAN_POINT('Origin',(-11.9642462952314,83.8,-108.690090577245));
#64489=CARTESIAN_POINT('',(-11.9642462952314,83.8,-108.690090577245));
#64490=CARTESIAN_POINT('Origin',(-14.2193778405427,83.8,-110.492232371521));
#64491=CARTESIAN_POINT('',(-14.2193778405427,83.8,-110.492232371521));
#64492=CARTESIAN_POINT('Origin',(-13.786243038134,83.8,-113.346304475774));
#64493=CARTESIAN_POINT('',(-13.786243038134,83.8,-113.346304475774));
#64494=CARTESIAN_POINT('Origin',(-11.097976690414,83.8,-114.398234785752));
#64495=CARTESIAN_POINT('',(-11.097976690414,83.8,-114.398234785752));
#64496=CARTESIAN_POINT('Origin',(-8.84284514510264,83.8,-112.596092991476));
#64497=CARTESIAN_POINT('Origin',(-16.2603007953045,83.8,-107.009025772869));
#64498=CARTESIAN_POINT('',(-16.2603007953045,83.8,-107.009025772869));
#64499=CARTESIAN_POINT('',(-15.8271659928958,83.8,-109.863097877122));
#64500=CARTESIAN_POINT('Origin',(-18.9485671430245,83.8,-105.957095462892));
#64501=CARTESIAN_POINT('',(-18.9485671430245,83.8,-105.957095462892));
#64502=CARTESIAN_POINT('Origin',(-21.2036986883359,83.8,-107.759237257167));
#64503=CARTESIAN_POINT('',(-21.2036986883359,83.8,-107.759237257167));
#64504=CARTESIAN_POINT('Origin',(-20.7705638859271,83.8,-110.61330936142));
#64505=CARTESIAN_POINT('',(-20.7705638859271,83.8,-110.61330936142));
#64506=CARTESIAN_POINT('Origin',(-18.0822975382071,83.8,-111.665239671398));
#64507=CARTESIAN_POINT('',(-18.0822975382071,83.8,-111.665239671398));
#64508=CARTESIAN_POINT('Origin',(-15.8271659928958,83.8,-109.863097877122));
#64509=CARTESIAN_POINT('Origin',(-23.2446216430976,83.8,-104.276030658515));
#64510=CARTESIAN_POINT('',(-23.2446216430976,83.8,-104.276030658515));
#64511=CARTESIAN_POINT('',(-22.8114868406889,83.8,-107.130102762768));
#64512=CARTESIAN_POINT('Origin',(-25.9328879908176,83.8,-103.224100348538));
#64513=CARTESIAN_POINT('',(-25.9328879908176,83.8,-103.224100348538));
#64514=CARTESIAN_POINT('Origin',(-28.188019536129,83.8,-105.026242142813));
#64515=CARTESIAN_POINT('',(-28.188019536129,83.8,-105.026242142813));
#64516=CARTESIAN_POINT('Origin',(-27.7548847337203,83.8,-107.880314247066));
#64517=CARTESIAN_POINT('',(-27.7548847337203,83.8,-107.880314247066));
#64518=CARTESIAN_POINT('Origin',(-25.0666183860002,83.8,-108.932244557044));
#64519=CARTESIAN_POINT('',(-25.0666183860002,83.8,-108.932244557044));
#64520=CARTESIAN_POINT('Origin',(-22.8114868406889,83.8,-107.130102762768));
#64521=CARTESIAN_POINT('Origin',(-24.1375213804361,83.8,-55.1033478960396));
#64522=CARTESIAN_POINT('',(-24.1375213804361,83.8,-55.1033478960396));
#64523=CARTESIAN_POINT('',(-23.7043865780274,83.8,-57.9574200002927));
#64524=CARTESIAN_POINT('Origin',(-26.8257877281561,83.8,-54.0514175860622));
#64525=CARTESIAN_POINT('',(-26.8257877281561,83.8,-54.0514175860622));
#64526=CARTESIAN_POINT('Origin',(-29.0809192734675,83.8,-55.8535593803378));
#64527=CARTESIAN_POINT('',(-29.0809192734675,83.8,-55.8535593803378));
#64528=CARTESIAN_POINT('Origin',(-28.6477844710588,83.8,-58.7076314845909));
#64529=CARTESIAN_POINT('',(-28.6477844710588,83.8,-58.7076314845909));
#64530=CARTESIAN_POINT('Origin',(-25.9595181233387,83.8,-59.7595617945683));
#64531=CARTESIAN_POINT('',(-25.9595181233387,83.8,-59.7595617945683));
#64532=CARTESIAN_POINT('Origin',(-23.7043865780274,83.8,-57.9574200002927));
#64533=CARTESIAN_POINT('Origin',(-31.1218422282293,83.8,-52.3703527816857));
#64534=CARTESIAN_POINT('',(-31.1218422282293,83.8,-52.3703527816857));
#64535=CARTESIAN_POINT('',(-30.6887074258205,83.8,-55.2244248859388));
#64536=CARTESIAN_POINT('Origin',(-33.8101085759493,83.8,-51.3184224717083));
#64537=CARTESIAN_POINT('',(-33.8101085759493,83.8,-51.3184224717083));
#64538=CARTESIAN_POINT('Origin',(-36.0652401212606,83.8,-53.120564265984));
#64539=CARTESIAN_POINT('',(-36.0652401212606,83.8,-53.120564265984));
#64540=CARTESIAN_POINT('Origin',(-35.6321053188519,83.8,-55.974636370237));
#64541=CARTESIAN_POINT('',(-35.6321053188519,83.8,-55.974636370237));
#64542=CARTESIAN_POINT('Origin',(-32.9438389711319,83.8,-57.0265666802144));
#64543=CARTESIAN_POINT('',(-32.9438389711319,83.8,-57.0265666802144));
#64544=CARTESIAN_POINT('Origin',(-30.6887074258205,83.8,-55.2244248859388));
#64545=CARTESIAN_POINT('Origin',(-38.1061630760224,83.8,-49.6373576673318));
#64546=CARTESIAN_POINT('',(-38.1061630760224,83.8,-49.6373576673318));
#64547=CARTESIAN_POINT('',(-37.6730282736137,83.8,-52.4914297715849));
#64548=CARTESIAN_POINT('Origin',(-40.7944294237424,83.8,-48.5854273573544));
#64549=CARTESIAN_POINT('',(-40.7944294237424,83.8,-48.5854273573544));
#64550=CARTESIAN_POINT('Origin',(-43.0495609690538,83.8,-50.3875691516301));
#64551=CARTESIAN_POINT('',(-43.0495609690538,83.8,-50.3875691516301));
#64552=CARTESIAN_POINT('Origin',(-42.616426166645,83.8,-53.2416412558831));
#64553=CARTESIAN_POINT('',(-42.616426166645,83.8,-53.2416412558831));
#64554=CARTESIAN_POINT('Origin',(-39.928159818925,83.8,-54.2935715658606));
#64555=CARTESIAN_POINT('',(-39.928159818925,83.8,-54.2935715658606));
#64556=CARTESIAN_POINT('Origin',(-37.6730282736137,83.8,-52.4914297715849));
#64557=CARTESIAN_POINT('Origin',(46.8310043239425,83.8,-89.8483958791255));
#64558=CARTESIAN_POINT('',(46.8310043239425,83.8,-89.8483958791255));
#64559=CARTESIAN_POINT('',(47.2641391263513,83.8,-92.7024679833786));
#64560=CARTESIAN_POINT('Origin',(44.1427379762225,83.8,-88.7964655691481));
#64561=CARTESIAN_POINT('',(44.1427379762225,83.8,-88.7964655691481));
#64562=CARTESIAN_POINT('Origin',(41.8876064309112,83.8,-90.5986073634238));
#64563=CARTESIAN_POINT('',(41.8876064309112,83.8,-90.5986073634238));
#64564=CARTESIAN_POINT('Origin',(42.3207412333199,83.8,-93.4526794676769));
#64565=CARTESIAN_POINT('',(42.3207412333199,83.8,-93.4526794676769));
#64566=CARTESIAN_POINT('Origin',(45.0090075810399,83.8,-94.5046097776543));
#64567=CARTESIAN_POINT('',(45.0090075810399,83.8,-94.5046097776543));
#64568=CARTESIAN_POINT('Origin',(47.2641391263513,83.8,-92.7024679833786));
#64569=CARTESIAN_POINT('Origin',(-17.153200532643,83.8,-57.8363430103935));
#64570=CARTESIAN_POINT('',(-17.153200532643,83.8,-57.8363430103935));
#64571=CARTESIAN_POINT('',(-16.7200657302343,83.8,-60.6904151146466));
#64572=CARTESIAN_POINT('Origin',(-19.841466880363,83.8,-56.784412700416));
#64573=CARTESIAN_POINT('',(-19.841466880363,83.8,-56.784412700416));
#64574=CARTESIAN_POINT('Origin',(-22.0965984256744,83.8,-58.5865544946917));
#64575=CARTESIAN_POINT('',(-22.0965984256744,83.8,-58.5865544946917));
#64576=CARTESIAN_POINT('Origin',(-21.6634636232656,83.8,-61.4406265989448));
#64577=CARTESIAN_POINT('',(-21.6634636232656,83.8,-61.4406265989448));
#64578=CARTESIAN_POINT('Origin',(-18.9751972755456,83.8,-62.4925569089222));
#64579=CARTESIAN_POINT('',(-18.9751972755456,83.8,-62.4925569089222));
#64580=CARTESIAN_POINT('Origin',(-16.7200657302343,83.8,-60.6904151146466));
#64581=CARTESIAN_POINT('Origin',(-10.1688796848499,83.8,-60.5693381247473));
#64582=CARTESIAN_POINT('',(-10.1688796848499,83.8,-60.5693381247473));
#64583=CARTESIAN_POINT('',(-9.73574488244115,83.8,-63.4234102290004));
#64584=CARTESIAN_POINT('Origin',(-12.8571460325699,83.8,-59.5174078147699));
#64585=CARTESIAN_POINT('',(-12.8571460325699,83.8,-59.5174078147699));
#64586=CARTESIAN_POINT('Origin',(-15.1122775778812,83.8,-61.3195496090456));
#64587=CARTESIAN_POINT('',(-15.1122775778812,83.8,-61.3195496090456));
#64588=CARTESIAN_POINT('Origin',(-14.6791427754725,83.8,-64.1736217132987));
#64589=CARTESIAN_POINT('',(-14.6791427754725,83.8,-64.1736217132987));
#64590=CARTESIAN_POINT('Origin',(-11.9908764277525,83.8,-65.2255520232761));
#64591=CARTESIAN_POINT('',(-11.9908764277525,83.8,-65.2255520232761));
#64592=CARTESIAN_POINT('Origin',(-9.73574488244115,83.8,-63.4234102290004));
#64593=CARTESIAN_POINT('Origin',(-3.18455883705674,83.8,-63.3023332391012));
#64594=CARTESIAN_POINT('',(-3.18455883705674,83.8,-63.3023332391012));
#64595=CARTESIAN_POINT('',(-2.75142403464802,83.8,-66.1564053433543));
#64596=CARTESIAN_POINT('Origin',(-5.87282518477675,83.8,-62.2504029291238));
#64597=CARTESIAN_POINT('',(-5.87282518477675,83.8,-62.2504029291238));
#64598=CARTESIAN_POINT('Origin',(-8.1279567300881,83.8,-64.0525447233995));
#64599=CARTESIAN_POINT('',(-8.1279567300881,83.8,-64.0525447233995));
#64600=CARTESIAN_POINT('Origin',(-7.69482192767937,83.8,-66.9066168276526));
#64601=CARTESIAN_POINT('',(-7.69482192767937,83.8,-66.9066168276526));
#64602=CARTESIAN_POINT('Origin',(-5.00655557995934,83.8,-67.95854713763));
#64603=CARTESIAN_POINT('',(-5.00655557995934,83.8,-67.95854713763));
#64604=CARTESIAN_POINT('Origin',(-2.75142403464802,83.8,-66.1564053433543));
#64605=CARTESIAN_POINT('Origin',(3.7997620107364,83.8,-66.0353283534551));
#64606=CARTESIAN_POINT('',(3.7997620107364,83.8,-66.0353283534551));
#64607=CARTESIAN_POINT('',(4.23289681314511,83.8,-68.8894004577082));
#64608=CARTESIAN_POINT('Origin',(1.11149566301639,83.8,-64.9833980434777));
#64609=CARTESIAN_POINT('',(1.11149566301639,83.8,-64.9833980434777));
#64610=CARTESIAN_POINT('Origin',(-1.14363588229497,83.8,-66.7855398377534));
#64611=CARTESIAN_POINT('',(-1.14363588229497,83.8,-66.7855398377534));
#64612=CARTESIAN_POINT('Origin',(-0.710501079886239,83.8,-69.6396119420065));
#64613=CARTESIAN_POINT('',(-0.710501079886239,83.8,-69.6396119420065));
#64614=CARTESIAN_POINT('Origin',(1.97776526783379,83.8,-70.6915422519839));
#64615=CARTESIAN_POINT('',(1.97776526783379,83.8,-70.6915422519839));
#64616=CARTESIAN_POINT('Origin',(4.23289681314511,83.8,-68.8894004577082));
#64617=CARTESIAN_POINT('Origin',(39.8466834761494,83.8,-87.1154007647716));
#64618=CARTESIAN_POINT('',(39.8466834761494,83.8,-87.1154007647716));
#64619=CARTESIAN_POINT('',(40.2798182785581,83.8,-89.9694728690247));
#64620=CARTESIAN_POINT('Origin',(37.1584171284294,83.8,-86.0634704547942));
#64621=CARTESIAN_POINT('',(37.1584171284294,83.8,-86.0634704547942));
#64622=CARTESIAN_POINT('Origin',(34.903285583118,83.8,-87.8656122490699));
#64623=CARTESIAN_POINT('',(34.903285583118,83.8,-87.8656122490699));
#64624=CARTESIAN_POINT('Origin',(35.3364203855268,83.8,-90.719684353323));
#64625=CARTESIAN_POINT('',(35.3364203855268,83.8,-90.719684353323));
#64626=CARTESIAN_POINT('Origin',(38.0246867332468,83.8,-91.7716146633004));
#64627=CARTESIAN_POINT('',(38.0246867332468,83.8,-91.7716146633004));
#64628=CARTESIAN_POINT('Origin',(40.2798182785581,83.8,-89.9694728690247));
#64629=CARTESIAN_POINT('Origin',(32.8623626283563,83.8,-84.3824056504177));
#64630=CARTESIAN_POINT('',(32.8623626283563,83.8,-84.3824056504177));
#64631=CARTESIAN_POINT('',(33.295497430765,83.8,-87.2364777546708));
#64632=CARTESIAN_POINT('Origin',(30.1740962806363,83.8,-83.3304753404403));
#64633=CARTESIAN_POINT('',(30.1740962806363,83.8,-83.3304753404403));
#64634=CARTESIAN_POINT('Origin',(27.9189647353249,83.8,-85.132617134716));
#64635=CARTESIAN_POINT('',(27.9189647353249,83.8,-85.132617134716));
#64636=CARTESIAN_POINT('Origin',(28.3520995377337,83.8,-87.9866892389691));
#64637=CARTESIAN_POINT('',(28.3520995377337,83.8,-87.9866892389691));
#64638=CARTESIAN_POINT('Origin',(31.0403658854537,83.8,-89.0386195489465));
#64639=CARTESIAN_POINT('',(31.0403658854537,83.8,-89.0386195489465));
#64640=CARTESIAN_POINT('Origin',(33.295497430765,83.8,-87.2364777546708));
#64641=CARTESIAN_POINT('Origin',(25.8780417805632,83.8,-81.6494105360638));
#64642=CARTESIAN_POINT('',(25.8780417805632,83.8,-81.6494105360638));
#64643=CARTESIAN_POINT('',(26.3111765829719,83.8,-84.5034826403169));
#64644=CARTESIAN_POINT('Origin',(23.1897754328432,83.8,-80.5974802260864));
#64645=CARTESIAN_POINT('',(23.1897754328432,83.8,-80.5974802260864));
#64646=CARTESIAN_POINT('Origin',(20.9346438875318,83.8,-82.3996220203621));
#64647=CARTESIAN_POINT('',(20.9346438875318,83.8,-82.3996220203621));
#64648=CARTESIAN_POINT('Origin',(21.3677786899405,83.8,-85.2536941246152));
#64649=CARTESIAN_POINT('',(21.3677786899405,83.8,-85.2536941246152));
#64650=CARTESIAN_POINT('Origin',(24.0560450376606,83.8,-86.3056244345926));
#64651=CARTESIAN_POINT('',(24.0560450376606,83.8,-86.3056244345926));
#64652=CARTESIAN_POINT('Origin',(26.3111765829719,83.8,-84.5034826403169));
#64653=CARTESIAN_POINT('Origin',(18.89372093277,83.8,-78.9164154217099));
#64654=CARTESIAN_POINT('',(18.89372093277,83.8,-78.9164154217099));
#64655=CARTESIAN_POINT('',(19.3268557351787,83.8,-81.770487525963));
#64656=CARTESIAN_POINT('Origin',(16.20545458505,83.8,-77.8644851117325));
#64657=CARTESIAN_POINT('',(16.20545458505,83.8,-77.8644851117325));
#64658=CARTESIAN_POINT('Origin',(13.9503230397387,83.8,-79.6666269060082));
#64659=CARTESIAN_POINT('',(13.9503230397387,83.8,-79.6666269060082));
#64660=CARTESIAN_POINT('Origin',(14.3834578421474,83.8,-82.5206990102613));
#64661=CARTESIAN_POINT('',(14.3834578421474,83.8,-82.5206990102613));
#64662=CARTESIAN_POINT('Origin',(17.0717241898674,83.8,-83.5726293202387));
#64663=CARTESIAN_POINT('',(17.0717241898674,83.8,-83.5726293202387));
#64664=CARTESIAN_POINT('Origin',(19.3268557351787,83.8,-81.770487525963));
#64665=CARTESIAN_POINT('Origin',(11.9094000849769,83.8,-76.1834203073561));
#64666=CARTESIAN_POINT('',(11.9094000849769,83.8,-76.1834203073561));
#64667=CARTESIAN_POINT('',(12.3425348873856,83.8,-79.0374924116092));
#64668=CARTESIAN_POINT('Origin',(9.22113373725689,83.8,-75.1314899973787));
#64669=CARTESIAN_POINT('',(9.22113373725689,83.8,-75.1314899973787));
#64670=CARTESIAN_POINT('Origin',(6.96600219194553,83.8,-76.9336317916543));
#64671=CARTESIAN_POINT('',(6.96600219194553,83.8,-76.9336317916543));
#64672=CARTESIAN_POINT('Origin',(7.39913699435427,83.8,-79.7877038959074));
#64673=CARTESIAN_POINT('',(7.39913699435427,83.8,-79.7877038959074));
#64674=CARTESIAN_POINT('Origin',(10.0874033420743,83.8,-80.8396342058848));
#64675=CARTESIAN_POINT('',(10.0874033420743,83.8,-80.8396342058848));
#64676=CARTESIAN_POINT('Origin',(12.3425348873856,83.8,-79.0374924116092));
#64677=CARTESIAN_POINT('Origin',(4.92507923718377,83.8,-73.4504251930022));
#64678=CARTESIAN_POINT('',(4.92507923718377,83.8,-73.4504251930022));
#64679=CARTESIAN_POINT('',(5.35821403959249,83.8,-76.3044972972553));
#64680=CARTESIAN_POINT('Origin',(2.23681288946376,83.8,-72.3984948830248));
#64681=CARTESIAN_POINT('',(2.23681288946376,83.8,-72.3984948830248));
#64682=CARTESIAN_POINT('Origin',(-0.0183186558475948,83.8,-74.2006366773005));
#64683=CARTESIAN_POINT('',(-0.0183186558475948,83.8,-74.2006366773005));
#64684=CARTESIAN_POINT('Origin',(0.414816146561137,83.8,-77.0547087815535));
#64685=CARTESIAN_POINT('',(0.414816146561137,83.8,-77.0547087815535));
#64686=CARTESIAN_POINT('Origin',(3.10308249428116,83.8,-78.1066390915309));
#64687=CARTESIAN_POINT('',(3.10308249428116,83.8,-78.1066390915309));
#64688=CARTESIAN_POINT('Origin',(5.35821403959249,83.8,-76.3044972972553));
#64689=CARTESIAN_POINT('Origin',(-2.05924161060936,83.8,-70.7174300786483));
#64690=CARTESIAN_POINT('',(-2.05924161060936,83.8,-70.7174300786483));
#64691=CARTESIAN_POINT('',(-1.62610680820064,83.8,-73.5715021829014));
#64692=CARTESIAN_POINT('Origin',(-4.74750795832937,83.8,-69.6654997686709));
#64693=CARTESIAN_POINT('',(-4.74750795832937,83.8,-69.6654997686709));
#64694=CARTESIAN_POINT('Origin',(-7.00263950364073,83.8,-71.4676415629466));
#64695=CARTESIAN_POINT('',(-7.00263950364073,83.8,-71.4676415629466));
#64696=CARTESIAN_POINT('Origin',(-6.569504701232,83.8,-74.3217136671996));
#64697=CARTESIAN_POINT('',(-6.569504701232,83.8,-74.3217136671996));
#64698=CARTESIAN_POINT('Origin',(-3.88123835351197,83.8,-75.3736439771771));
#64699=CARTESIAN_POINT('',(-3.88123835351197,83.8,-75.3736439771771));
#64700=CARTESIAN_POINT('Origin',(-1.62610680820064,83.8,-73.5715021829014));
#64701=CARTESIAN_POINT('Origin',(-9.04356245840249,83.8,-67.9844349642944));
#64702=CARTESIAN_POINT('',(-9.04356245840249,83.8,-67.9844349642944));
#64703=CARTESIAN_POINT('',(-8.61042765599378,83.8,-70.8385070685475));
#64704=CARTESIAN_POINT('Origin',(-11.7318288061225,83.8,-66.932504654317));
#64705=CARTESIAN_POINT('',(-11.7318288061225,83.8,-66.932504654317));
#64706=CARTESIAN_POINT('Origin',(-13.9869603514339,83.8,-68.7346464485927));
#64707=CARTESIAN_POINT('',(-13.9869603514339,83.8,-68.7346464485927));
#64708=CARTESIAN_POINT('Origin',(-13.5538255490251,83.8,-71.5887185528457));
#64709=CARTESIAN_POINT('',(-13.5538255490251,83.8,-71.5887185528457));
#64710=CARTESIAN_POINT('Origin',(-10.8655592013051,83.8,-72.6406488628232));
#64711=CARTESIAN_POINT('',(-10.8655592013051,83.8,-72.6406488628232));
#64712=CARTESIAN_POINT('Origin',(-8.61042765599378,83.8,-70.8385070685475));
#64713=CARTESIAN_POINT('Origin',(16.6430864798753,83.8,-64.0862217426158));
#64714=CARTESIAN_POINT('',(16.6430864798753,83.8,-64.0862217426158));
#64715=CARTESIAN_POINT('',(17.076221282284,83.8,-66.940293846869));
#64716=CARTESIAN_POINT('Origin',(13.9548201321553,83.8,-63.0342914326384));
#64717=CARTESIAN_POINT('',(13.9548201321553,83.8,-63.0342914326384));
#64718=CARTESIAN_POINT('Origin',(11.6996885868439,83.8,-64.8364332269141));
#64719=CARTESIAN_POINT('',(11.6996885868439,83.8,-64.8364332269141));
#64720=CARTESIAN_POINT('Origin',(12.1328233892526,83.8,-67.6905053311672));
#64721=CARTESIAN_POINT('',(12.1328233892526,83.8,-67.6905053311672));
#64722=CARTESIAN_POINT('Origin',(14.8210897369727,83.8,-68.7424356411446));
#64723=CARTESIAN_POINT('',(14.8210897369727,83.8,-68.7424356411446));
#64724=CARTESIAN_POINT('Origin',(17.076221282284,83.8,-66.940293846869));
#64725=CARTESIAN_POINT('Origin',(9.65876563208215,83.8,-61.353226628262));
#64726=CARTESIAN_POINT('',(9.65876563208215,83.8,-61.353226628262));
#64727=CARTESIAN_POINT('',(10.0919004344909,83.8,-64.2072987325151));
#64728=CARTESIAN_POINT('Origin',(6.97049928436214,83.8,-60.3012963182845));
#64729=CARTESIAN_POINT('',(6.97049928436214,83.8,-60.3012963182845));
#64730=CARTESIAN_POINT('Origin',(4.71536773905078,83.8,-62.1034381125602));
#64731=CARTESIAN_POINT('',(4.71536773905078,83.8,-62.1034381125602));
#64732=CARTESIAN_POINT('Origin',(5.14850254145952,83.8,-64.9575102168133));
#64733=CARTESIAN_POINT('',(5.14850254145952,83.8,-64.9575102168133));
#64734=CARTESIAN_POINT('Origin',(7.83676888917954,83.8,-66.0094405267907));
#64735=CARTESIAN_POINT('',(7.83676888917954,83.8,-66.0094405267907));
#64736=CARTESIAN_POINT('Origin',(10.0919004344909,83.8,-64.2072987325151));
#64737=CARTESIAN_POINT('Origin',(2.67444478428902,83.8,-58.6202315139081));
#64738=CARTESIAN_POINT('',(2.67444478428902,83.8,-58.6202315139081));
#64739=CARTESIAN_POINT('',(3.10757958669774,83.8,-61.4743036181612));
#64740=CARTESIAN_POINT('Origin',(-0.0138215634309935,83.8,-57.5683012039307));
#64741=CARTESIAN_POINT('',(-0.0138215634309935,83.8,-57.5683012039307));
#64742=CARTESIAN_POINT('Origin',(-2.26895310874235,83.8,-59.3704429982063));
#64743=CARTESIAN_POINT('',(-2.26895310874235,83.8,-59.3704429982063));
#64744=CARTESIAN_POINT('Origin',(-1.83581830633362,83.8,-62.2245151024594));
#64745=CARTESIAN_POINT('',(-1.83581830633362,83.8,-62.2245151024594));
#64746=CARTESIAN_POINT('Origin',(0.852448041386411,83.8,-63.2764454124368));
#64747=CARTESIAN_POINT('',(0.852448041386411,83.8,-63.2764454124368));
#64748=CARTESIAN_POINT('Origin',(3.10757958669774,83.8,-61.4743036181612));
#64749=CARTESIAN_POINT('Origin',(-4.30987606350412,83.8,-55.8872363995542));
#64750=CARTESIAN_POINT('',(-4.30987606350412,83.8,-55.8872363995542));
#64751=CARTESIAN_POINT('',(-3.8767412610954,83.8,-58.7413085038073));
#64752=CARTESIAN_POINT('Origin',(-6.99814241122413,83.8,-54.8353060895768));
#64753=CARTESIAN_POINT('',(-6.99814241122413,83.8,-54.8353060895768));
#64754=CARTESIAN_POINT('Origin',(-9.25327395653548,83.8,-56.6374478838525));
#64755=CARTESIAN_POINT('',(-9.25327395653548,83.8,-56.6374478838525));
#64756=CARTESIAN_POINT('Origin',(-8.82013915412675,83.8,-59.4915199881055));
#64757=CARTESIAN_POINT('',(-8.82013915412675,83.8,-59.4915199881055));
#64758=CARTESIAN_POINT('Origin',(-6.13187280640672,83.8,-60.543450298083));
#64759=CARTESIAN_POINT('',(-6.13187280640672,83.8,-60.543450298083));
#64760=CARTESIAN_POINT('Origin',(-3.8767412610954,83.8,-58.7413085038073));
#64761=CARTESIAN_POINT('Origin',(-11.2941969112972,83.8,-53.1542412852003));
#64762=CARTESIAN_POINT('',(-11.2941969112972,83.8,-53.1542412852003));
#64763=CARTESIAN_POINT('',(-10.8610621088885,83.8,-56.0083133894534));
#64764=CARTESIAN_POINT('Origin',(-13.9824632590173,83.8,-52.1023109752229));
#64765=CARTESIAN_POINT('',(-13.9824632590173,83.8,-52.1023109752229));
#64766=CARTESIAN_POINT('Origin',(-16.2375948043286,83.8,-53.9044527694986));
#64767=CARTESIAN_POINT('',(-16.2375948043286,83.8,-53.9044527694986));
#64768=CARTESIAN_POINT('Origin',(-15.8044600019199,83.8,-56.7585248737516));
#64769=CARTESIAN_POINT('',(-15.8044600019199,83.8,-56.7585248737516));
#64770=CARTESIAN_POINT('Origin',(-13.1161936541999,83.8,-57.8104551837291));
#64771=CARTESIAN_POINT('',(-13.1161936541999,83.8,-57.8104551837291));
#64772=CARTESIAN_POINT('Origin',(-10.8610621088885,83.8,-56.0083133894534));
#64773=CARTESIAN_POINT('Origin',(-18.2785177590904,83.8,-50.4212461708464));
#64774=CARTESIAN_POINT('',(-18.2785177590904,83.8,-50.4212461708464));
#64775=CARTESIAN_POINT('',(-17.8453829566817,83.8,-53.2753182750995));
#64776=CARTESIAN_POINT('Origin',(-20.9667841068104,83.8,-49.369315860869));
#64777=CARTESIAN_POINT('',(-20.9667841068104,83.8,-49.369315860869));
#64778=CARTESIAN_POINT('Origin',(-23.2219156521217,83.8,-51.1714576551447));
#64779=CARTESIAN_POINT('',(-23.2219156521217,83.8,-51.1714576551447));
#64780=CARTESIAN_POINT('Origin',(-22.788780849713,83.8,-54.0255297593977));
#64781=CARTESIAN_POINT('',(-22.788780849713,83.8,-54.0255297593977));
#64782=CARTESIAN_POINT('Origin',(-20.100514501993,83.8,-55.0774600693752));
#64783=CARTESIAN_POINT('',(-20.100514501993,83.8,-55.0774600693752));
#64784=CARTESIAN_POINT('Origin',(-17.8453829566817,83.8,-53.2753182750995));
#64785=CARTESIAN_POINT('Origin',(-25.2628386068835,83.8,-47.6882510564925));
#64786=CARTESIAN_POINT('',(-25.2628386068835,83.8,-47.6882510564925));
#64787=CARTESIAN_POINT('',(-24.8297038044748,83.8,-50.5423231607456));
#64788=CARTESIAN_POINT('Origin',(-27.9511049546035,83.8,-46.6363207465151));
#64789=CARTESIAN_POINT('',(-27.9511049546035,83.8,-46.6363207465151));
#64790=CARTESIAN_POINT('Origin',(-30.2062364999149,83.8,-48.4384625407908));
#64791=CARTESIAN_POINT('',(-30.2062364999149,83.8,-48.4384625407908));
#64792=CARTESIAN_POINT('Origin',(-29.7731016975061,83.8,-51.2925346450439));
#64793=CARTESIAN_POINT('',(-29.7731016975061,83.8,-51.2925346450439));
#64794=CARTESIAN_POINT('Origin',(-27.0848353497861,83.8,-52.3444649550213));
#64795=CARTESIAN_POINT('',(-27.0848353497861,83.8,-52.3444649550213));
#64796=CARTESIAN_POINT('Origin',(-24.8297038044748,83.8,-50.5423231607456));
#64797=CARTESIAN_POINT('Origin',(-32.2471594546766,83.8,-44.9552559421386));
#64798=CARTESIAN_POINT('',(-32.2471594546766,83.8,-44.9552559421386));
#64799=CARTESIAN_POINT('',(-31.8140246522679,83.8,-47.8093280463917));
#64800=CARTESIAN_POINT('Origin',(-34.9354258023966,83.8,-43.9033256321612));
#64801=CARTESIAN_POINT('',(-34.9354258023966,83.8,-43.9033256321612));
#64802=CARTESIAN_POINT('Origin',(-37.190557347708,83.8,-45.7054674264369));
#64803=CARTESIAN_POINT('',(-37.190557347708,83.8,-45.7054674264369));
#64804=CARTESIAN_POINT('Origin',(-36.7574225452993,83.8,-48.55953953069));
#64805=CARTESIAN_POINT('',(-36.7574225452993,83.8,-48.55953953069));
#64806=CARTESIAN_POINT('Origin',(-34.0691561975792,83.8,-49.6114698406674));
#64807=CARTESIAN_POINT('',(-34.0691561975792,83.8,-49.6114698406674));
#64808=CARTESIAN_POINT('Origin',(-31.8140246522679,83.8,-47.8093280463917));
#64809=CARTESIAN_POINT('Origin',(10.7840828585295,83.8,-68.768323467809));
#64810=CARTESIAN_POINT('',(10.7840828585295,83.8,-68.768323467809));
#64811=CARTESIAN_POINT('',(11.2172176609382,83.8,-71.6223955720621));
#64812=CARTESIAN_POINT('Origin',(8.09581651080951,83.8,-67.7163931578316));
#64813=CARTESIAN_POINT('',(8.09581651080951,83.8,-67.7163931578316));
#64814=CARTESIAN_POINT('Origin',(5.84068496549816,83.8,-69.5185349521073));
#64815=CARTESIAN_POINT('',(5.84068496549816,83.8,-69.5185349521073));
#64816=CARTESIAN_POINT('Origin',(6.27381976790689,83.8,-72.3726070563604));
#64817=CARTESIAN_POINT('',(6.27381976790689,83.8,-72.3726070563604));
#64818=CARTESIAN_POINT('Origin',(8.96208611562692,83.8,-73.4245373663378));
#64819=CARTESIAN_POINT('',(8.96208611562692,83.8,-73.4245373663378));
#64820=CARTESIAN_POINT('Origin',(11.2172176609382,83.8,-71.6223955720621));
#64821=CARTESIAN_POINT('Origin',(17.7684037063227,83.8,-71.5013185821629));
#64822=CARTESIAN_POINT('',(17.7684037063227,83.8,-71.5013185821629));
#64823=CARTESIAN_POINT('',(18.2015385087314,83.8,-74.355390686416));
#64824=CARTESIAN_POINT('Origin',(15.0801373586026,83.8,-70.4493882721855));
#64825=CARTESIAN_POINT('',(15.0801373586026,83.8,-70.4493882721855));
#64826=CARTESIAN_POINT('Origin',(12.8250058132913,83.8,-72.2515300664612));
#64827=CARTESIAN_POINT('',(12.8250058132913,83.8,-72.2515300664612));
#64828=CARTESIAN_POINT('Origin',(13.2581406157,83.8,-75.1056021707142));
#64829=CARTESIAN_POINT('',(13.2581406157,83.8,-75.1056021707142));
#64830=CARTESIAN_POINT('Origin',(15.94640696342,83.8,-76.1575324806917));
#64831=CARTESIAN_POINT('',(15.94640696342,83.8,-76.1575324806917));
#64832=CARTESIAN_POINT('Origin',(18.2015385087314,83.8,-74.355390686416));
#64833=CARTESIAN_POINT('Origin',(24.7527245541158,83.8,-74.2343136965168));
#64834=CARTESIAN_POINT('',(24.7527245541158,83.8,-74.2343136965168));
#64835=CARTESIAN_POINT('',(25.1858593565245,83.8,-77.0883858007699));
#64836=CARTESIAN_POINT('Origin',(22.0644582063958,83.8,-73.1823833865394));
#64837=CARTESIAN_POINT('',(22.0644582063958,83.8,-73.1823833865394));
#64838=CARTESIAN_POINT('Origin',(19.8093266610844,83.8,-74.9845251808151));
#64839=CARTESIAN_POINT('',(19.8093266610844,83.8,-74.9845251808151));
#64840=CARTESIAN_POINT('Origin',(20.2424614634932,83.8,-77.8385972850681));
#64841=CARTESIAN_POINT('',(20.2424614634932,83.8,-77.8385972850681));
#64842=CARTESIAN_POINT('Origin',(22.9307278112132,83.8,-78.8905275950456));
#64843=CARTESIAN_POINT('',(22.9307278112132,83.8,-78.8905275950456));
#64844=CARTESIAN_POINT('Origin',(25.1858593565245,83.8,-77.0883858007699));
#64845=CARTESIAN_POINT('Origin',(31.7370454019089,83.8,-76.9673088108707));
#64846=CARTESIAN_POINT('',(31.7370454019089,83.8,-76.9673088108707));
#64847=CARTESIAN_POINT('',(32.1701802043176,83.8,-79.8213809151238));
#64848=CARTESIAN_POINT('Origin',(29.0487790541889,83.8,-75.9153785008933));
#64849=CARTESIAN_POINT('',(29.0487790541889,83.8,-75.9153785008933));
#64850=CARTESIAN_POINT('Origin',(26.7936475088776,83.8,-77.717520295169));
#64851=CARTESIAN_POINT('',(26.7936475088776,83.8,-77.717520295169));
#64852=CARTESIAN_POINT('Origin',(27.2267823112863,83.8,-80.571592399422));
#64853=CARTESIAN_POINT('',(27.2267823112863,83.8,-80.571592399422));
#64854=CARTESIAN_POINT('Origin',(29.9150486590063,83.8,-81.6235227093995));
#64855=CARTESIAN_POINT('',(29.9150486590063,83.8,-81.6235227093995));
#64856=CARTESIAN_POINT('Origin',(32.1701802043176,83.8,-79.8213809151238));
#64857=CARTESIAN_POINT('Origin',(-39.2314803024698,83.8,-42.2222608277847));
#64858=CARTESIAN_POINT('',(-39.2314803024698,83.8,-42.2222608277847));
#64859=CARTESIAN_POINT('',(-38.798345500061,83.8,-45.0763329320378));
#64860=CARTESIAN_POINT('Origin',(-41.9197466501898,83.8,-41.1703305178073));
#64861=CARTESIAN_POINT('',(-41.9197466501898,83.8,-41.1703305178073));
#64862=CARTESIAN_POINT('Origin',(-44.1748781955011,83.8,-42.972472312083));
#64863=CARTESIAN_POINT('',(-44.1748781955011,83.8,-42.972472312083));
#64864=CARTESIAN_POINT('Origin',(-43.7417433930924,83.8,-45.8265444163361));
#64865=CARTESIAN_POINT('',(-43.7417433930924,83.8,-45.8265444163361));
#64866=CARTESIAN_POINT('Origin',(-41.0534770453724,83.8,-46.8784747263135));
#64867=CARTESIAN_POINT('',(-41.0534770453724,83.8,-46.8784747263135));
#64868=CARTESIAN_POINT('Origin',(-38.798345500061,83.8,-45.0763329320378));
#64869=CARTESIAN_POINT('Origin',(52.6900079452883,83.8,-85.1662941539323));
#64870=CARTESIAN_POINT('',(52.6900079452883,83.8,-85.1662941539323));
#64871=CARTESIAN_POINT('',(53.123142747697,83.8,-88.0203662581854));
#64872=CARTESIAN_POINT('Origin',(50.0017415975683,83.8,-84.1143638439549));
#64873=CARTESIAN_POINT('',(50.0017415975683,83.8,-84.1143638439549));
#64874=CARTESIAN_POINT('Origin',(47.7466100522569,83.8,-85.9165056382306));
#64875=CARTESIAN_POINT('',(47.7466100522569,83.8,-85.9165056382306));
#64876=CARTESIAN_POINT('Origin',(48.1797448546657,83.8,-88.7705777424837));
#64877=CARTESIAN_POINT('',(48.1797448546657,83.8,-88.7705777424837));
#64878=CARTESIAN_POINT('Origin',(50.8680112023857,83.8,-89.8225080524611));
#64879=CARTESIAN_POINT('',(50.8680112023857,83.8,-89.8225080524611));
#64880=CARTESIAN_POINT('Origin',(53.123142747697,83.8,-88.0203662581854));
#64881=CARTESIAN_POINT('Origin',(45.7056870974952,83.8,-82.4332990395785));
#64882=CARTESIAN_POINT('',(45.7056870974952,83.8,-82.4332990395785));
#64883=CARTESIAN_POINT('',(46.1388218999039,83.8,-85.2873711438316));
#64884=CARTESIAN_POINT('Origin',(43.0174207497752,83.8,-81.381368729601));
#64885=CARTESIAN_POINT('',(43.0174207497752,83.8,-81.381368729601));
#64886=CARTESIAN_POINT('Origin',(40.7622892044638,83.8,-83.1835105238767));
#64887=CARTESIAN_POINT('',(40.7622892044638,83.8,-83.1835105238767));
#64888=CARTESIAN_POINT('Origin',(41.1954240068725,83.8,-86.0375826281298));
#64889=CARTESIAN_POINT('',(41.1954240068725,83.8,-86.0375826281298));
#64890=CARTESIAN_POINT('Origin',(43.8836903545926,83.8,-87.0895129381072));
#64891=CARTESIAN_POINT('',(43.8836903545926,83.8,-87.0895129381072));
#64892=CARTESIAN_POINT('Origin',(46.1388218999039,83.8,-85.2873711438316));
#64893=CARTESIAN_POINT('Origin',(38.721366249702,83.8,-79.7003039252246));
#64894=CARTESIAN_POINT('',(38.721366249702,83.8,-79.7003039252246));
#64895=CARTESIAN_POINT('',(39.1545010521108,83.8,-82.5543760294777));
#64896=CARTESIAN_POINT('Origin',(36.033099901982,83.8,-78.6483736152472));
#64897=CARTESIAN_POINT('',(36.033099901982,83.8,-78.6483736152472));
#64898=CARTESIAN_POINT('Origin',(33.7779683566707,83.8,-80.4505154095229));
#64899=CARTESIAN_POINT('',(33.7779683566707,83.8,-80.4505154095229));
#64900=CARTESIAN_POINT('Origin',(34.2111031590794,83.8,-83.3045875137759));
#64901=CARTESIAN_POINT('',(34.2111031590794,83.8,-83.3045875137759));
#64902=CARTESIAN_POINT('Origin',(36.8993695067994,83.8,-84.3565178237533));
#64903=CARTESIAN_POINT('',(36.8993695067994,83.8,-84.3565178237533));
#64904=CARTESIAN_POINT('Origin',(39.1545010521108,83.8,-82.5543760294777));
#64905=CARTESIAN_POINT('Origin',(14.1600345378716,83.8,-91.0136139864502));
#64906=CARTESIAN_POINT('',(14.1600345378716,83.8,-91.0136139864502));
#64907=CARTESIAN_POINT('',(14.5931693402804,83.8,-93.8676860907033));
#64908=CARTESIAN_POINT('Origin',(11.4717681901516,83.8,-89.9616836764728));
#64909=CARTESIAN_POINT('',(11.4717681901516,83.8,-89.9616836764728));
#64910=CARTESIAN_POINT('Origin',(9.21663664484028,83.8,-91.7638254707484));
#64911=CARTESIAN_POINT('',(9.21663664484028,83.8,-91.7638254707484));
#64912=CARTESIAN_POINT('Origin',(9.64977144724901,83.8,-94.6178975750015));
#64913=CARTESIAN_POINT('',(9.64977144724901,83.8,-94.6178975750015));
#64914=CARTESIAN_POINT('Origin',(12.338037794969,83.8,-95.6698278849789));
#64915=CARTESIAN_POINT('',(12.338037794969,83.8,-95.6698278849789));
#64916=CARTESIAN_POINT('Origin',(14.5931693402804,83.8,-93.8676860907033));
#64917=CARTESIAN_POINT('Origin',(21.1443553856648,83.8,-93.7466091008041));
#64918=CARTESIAN_POINT('',(21.1443553856648,83.8,-93.7466091008041));
#64919=CARTESIAN_POINT('',(21.5774901880735,83.8,-96.6006812050572));
#64920=CARTESIAN_POINT('Origin',(18.4560890379448,83.8,-92.6946787908267));
#64921=CARTESIAN_POINT('',(18.4560890379448,83.8,-92.6946787908267));
#64922=CARTESIAN_POINT('Origin',(16.2009574926334,83.8,-94.4968205851023));
#64923=CARTESIAN_POINT('',(16.2009574926334,83.8,-94.4968205851023));
#64924=CARTESIAN_POINT('Origin',(16.6340922950421,83.8,-97.3508926893554));
#64925=CARTESIAN_POINT('',(16.6340922950421,83.8,-97.3508926893554));
#64926=CARTESIAN_POINT('Origin',(19.3223586427622,83.8,-98.4028229993328));
#64927=CARTESIAN_POINT('',(19.3223586427622,83.8,-98.4028229993328));
#64928=CARTESIAN_POINT('Origin',(21.5774901880735,83.8,-96.6006812050572));
#64929=CARTESIAN_POINT('Origin',(28.1286762334579,83.8,-96.479604215158));
#64930=CARTESIAN_POINT('',(28.1286762334579,83.8,-96.479604215158));
#64931=CARTESIAN_POINT('',(28.5618110358666,83.8,-99.3336763194111));
#64932=CARTESIAN_POINT('Origin',(25.4404098857379,83.8,-95.4276739051805));
#64933=CARTESIAN_POINT('',(25.4404098857379,83.8,-95.4276739051805));
#64934=CARTESIAN_POINT('Origin',(23.1852783404265,83.8,-97.2298156994562));
#64935=CARTESIAN_POINT('',(23.1852783404265,83.8,-97.2298156994562));
#64936=CARTESIAN_POINT('Origin',(23.6184131428353,83.8,-100.083887803709));
#64937=CARTESIAN_POINT('',(23.6184131428353,83.8,-100.083887803709));
#64938=CARTESIAN_POINT('Origin',(26.3066794905553,83.8,-101.135818113687));
#64939=CARTESIAN_POINT('',(26.3066794905553,83.8,-101.135818113687));
#64940=CARTESIAN_POINT('Origin',(28.5618110358666,83.8,-99.3336763194111));
#64941=CARTESIAN_POINT('Origin',(35.112997081251,83.8,-99.2125993295118));
#64942=CARTESIAN_POINT('',(35.112997081251,83.8,-99.2125993295118));
#64943=CARTESIAN_POINT('',(35.5461318836598,83.8,-102.066671433765));
#64944=CARTESIAN_POINT('Origin',(32.424730733531,83.8,-98.1606690195344));
#64945=CARTESIAN_POINT('',(32.424730733531,83.8,-98.1606690195344));
#64946=CARTESIAN_POINT('Origin',(30.1695991882197,83.8,-99.9628108138101));
#64947=CARTESIAN_POINT('',(30.1695991882197,83.8,-99.9628108138101));
#64948=CARTESIAN_POINT('Origin',(30.6027339906284,83.8,-102.816882918063));
#64949=CARTESIAN_POINT('',(30.6027339906284,83.8,-102.816882918063));
#64950=CARTESIAN_POINT('Origin',(33.2910003383484,83.8,-103.868813228041));
#64951=CARTESIAN_POINT('',(33.2910003383484,83.8,-103.868813228041));
#64952=CARTESIAN_POINT('Origin',(35.5461318836598,83.8,-102.066671433765));
#64953=CARTESIAN_POINT('Origin',(-28.8712077753345,83.8,-67.2005464607798));
#64954=CARTESIAN_POINT('',(-28.8712077753345,83.8,-67.2005464607798));
#64955=CARTESIAN_POINT('',(-28.4380729729258,83.8,-70.0546185650329));
#64956=CARTESIAN_POINT('Origin',(-31.5594741230545,83.8,-66.1486161508024));
#64957=CARTESIAN_POINT('',(-31.5594741230545,83.8,-66.1486161508024));
#64958=CARTESIAN_POINT('Origin',(-33.8146056683659,83.8,-67.9507579450781));
#64959=CARTESIAN_POINT('',(-33.8146056683659,83.8,-67.9507579450781));
#64960=CARTESIAN_POINT('Origin',(-33.3814708659571,83.8,-70.8048300493311));
#64961=CARTESIAN_POINT('',(-33.3814708659571,83.8,-70.8048300493311));
#64962=CARTESIAN_POINT('Origin',(-30.6932045182371,83.8,-71.8567603593086));
#64963=CARTESIAN_POINT('',(-30.6932045182371,83.8,-71.8567603593086));
#64964=CARTESIAN_POINT('Origin',(-28.4380729729258,83.8,-70.0546185650329));
#64965=CARTESIAN_POINT('Origin',(-35.8555286231276,83.8,-64.4675513464259));
#64966=CARTESIAN_POINT('',(-35.8555286231276,83.8,-64.4675513464259));
#64967=CARTESIAN_POINT('',(-35.4223938207189,83.8,-67.321623450679));
#64968=CARTESIAN_POINT('Origin',(-38.5437949708476,83.8,-63.4156210364485));
#64969=CARTESIAN_POINT('',(-38.5437949708476,83.8,-63.4156210364485));
#64970=CARTESIAN_POINT('Origin',(-40.798926516159,83.8,-65.2177628307242));
#64971=CARTESIAN_POINT('',(-40.798926516159,83.8,-65.2177628307242));
#64972=CARTESIAN_POINT('Origin',(-40.3657917137503,83.8,-68.0718349349772));
#64973=CARTESIAN_POINT('',(-40.3657917137503,83.8,-68.0718349349772));
#64974=CARTESIAN_POINT('Origin',(-37.6775253660303,83.8,-69.1237652449547));
#64975=CARTESIAN_POINT('',(-37.6775253660303,83.8,-69.1237652449547));
#64976=CARTESIAN_POINT('Origin',(-35.4223938207189,83.8,-67.321623450679));
#64977=CARTESIAN_POINT('Origin',(-42.8398494709208,83.8,-61.734556232072));
#64978=CARTESIAN_POINT('',(-42.8398494709208,83.8,-61.734556232072));
#64979=CARTESIAN_POINT('',(-42.4067146685121,83.8,-64.5886283363251));
#64980=CARTESIAN_POINT('Origin',(-45.5281158186408,83.8,-60.6826259220946));
#64981=CARTESIAN_POINT('',(-45.5281158186408,83.8,-60.6826259220946));
#64982=CARTESIAN_POINT('Origin',(-47.7832473639521,83.8,-62.4847677163703));
#64983=CARTESIAN_POINT('',(-47.7832473639521,83.8,-62.4847677163703));
#64984=CARTESIAN_POINT('Origin',(-47.3501125615434,83.8,-65.3388398206233));
#64985=CARTESIAN_POINT('',(-47.3501125615434,83.8,-65.3388398206233));
#64986=CARTESIAN_POINT('Origin',(-44.6618462138234,83.8,-66.3907701306008));
#64987=CARTESIAN_POINT('',(-44.6618462138234,83.8,-66.3907701306008));
#64988=CARTESIAN_POINT('Origin',(-42.4067146685121,83.8,-64.5886283363251));
#64989=CARTESIAN_POINT('Origin',(42.0973179290442,83.8,-101.945594443866));
#64990=CARTESIAN_POINT('',(42.0973179290442,83.8,-101.945594443866));
#64991=CARTESIAN_POINT('',(42.5304527314529,83.8,-104.799666548119));
#64992=CARTESIAN_POINT('Origin',(39.4090515813242,83.8,-100.893664133888));
#64993=CARTESIAN_POINT('',(39.4090515813242,83.8,-100.893664133888));
#64994=CARTESIAN_POINT('Origin',(37.1539200360128,83.8,-102.695805928164));
#64995=CARTESIAN_POINT('',(37.1539200360128,83.8,-102.695805928164));
#64996=CARTESIAN_POINT('Origin',(37.5870548384215,83.8,-105.549878032417));
#64997=CARTESIAN_POINT('',(37.5870548384215,83.8,-105.549878032417));
#64998=CARTESIAN_POINT('Origin',(40.2753211861416,83.8,-106.601808342394));
#64999=CARTESIAN_POINT('',(40.2753211861416,83.8,-106.601808342394));
#65000=CARTESIAN_POINT('Origin',(42.5304527314529,83.8,-104.799666548119));
#65001=CARTESIAN_POINT('Origin',(7.17571369007852,83.8,-88.2806188720963));
#65002=CARTESIAN_POINT('',(7.17571369007852,83.8,-88.2806188720963));
#65003=CARTESIAN_POINT('',(7.60884849248723,83.8,-91.1346909763494));
#65004=CARTESIAN_POINT('Origin',(4.4874473423585,83.8,-87.2286885621189));
#65005=CARTESIAN_POINT('',(4.4874473423585,83.8,-87.2286885621189));
#65006=CARTESIAN_POINT('Origin',(2.23231579704715,83.8,-89.0308303563946));
#65007=CARTESIAN_POINT('',(2.23231579704715,83.8,-89.0308303563946));
#65008=CARTESIAN_POINT('Origin',(2.66545059945588,83.8,-91.8849024606476));
#65009=CARTESIAN_POINT('',(2.66545059945588,83.8,-91.8849024606476));
#65010=CARTESIAN_POINT('Origin',(5.35371694717591,83.8,-92.936832770625));
#65011=CARTESIAN_POINT('',(5.35371694717591,83.8,-92.936832770625));
#65012=CARTESIAN_POINT('Origin',(7.60884849248723,83.8,-91.1346909763494));
#65013=CARTESIAN_POINT('Origin',(0.191392842285382,83.8,-85.5476237577424));
#65014=CARTESIAN_POINT('',(0.191392842285382,83.8,-85.5476237577424));
#65015=CARTESIAN_POINT('',(0.6245276446941,83.8,-88.4016958619955));
#65016=CARTESIAN_POINT('Origin',(-2.49687350543463,83.8,-84.495693447765));
#65017=CARTESIAN_POINT('',(-2.49687350543463,83.8,-84.495693447765));
#65018=CARTESIAN_POINT('Origin',(-4.75200505074598,83.8,-86.2978352420407));
#65019=CARTESIAN_POINT('',(-4.75200505074598,83.8,-86.2978352420407));
#65020=CARTESIAN_POINT('Origin',(-4.31887024833725,83.8,-89.1519073462937));
#65021=CARTESIAN_POINT('',(-4.31887024833725,83.8,-89.1519073462937));
#65022=CARTESIAN_POINT('Origin',(-1.63060390061722,83.8,-90.2038376562712));
#65023=CARTESIAN_POINT('',(-1.63060390061722,83.8,-90.2038376562712));
#65024=CARTESIAN_POINT('Origin',(0.6245276446941,83.8,-88.4016958619955));
#65025=CARTESIAN_POINT('Origin',(-6.79292800550775,83.8,-82.8146286433885));
#65026=CARTESIAN_POINT('',(-6.79292800550775,83.8,-82.8146286433885));
#65027=CARTESIAN_POINT('',(-6.35979320309903,83.8,-85.6687007476416));
#65028=CARTESIAN_POINT('Origin',(-9.48119435322776,83.8,-81.7626983334111));
#65029=CARTESIAN_POINT('',(-9.48119435322776,83.8,-81.7626983334111));
#65030=CARTESIAN_POINT('Origin',(-11.7363258985391,83.8,-83.5648401276868));
#65031=CARTESIAN_POINT('',(-11.7363258985391,83.8,-83.5648401276868));
#65032=CARTESIAN_POINT('Origin',(-11.3031910961304,83.8,-86.4189122319399));
#65033=CARTESIAN_POINT('',(-11.3031910961304,83.8,-86.4189122319399));
#65034=CARTESIAN_POINT('Origin',(-8.61492474841036,83.8,-87.4708425419173));
#65035=CARTESIAN_POINT('',(-8.61492474841036,83.8,-87.4708425419173));
#65036=CARTESIAN_POINT('Origin',(-6.35979320309903,83.8,-85.6687007476416));
#65037=CARTESIAN_POINT('Origin',(-13.7772488533009,83.8,-80.0816335290346));
#65038=CARTESIAN_POINT('',(-13.7772488533009,83.8,-80.0816335290346));
#65039=CARTESIAN_POINT('',(-13.3441140508922,83.8,-82.9357056332877));
#65040=CARTESIAN_POINT('Origin',(-16.4655152010209,83.8,-79.0297032190572));
#65041=CARTESIAN_POINT('',(-16.4655152010209,83.8,-79.0297032190572));
#65042=CARTESIAN_POINT('Origin',(-18.7206467463322,83.8,-80.8318450133329));
#65043=CARTESIAN_POINT('',(-18.7206467463322,83.8,-80.8318450133329));
#65044=CARTESIAN_POINT('Origin',(-18.2875119439235,83.8,-83.685917117586));
#65045=CARTESIAN_POINT('',(-18.2875119439235,83.8,-83.685917117586));
#65046=CARTESIAN_POINT('Origin',(-15.5992455962035,83.8,-84.7378474275634));
#65047=CARTESIAN_POINT('',(-15.5992455962035,83.8,-84.7378474275634));
#65048=CARTESIAN_POINT('Origin',(-13.3441140508922,83.8,-82.9357056332877));
#65049=CARTESIAN_POINT('Origin',(-20.761569701094,83.8,-77.3486384146807));
#65050=CARTESIAN_POINT('',(-20.761569701094,83.8,-77.3486384146807));
#65051=CARTESIAN_POINT('',(-20.3284348986853,83.8,-80.2027105189338));
#65052=CARTESIAN_POINT('Origin',(-23.449836048814,83.8,-76.2967081047033));
#65053=CARTESIAN_POINT('',(-23.449836048814,83.8,-76.2967081047033));
#65054=CARTESIAN_POINT('Origin',(-25.7049675941254,83.8,-78.098849898979));
#65055=CARTESIAN_POINT('',(-25.7049675941254,83.8,-78.098849898979));
#65056=CARTESIAN_POINT('Origin',(-25.2718327917166,83.8,-80.9529220032321));
#65057=CARTESIAN_POINT('',(-25.2718327917166,83.8,-80.9529220032321));
#65058=CARTESIAN_POINT('Origin',(-22.5835664439966,83.8,-82.0048523132095));
#65059=CARTESIAN_POINT('',(-22.5835664439966,83.8,-82.0048523132095));
#65060=CARTESIAN_POINT('Origin',(-20.3284348986853,83.8,-80.2027105189338));
#65061=CARTESIAN_POINT('Origin',(-27.7458905488871,83.8,-74.6156433003268));
#65062=CARTESIAN_POINT('',(-27.7458905488871,83.8,-74.6156433003268));
#65063=CARTESIAN_POINT('',(-27.3127557464784,83.8,-77.4697154045799));
#65064=CARTESIAN_POINT('Origin',(-30.4341568966072,83.8,-73.5637129903494));
#65065=CARTESIAN_POINT('',(-30.4341568966072,83.8,-73.5637129903494));
#65066=CARTESIAN_POINT('Origin',(-32.6892884419185,83.8,-75.3658547846251));
#65067=CARTESIAN_POINT('',(-32.6892884419185,83.8,-75.3658547846251));
#65068=CARTESIAN_POINT('Origin',(-32.2561536395098,83.8,-78.2199268888782));
#65069=CARTESIAN_POINT('',(-32.2561536395098,83.8,-78.2199268888782));
#65070=CARTESIAN_POINT('Origin',(-29.5678872917897,83.8,-79.2718571988556));
#65071=CARTESIAN_POINT('',(-29.5678872917897,83.8,-79.2718571988556));
#65072=CARTESIAN_POINT('Origin',(-27.3127557464784,83.8,-77.4697154045799));
#65073=CARTESIAN_POINT('Origin',(-34.7302113966803,83.8,-71.8826481859729));
#65074=CARTESIAN_POINT('',(-34.7302113966803,83.8,-71.8826481859729));
#65075=CARTESIAN_POINT('',(-34.2970765942716,83.8,-74.7367202902261));
#65076=CARTESIAN_POINT('Origin',(-37.4184777444003,83.8,-70.8307178759955));
#65077=CARTESIAN_POINT('',(-37.4184777444003,83.8,-70.8307178759955));
#65078=CARTESIAN_POINT('Origin',(-39.6736092897116,83.8,-72.6328596702712));
#65079=CARTESIAN_POINT('',(-39.6736092897116,83.8,-72.6328596702712));
#65080=CARTESIAN_POINT('Origin',(-39.2404744873029,83.8,-75.4869317745243));
#65081=CARTESIAN_POINT('',(-39.2404744873029,83.8,-75.4869317745243));
#65082=CARTESIAN_POINT('Origin',(-36.5522081395829,83.8,-76.5388620845017));
#65083=CARTESIAN_POINT('',(-36.5522081395829,83.8,-76.5388620845017));
#65084=CARTESIAN_POINT('Origin',(-34.2970765942716,83.8,-74.7367202902261));
#65085=CARTESIAN_POINT('Origin',(-41.7145322444734,83.8,-69.1496530716191));
#65086=CARTESIAN_POINT('',(-41.7145322444734,83.8,-69.1496530716191));
#65087=CARTESIAN_POINT('',(-41.2813974420647,83.8,-72.0037251758721));
#65088=CARTESIAN_POINT('Origin',(-44.4027985921934,83.8,-68.0977227616416));
#65089=CARTESIAN_POINT('',(-44.4027985921934,83.8,-68.0977227616416));
#65090=CARTESIAN_POINT('Origin',(-46.6579301375048,83.8,-69.8998645559173));
#65091=CARTESIAN_POINT('',(-46.6579301375048,83.8,-69.8998645559173));
#65092=CARTESIAN_POINT('Origin',(-46.224795335096,83.8,-72.7539366601704));
#65093=CARTESIAN_POINT('',(-46.224795335096,83.8,-72.7539366601704));
#65094=CARTESIAN_POINT('Origin',(-43.536528987376,83.8,-73.8058669701478));
#65095=CARTESIAN_POINT('',(-43.536528987376,83.8,-73.8058669701478));
#65096=CARTESIAN_POINT('Origin',(-41.2813974420647,83.8,-72.0037251758721));
#65097=CARTESIAN_POINT('Origin',(-43.9651666973681,83.8,-54.3194593925249));
#65098=CARTESIAN_POINT('',(-43.9651666973681,83.8,-54.3194593925249));
#65099=CARTESIAN_POINT('',(-43.5320318949594,83.8,-57.1735314967781));
#65100=CARTESIAN_POINT('Origin',(-46.6534330450882,83.8,-53.2675290825475));
#65101=CARTESIAN_POINT('',(-46.6534330450882,83.8,-53.2675290825475));
#65102=CARTESIAN_POINT('Origin',(-48.9085645903995,83.8,-55.0696708768232));
#65103=CARTESIAN_POINT('',(-48.9085645903995,83.8,-55.0696708768232));
#65104=CARTESIAN_POINT('Origin',(-48.4754297879908,83.8,-57.9237429810763));
#65105=CARTESIAN_POINT('',(-48.4754297879908,83.8,-57.9237429810763));
#65106=CARTESIAN_POINT('Origin',(-45.7871634402707,83.8,-58.9756732910537));
#65107=CARTESIAN_POINT('',(-45.7871634402707,83.8,-58.9756732910537));
#65108=CARTESIAN_POINT('Origin',(-43.5320318949594,83.8,-57.1735314967781));
#65109=CARTESIAN_POINT('Origin',(47.9563215503899,83.8,-97.2634927186726));
#65110=CARTESIAN_POINT('',(47.9563215503899,83.8,-97.2634927186726));
#65111=CARTESIAN_POINT('',(48.3894563527986,83.8,-100.117564822926));
#65112=CARTESIAN_POINT('Origin',(45.2680552026699,83.8,-96.2115624086952));
#65113=CARTESIAN_POINT('',(45.2680552026699,83.8,-96.2115624086952));
#65114=CARTESIAN_POINT('Origin',(43.0129236573585,83.8,-98.0137042029708));
#65115=CARTESIAN_POINT('',(43.0129236573585,83.8,-98.0137042029708));
#65116=CARTESIAN_POINT('Origin',(43.4460584597673,83.8,-100.867776307224));
#65117=CARTESIAN_POINT('',(43.4460584597673,83.8,-100.867776307224));
#65118=CARTESIAN_POINT('Origin',(46.1343248074873,83.8,-101.919706617201));
#65119=CARTESIAN_POINT('',(46.1343248074873,83.8,-101.919706617201));
#65120=CARTESIAN_POINT('Origin',(48.3894563527986,83.8,-100.117564822926));
#65121=CARTESIAN_POINT('Origin',(40.9720007025968,83.8,-94.5304976043187));
#65122=CARTESIAN_POINT('',(40.9720007025968,83.8,-94.5304976043187));
#65123=CARTESIAN_POINT('',(41.4051355050055,83.8,-97.3845697085718));
#65124=CARTESIAN_POINT('Origin',(38.2837343548768,83.8,-93.4785672943413));
#65125=CARTESIAN_POINT('',(38.2837343548768,83.8,-93.4785672943413));
#65126=CARTESIAN_POINT('Origin',(36.0286028095654,83.8,-95.280709088617));
#65127=CARTESIAN_POINT('',(36.0286028095654,83.8,-95.280709088617));
#65128=CARTESIAN_POINT('Origin',(36.4617376119742,83.8,-98.13478119287));
#65129=CARTESIAN_POINT('',(36.4617376119742,83.8,-98.13478119287));
#65130=CARTESIAN_POINT('Origin',(39.1500039596942,83.8,-99.1867115028474));
#65131=CARTESIAN_POINT('',(39.1500039596942,83.8,-99.1867115028474));
#65132=CARTESIAN_POINT('Origin',(41.4051355050055,83.8,-97.3845697085718));
#65133=CARTESIAN_POINT('Origin',(33.9876798548037,83.8,-91.7975024899648));
#65134=CARTESIAN_POINT('',(33.9876798548037,83.8,-91.7975024899648));
#65135=CARTESIAN_POINT('',(34.4208146572124,83.8,-94.6515745942179));
#65136=CARTESIAN_POINT('Origin',(31.2994135070836,83.8,-90.7455721799874));
#65137=CARTESIAN_POINT('',(31.2994135070836,83.8,-90.7455721799874));
#65138=CARTESIAN_POINT('Origin',(29.0442819617723,83.8,-92.5477139742631));
#65139=CARTESIAN_POINT('',(29.0442819617723,83.8,-92.5477139742631));
#65140=CARTESIAN_POINT('Origin',(29.477416764181,83.8,-95.4017860785161));
#65141=CARTESIAN_POINT('',(29.477416764181,83.8,-95.4017860785161));
#65142=CARTESIAN_POINT('Origin',(32.1656831119011,83.8,-96.4537163884935));
#65143=CARTESIAN_POINT('',(32.1656831119011,83.8,-96.4537163884935));
#65144=CARTESIAN_POINT('Origin',(34.4208146572124,83.8,-94.6515745942179));
#65145=CARTESIAN_POINT('Origin',(-36.980845849575,83.8,-57.0524545068788));
#65146=CARTESIAN_POINT('',(-36.980845849575,83.8,-57.0524545068788));
#65147=CARTESIAN_POINT('',(-36.5477110471663,83.8,-59.9065266111319));
#65148=CARTESIAN_POINT('Origin',(-39.669112197295,83.8,-56.0005241969014));
#65149=CARTESIAN_POINT('',(-39.669112197295,83.8,-56.0005241969014));
#65150=CARTESIAN_POINT('Origin',(-41.9242437426064,83.8,-57.8026659911771));
#65151=CARTESIAN_POINT('',(-41.9242437426064,83.8,-57.8026659911771));
#65152=CARTESIAN_POINT('Origin',(-41.4911089401976,83.8,-60.6567380954302));
#65153=CARTESIAN_POINT('',(-41.4911089401976,83.8,-60.6567380954302));
#65154=CARTESIAN_POINT('Origin',(-38.8028425924776,83.8,-61.7086684054076));
#65155=CARTESIAN_POINT('',(-38.8028425924776,83.8,-61.7086684054076));
#65156=CARTESIAN_POINT('Origin',(-36.5477110471663,83.8,-59.9065266111319));
#65157=CARTESIAN_POINT('Origin',(-29.9965250017819,83.8,-59.7854496212327));
#65158=CARTESIAN_POINT('',(-29.9965250017819,83.8,-59.7854496212327));
#65159=CARTESIAN_POINT('',(-29.5633901993732,83.8,-62.6395217254858));
#65160=CARTESIAN_POINT('Origin',(-32.6847913495019,83.8,-58.7335193112553));
#65161=CARTESIAN_POINT('',(-32.6847913495019,83.8,-58.7335193112553));
#65162=CARTESIAN_POINT('Origin',(-34.9399228948133,83.8,-60.535661105531));
#65163=CARTESIAN_POINT('',(-34.9399228948133,83.8,-60.535661105531));
#65164=CARTESIAN_POINT('Origin',(-34.5067880924045,83.8,-63.3897332097841));
#65165=CARTESIAN_POINT('',(-34.5067880924045,83.8,-63.3897332097841));
#65166=CARTESIAN_POINT('Origin',(-31.8185217446845,83.8,-64.4416635197615));
#65167=CARTESIAN_POINT('',(-31.8185217446845,83.8,-64.4416635197615));
#65168=CARTESIAN_POINT('Origin',(-29.5633901993732,83.8,-62.6395217254858));
#65169=CARTESIAN_POINT('Origin',(-23.0122041539888,83.8,-62.5184447355866));
#65170=CARTESIAN_POINT('',(-23.0122041539888,83.8,-62.5184447355866));
#65171=CARTESIAN_POINT('',(-22.57906935158,83.8,-65.3725168398397));
#65172=CARTESIAN_POINT('Origin',(-25.7004705017088,83.8,-61.4665144256092));
#65173=CARTESIAN_POINT('',(-25.7004705017088,83.8,-61.4665144256092));
#65174=CARTESIAN_POINT('Origin',(-27.9556020470201,83.8,-63.2686562198849));
#65175=CARTESIAN_POINT('',(-27.9556020470201,83.8,-63.2686562198849));
#65176=CARTESIAN_POINT('Origin',(-27.5224672446114,83.8,-66.122728324138));
#65177=CARTESIAN_POINT('',(-27.5224672446114,83.8,-66.122728324138));
#65178=CARTESIAN_POINT('Origin',(-24.8342008968914,83.8,-67.1746586341154));
#65179=CARTESIAN_POINT('',(-24.8342008968914,83.8,-67.1746586341154));
#65180=CARTESIAN_POINT('Origin',(-22.57906935158,83.8,-65.3725168398397));
#65181=CARTESIAN_POINT('Origin',(-16.0278833061956,83.8,-65.2514398499405));
#65182=CARTESIAN_POINT('',(-16.0278833061956,83.8,-65.2514398499405));
#65183=CARTESIAN_POINT('',(-15.5947485037869,83.8,-68.1055119541936));
#65184=CARTESIAN_POINT('Origin',(-18.7161496539156,83.8,-64.1995095399631));
#65185=CARTESIAN_POINT('',(-18.7161496539156,83.8,-64.1995095399631));
#65186=CARTESIAN_POINT('Origin',(-20.971281199227,83.8,-66.0016513342388));
#65187=CARTESIAN_POINT('',(-20.971281199227,83.8,-66.0016513342388));
#65188=CARTESIAN_POINT('Origin',(-20.5381463968183,83.8,-68.8557234384919));
#65189=CARTESIAN_POINT('',(-20.5381463968183,83.8,-68.8557234384919));
#65190=CARTESIAN_POINT('Origin',(-17.8498800490982,83.8,-69.9076537484693));
#65191=CARTESIAN_POINT('',(-17.8498800490982,83.8,-69.9076537484693));
#65192=CARTESIAN_POINT('Origin',(-15.5947485037869,83.8,-68.1055119541936));
#65193=CARTESIAN_POINT('Origin',(27.0033590070105,83.8,-89.0645073756109));
#65194=CARTESIAN_POINT('',(27.0033590070105,83.8,-89.0645073756109));
#65195=CARTESIAN_POINT('',(27.4364938094193,83.8,-91.918579479864));
#65196=CARTESIAN_POINT('Origin',(24.3150926592905,83.8,-88.0125770656335));
#65197=CARTESIAN_POINT('',(24.3150926592905,83.8,-88.0125770656335));
#65198=CARTESIAN_POINT('Origin',(22.0599611139792,83.8,-89.8147188599092));
#65199=CARTESIAN_POINT('',(22.0599611139792,83.8,-89.8147188599092));
#65200=CARTESIAN_POINT('Origin',(22.4930959163879,83.8,-92.6687909641622));
#65201=CARTESIAN_POINT('',(22.4930959163879,83.8,-92.6687909641622));
#65202=CARTESIAN_POINT('Origin',(25.1813622641079,83.8,-93.7207212741397));
#65203=CARTESIAN_POINT('',(25.1813622641079,83.8,-93.7207212741397));
#65204=CARTESIAN_POINT('Origin',(27.4364938094193,83.8,-91.918579479864));
#65205=CARTESIAN_POINT('Origin',(20.0190381592174,83.8,-86.331512261257));
#65206=CARTESIAN_POINT('',(20.0190381592174,83.8,-86.331512261257));
#65207=CARTESIAN_POINT('',(20.4521729616261,83.8,-89.1855843655101));
#65208=CARTESIAN_POINT('Origin',(17.3307718114974,83.8,-85.2795819512796));
#65209=CARTESIAN_POINT('',(17.3307718114974,83.8,-85.2795819512796));
#65210=CARTESIAN_POINT('Origin',(15.075640266186,83.8,-87.0817237455553));
#65211=CARTESIAN_POINT('',(15.075640266186,83.8,-87.0817237455553));
#65212=CARTESIAN_POINT('Origin',(15.5087750685948,83.8,-89.9357958498083));
#65213=CARTESIAN_POINT('',(15.5087750685948,83.8,-89.9357958498083));
#65214=CARTESIAN_POINT('Origin',(18.1970414163148,83.8,-90.9877261597858));
#65215=CARTESIAN_POINT('',(18.1970414163148,83.8,-90.9877261597858));
#65216=CARTESIAN_POINT('Origin',(20.4521729616261,83.8,-89.1855843655101));
#65217=CARTESIAN_POINT('Origin',(13.0347173114243,83.8,-83.5985171469031));
#65218=CARTESIAN_POINT('',(13.0347173114243,83.8,-83.5985171469031));
#65219=CARTESIAN_POINT('',(13.467852113833,83.8,-86.4525892511562));
#65220=CARTESIAN_POINT('Origin',(10.3464509637043,83.8,-82.5465868369257));
#65221=CARTESIAN_POINT('',(10.3464509637043,83.8,-82.5465868369257));
#65222=CARTESIAN_POINT('Origin',(8.09131941839291,83.8,-84.3487286312014));
#65223=CARTESIAN_POINT('',(8.09131941839291,83.8,-84.3487286312014));
#65224=CARTESIAN_POINT('Origin',(8.52445422080164,83.8,-87.2028007354545));
#65225=CARTESIAN_POINT('',(8.52445422080164,83.8,-87.2028007354545));
#65226=CARTESIAN_POINT('Origin',(11.2127205685217,83.8,-88.2547310454319));
#65227=CARTESIAN_POINT('',(11.2127205685217,83.8,-88.2547310454319));
#65228=CARTESIAN_POINT('Origin',(13.467852113833,83.8,-86.4525892511562));
#65229=CARTESIAN_POINT('Origin',(6.05039646363115,83.8,-80.8655220325492));
#65230=CARTESIAN_POINT('',(6.05039646363115,83.8,-80.8655220325492));
#65231=CARTESIAN_POINT('',(6.48353126603986,83.8,-83.7195941368023));
#65232=CARTESIAN_POINT('Origin',(3.36213011591114,83.8,-79.8135917225718));
#65233=CARTESIAN_POINT('',(3.36213011591114,83.8,-79.8135917225718));
#65234=CARTESIAN_POINT('Origin',(1.10699857059978,83.8,-81.6157335168475));
#65235=CARTESIAN_POINT('',(1.10699857059978,83.8,-81.6157335168475));
#65236=CARTESIAN_POINT('Origin',(1.54013337300851,83.8,-84.4698056211006));
#65237=CARTESIAN_POINT('',(1.54013337300851,83.8,-84.4698056211006));
#65238=CARTESIAN_POINT('Origin',(4.22839972072854,83.8,-85.521735931078));
#65239=CARTESIAN_POINT('',(4.22839972072854,83.8,-85.521735931078));
#65240=CARTESIAN_POINT('Origin',(6.48353126603986,83.8,-83.7195941368023));
#65241=CARTESIAN_POINT('Origin',(-0.933924384161986,83.8,-78.1325269181953));
#65242=CARTESIAN_POINT('',(-0.933924384161986,83.8,-78.1325269181953));
#65243=CARTESIAN_POINT('',(-0.500789581753269,83.8,-80.9865990224485));
#65244=CARTESIAN_POINT('Origin',(-3.622190731882,83.8,-77.0805966082179));
#65245=CARTESIAN_POINT('',(-3.622190731882,83.8,-77.0805966082179));
#65246=CARTESIAN_POINT('Origin',(-5.87732227719335,83.8,-78.8827384024936));
#65247=CARTESIAN_POINT('',(-5.87732227719335,83.8,-78.8827384024936));
#65248=CARTESIAN_POINT('Origin',(-5.44418747478462,83.8,-81.7368105067467));
#65249=CARTESIAN_POINT('',(-5.44418747478462,83.8,-81.7368105067467));
#65250=CARTESIAN_POINT('Origin',(-2.75592112706459,83.8,-82.7887408167241));
#65251=CARTESIAN_POINT('',(-2.75592112706459,83.8,-82.7887408167241));
#65252=CARTESIAN_POINT('Origin',(-0.500789581753269,83.8,-80.9865990224485));
#65253=CARTESIAN_POINT('Origin',(-7.91824523195512,83.8,-75.3995318038414));
#65254=CARTESIAN_POINT('',(-7.91824523195512,83.8,-75.3995318038414));
#65255=CARTESIAN_POINT('',(-7.4851104295464,83.8,-78.2536039080945));
#65256=CARTESIAN_POINT('Origin',(-10.6065115796751,83.8,-74.347601493864));
#65257=CARTESIAN_POINT('',(-10.6065115796751,83.8,-74.347601493864));
#65258=CARTESIAN_POINT('Origin',(-12.8616431249865,83.8,-76.1497432881397));
#65259=CARTESIAN_POINT('',(-12.8616431249865,83.8,-76.1497432881397));
#65260=CARTESIAN_POINT('Origin',(-12.4285083225778,83.8,-79.0038153923928));
#65261=CARTESIAN_POINT('',(-12.4285083225778,83.8,-79.0038153923928));
#65262=CARTESIAN_POINT('Origin',(-9.74024197485773,83.8,-80.0557457023702));
#65263=CARTESIAN_POINT('',(-9.74024197485773,83.8,-80.0557457023702));
#65264=CARTESIAN_POINT('Origin',(-7.4851104295464,83.8,-78.2536039080945));
#65265=CARTESIAN_POINT('Origin',(-14.9025660797482,83.8,-72.6665366894876));
#65266=CARTESIAN_POINT('',(-14.9025660797482,83.8,-72.6665366894876));
#65267=CARTESIAN_POINT('',(-14.4694312773395,83.8,-75.5206087937407));
#65268=CARTESIAN_POINT('Origin',(-17.5908324274683,83.8,-71.6146063795101));
#65269=CARTESIAN_POINT('',(-17.5908324274683,83.8,-71.6146063795101));
#65270=CARTESIAN_POINT('Origin',(-19.8459639727796,83.8,-73.4167481737858));
#65271=CARTESIAN_POINT('',(-19.8459639727796,83.8,-73.4167481737858));
#65272=CARTESIAN_POINT('Origin',(-19.4128291703709,83.8,-76.2708202780389));
#65273=CARTESIAN_POINT('',(-19.4128291703709,83.8,-76.2708202780389));
#65274=CARTESIAN_POINT('Origin',(-16.7245628226509,83.8,-77.3227505880163));
#65275=CARTESIAN_POINT('',(-16.7245628226509,83.8,-77.3227505880163));
#65276=CARTESIAN_POINT('Origin',(-14.4694312773395,83.8,-75.5206087937407));
#65277=CARTESIAN_POINT('Origin',(-21.8868869275414,83.8,-69.9335415751337));
#65278=CARTESIAN_POINT('',(-21.8868869275414,83.8,-69.9335415751337));
#65279=CARTESIAN_POINT('',(-21.4537521251327,83.8,-72.7876136793868));
#65280=CARTESIAN_POINT('Origin',(-24.5751532752614,83.8,-68.8816112651563));
#65281=CARTESIAN_POINT('',(-24.5751532752614,83.8,-68.8816112651563));
#65282=CARTESIAN_POINT('Origin',(-26.8302848205727,83.8,-70.683753059432));
#65283=CARTESIAN_POINT('',(-26.8302848205727,83.8,-70.683753059432));
#65284=CARTESIAN_POINT('Origin',(-26.397150018164,83.8,-73.537825163685));
#65285=CARTESIAN_POINT('',(-26.397150018164,83.8,-73.537825163685));
#65286=CARTESIAN_POINT('Origin',(-23.708883670444,83.8,-74.5897554736624));
#65287=CARTESIAN_POINT('',(-23.708883670444,83.8,-74.5897554736624));
#65288=CARTESIAN_POINT('Origin',(-21.4537521251327,83.8,-72.7876136793868));
#65289=CARTESIAN_POINT('',(42.5167202179974,15.1665315209774,72.6737901242527));
#65290=CARTESIAN_POINT('',(80.8492202179974,87.0556842128227,157.935763443077));
#65291=CARTESIAN_POINT('',(112.516720260722,87.7473091544726,158.163001726627));
#65292=CARTESIAN_POINT('',(42.5167202179974,15.1665315209774,157.063790124253));
#65293=UNCERTAINTY_MEASURE_WITH_UNIT(LENGTH_MEASURE(0.01),#65305,
'DISTANCE_ACCURACY_VALUE',
'Maximum model space distance between geometric entities at asserted c
onnectivities');
#65294=UNCERTAINTY_MEASURE_WITH_UNIT(LENGTH_MEASURE(0.01),#65305,
'DISTANCE_ACCURACY_VALUE',
'Maximum model space distance between geometric entities at asserted c
onnectivities');
#65295=UNCERTAINTY_MEASURE_WITH_UNIT(LENGTH_MEASURE(0.01),#65305,
'DISTANCE_ACCURACY_VALUE',
'Maximum model space distance between geometric entities at asserted c
onnectivities');
#65296=UNCERTAINTY_MEASURE_WITH_UNIT(LENGTH_MEASURE(0.01),#65305,
'DISTANCE_ACCURACY_VALUE',
'Maximum model space distance between geometric entities at asserted c
onnectivities');
#65297=UNCERTAINTY_MEASURE_WITH_UNIT(LENGTH_MEASURE(0.01),#65305,
'DISTANCE_ACCURACY_VALUE',
'Maximum model space distance between geometric entities at asserted c
onnectivities');
#65298=UNCERTAINTY_MEASURE_WITH_UNIT(LENGTH_MEASURE(0.01),#65305,
'DISTANCE_ACCURACY_VALUE',
'Maximum model space distance between geometric entities at asserted c
onnectivities');
#65299=(
GEOMETRIC_REPRESENTATION_CONTEXT(3)
GLOBAL_UNCERTAINTY_ASSIGNED_CONTEXT((#65293))
GLOBAL_UNIT_ASSIGNED_CONTEXT((#65305,#65307,#65308))
REPRESENTATION_CONTEXT('','3D')
);
#65300=(
GEOMETRIC_REPRESENTATION_CONTEXT(3)
GLOBAL_UNCERTAINTY_ASSIGNED_CONTEXT((#65294))
GLOBAL_UNIT_ASSIGNED_CONTEXT((#65305,#65307,#65308))
REPRESENTATION_CONTEXT('','3D')
);
#65301=(
GEOMETRIC_REPRESENTATION_CONTEXT(3)
GLOBAL_UNCERTAINTY_ASSIGNED_CONTEXT((#65295))
GLOBAL_UNIT_ASSIGNED_CONTEXT((#65305,#65307,#65308))
REPRESENTATION_CONTEXT('','3D')
);
#65302=(
GEOMETRIC_REPRESENTATION_CONTEXT(3)
GLOBAL_UNCERTAINTY_ASSIGNED_CONTEXT((#65296))
GLOBAL_UNIT_ASSIGNED_CONTEXT((#65305,#65307,#65308))
REPRESENTATION_CONTEXT('','3D')
);
#65303=(
GEOMETRIC_REPRESENTATION_CONTEXT(3)
GLOBAL_UNCERTAINTY_ASSIGNED_CONTEXT((#65297))
GLOBAL_UNIT_ASSIGNED_CONTEXT((#65305,#65307,#65308))
REPRESENTATION_CONTEXT('','3D')
);
#65304=(
GEOMETRIC_REPRESENTATION_CONTEXT(3)
GLOBAL_UNCERTAINTY_ASSIGNED_CONTEXT((#65298))
GLOBAL_UNIT_ASSIGNED_CONTEXT((#65305,#65307,#65308))
REPRESENTATION_CONTEXT('','3D')
);
#65305=(
LENGTH_UNIT()
NAMED_UNIT(*)
SI_UNIT(.MILLI.,.METRE.)
);
#65306=(
LENGTH_UNIT()
NAMED_UNIT(*)
SI_UNIT($,.METRE.)
);
#65307=(
NAMED_UNIT(*)
PLANE_ANGLE_UNIT()
SI_UNIT($,.RADIAN.)
);
#65308=(
NAMED_UNIT(*)
SI_UNIT($,.STERADIAN.)
SOLID_ANGLE_UNIT()
);
#65309=SHAPE_DEFINITION_REPRESENTATION(#65314,#65323);
#65310=SHAPE_DEFINITION_REPRESENTATION(#65315,#65324);
#65311=SHAPE_DEFINITION_REPRESENTATION(#65316,#65325);
#65312=SHAPE_DEFINITION_REPRESENTATION(#65317,#65326);
#65313=SHAPE_DEFINITION_REPRESENTATION(#65318,#65327);
#65314=PRODUCT_DEFINITION_SHAPE('',$,#65329);
#65315=PRODUCT_DEFINITION_SHAPE('',$,#65330);
#65316=PRODUCT_DEFINITION_SHAPE('',$,#65331);
#65317=PRODUCT_DEFINITION_SHAPE('',$,#65332);
#65318=PRODUCT_DEFINITION_SHAPE('',$,#65333);
#65319=PRODUCT_DEFINITION_SHAPE($,$,#23);
#65320=PRODUCT_DEFINITION_SHAPE($,$,#24);
#65321=PRODUCT_DEFINITION_SHAPE($,$,#25);
#65322=PRODUCT_DEFINITION_SHAPE($,$,#26);
#65323=SHAPE_REPRESENTATION('',(#39983,#42510,#42511,#42512,#42513),#65299);
#65324=SHAPE_REPRESENTATION('',(#39984),#65300);
#65325=SHAPE_REPRESENTATION('',(#41041),#65301);
#65326=SHAPE_REPRESENTATION('',(#41224),#65302);
#65327=SHAPE_REPRESENTATION('',(#41307),#65303);
#65328=PRODUCT_DEFINITION_CONTEXT('part definition',#65345,'design');
#65329=PRODUCT_DEFINITION('MAS-688','MAS-688',#65334,#65328);
#65330=PRODUCT_DEFINITION('Sheet Metal Down','Sheet Metal Down',#65335,
#65328);
#65331=PRODUCT_DEFINITION('AC Connector','AC Connector',#65336,#65328);
#65332=PRODUCT_DEFINITION('Swich_Predeterminado','Swich_Predeterminado',
#65337,#65328);
#65333=PRODUCT_DEFINITION('Sheet Metal Up','Sheet Metal Up',#65338,#65328);
#65334=PRODUCT_DEFINITION_FORMATION('',$,#65347);
#65335=PRODUCT_DEFINITION_FORMATION('',$,#65348);
#65336=PRODUCT_DEFINITION_FORMATION('',$,#65349);
#65337=PRODUCT_DEFINITION_FORMATION('',$,#65350);
#65338=PRODUCT_DEFINITION_FORMATION('',$,#65351);
#65339=PRODUCT_RELATED_PRODUCT_CATEGORY('MAS-688','MAS-688',(#65347));
#65340=PRODUCT_RELATED_PRODUCT_CATEGORY('Sheet Metal Down',
'Sheet Metal Down',(#65348));
#65341=PRODUCT_RELATED_PRODUCT_CATEGORY('AC Connector','AC Connector',(#65349));
#65342=PRODUCT_RELATED_PRODUCT_CATEGORY('Swich_Predeterminado',
'Swich_Predeterminado',(#65350));
#65343=PRODUCT_RELATED_PRODUCT_CATEGORY('Sheet Metal Up',
'Sheet Metal Up',(#65351));
#65344=APPLICATION_PROTOCOL_DEFINITION('international standard',
'automotive_design',2009,#65345);
#65345=APPLICATION_CONTEXT(
'Core Data for Automotive Mechanical Design Process');
#65346=PRODUCT_CONTEXT('part definition',#65345,'mechanical');
#65347=PRODUCT('MAS-688','MAS-688','STEP AP214',(#65346));
#65348=PRODUCT('Sheet Metal Down','Sheet Metal Down',$,(#65346));
#65349=PRODUCT('AC Connector','AC Connector',$,(#65346));
#65350=PRODUCT('Swich_Predeterminado','Swich_Predeterminado',$,(#65346));
#65351=PRODUCT('Sheet Metal Up','Sheet Metal Up',$,(#65346));
#65352=PRESENTATION_STYLE_ASSIGNMENT((#65357));
#65353=PRESENTATION_STYLE_ASSIGNMENT((#65358));
#65354=PRESENTATION_STYLE_ASSIGNMENT((#65359));
#65355=PRESENTATION_STYLE_ASSIGNMENT((#65360));
#65356=PRESENTATION_STYLE_ASSIGNMENT((#65361));
#65357=SURFACE_STYLE_USAGE(.BOTH.,#65362);
#65358=SURFACE_STYLE_USAGE(.BOTH.,#65363);
#65359=SURFACE_STYLE_USAGE(.BOTH.,#65364);
#65360=SURFACE_STYLE_USAGE(.BOTH.,#65365);
#65361=SURFACE_STYLE_USAGE(.BOTH.,#65366);
#65362=SURFACE_SIDE_STYLE('',(#65367));
#65363=SURFACE_SIDE_STYLE('',(#65368));
#65364=SURFACE_SIDE_STYLE('',(#65369));
#65365=SURFACE_SIDE_STYLE('',(#65370));
#65366=SURFACE_SIDE_STYLE('',(#65371));
#65367=SURFACE_STYLE_FILL_AREA(#65372);
#65368=SURFACE_STYLE_FILL_AREA(#65373);
#65369=SURFACE_STYLE_FILL_AREA(#65374);
#65370=SURFACE_STYLE_FILL_AREA(#65375);
#65371=SURFACE_STYLE_FILL_AREA(#65376);
#65372=FILL_AREA_STYLE('Steel - Satin',(#65377));
#65373=FILL_AREA_STYLE('Opaque(104,114,127)',(#65378));
#65374=FILL_AREA_STYLE('Opaque(23,69,131)',(#65379));
#65375=FILL_AREA_STYLE('Opaque(81,175,227)',(#65380));
#65376=FILL_AREA_STYLE('Opaque(169,212,242)',(#65381));
#65377=FILL_AREA_STYLE_COLOUR('Steel - Satin',#65382);
#65378=FILL_AREA_STYLE_COLOUR('Opaque(104,114,127)',#65383);
#65379=FILL_AREA_STYLE_COLOUR('Opaque(23,69,131)',#65384);
#65380=FILL_AREA_STYLE_COLOUR('Opaque(81,175,227)',#65385);
#65381=FILL_AREA_STYLE_COLOUR('Opaque(169,212,242)',#65386);
#65382=COLOUR_RGB('Steel - Satin',0.627450980392157,0.627450980392157,0.627450980392157);
#65383=COLOUR_RGB('Opaque(104,114,127)',0.407843137254902,0.447058823529412,
0.498039215686275);
#65384=COLOUR_RGB('Opaque(23,69,131)',0.0901960784313725,0.270588235294118,
0.513725490196078);
#65385=COLOUR_RGB('Opaque(81,175,227)',0.317647058823529,0.686274509803922,
0.890196078431372);
#65386=COLOUR_RGB('Opaque(169,212,242)',0.662745098039216,0.831372549019608,
0.949019607843137);
ENDSEC;
END-ISO-10303-21;
